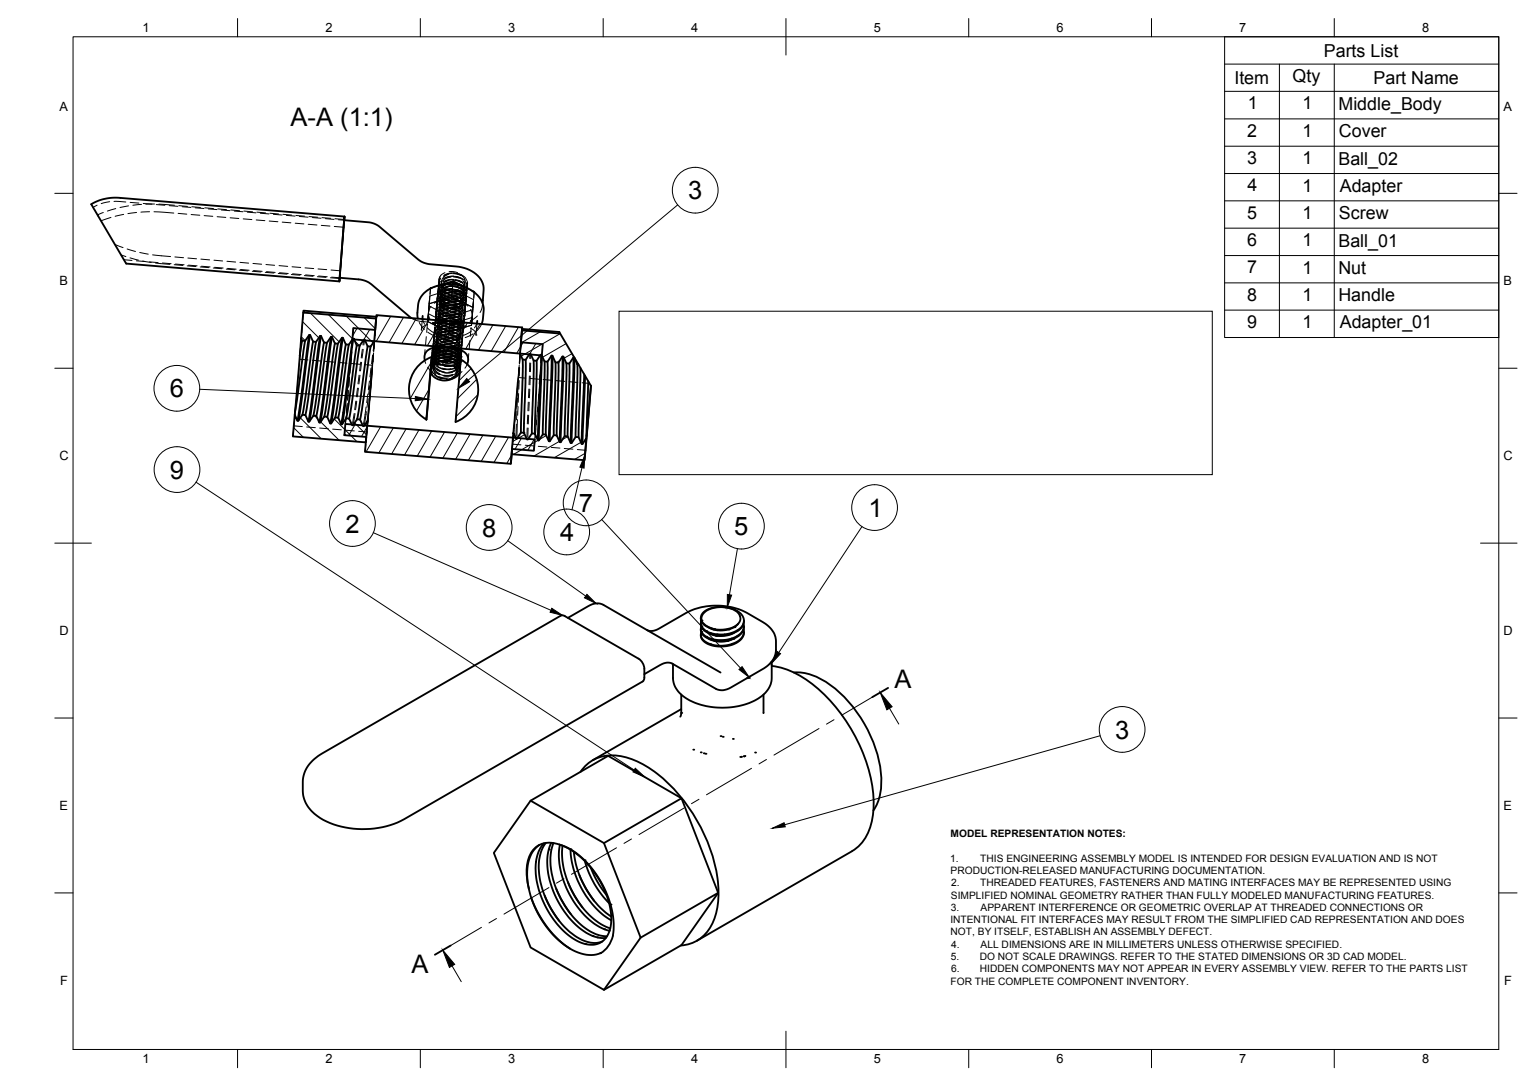
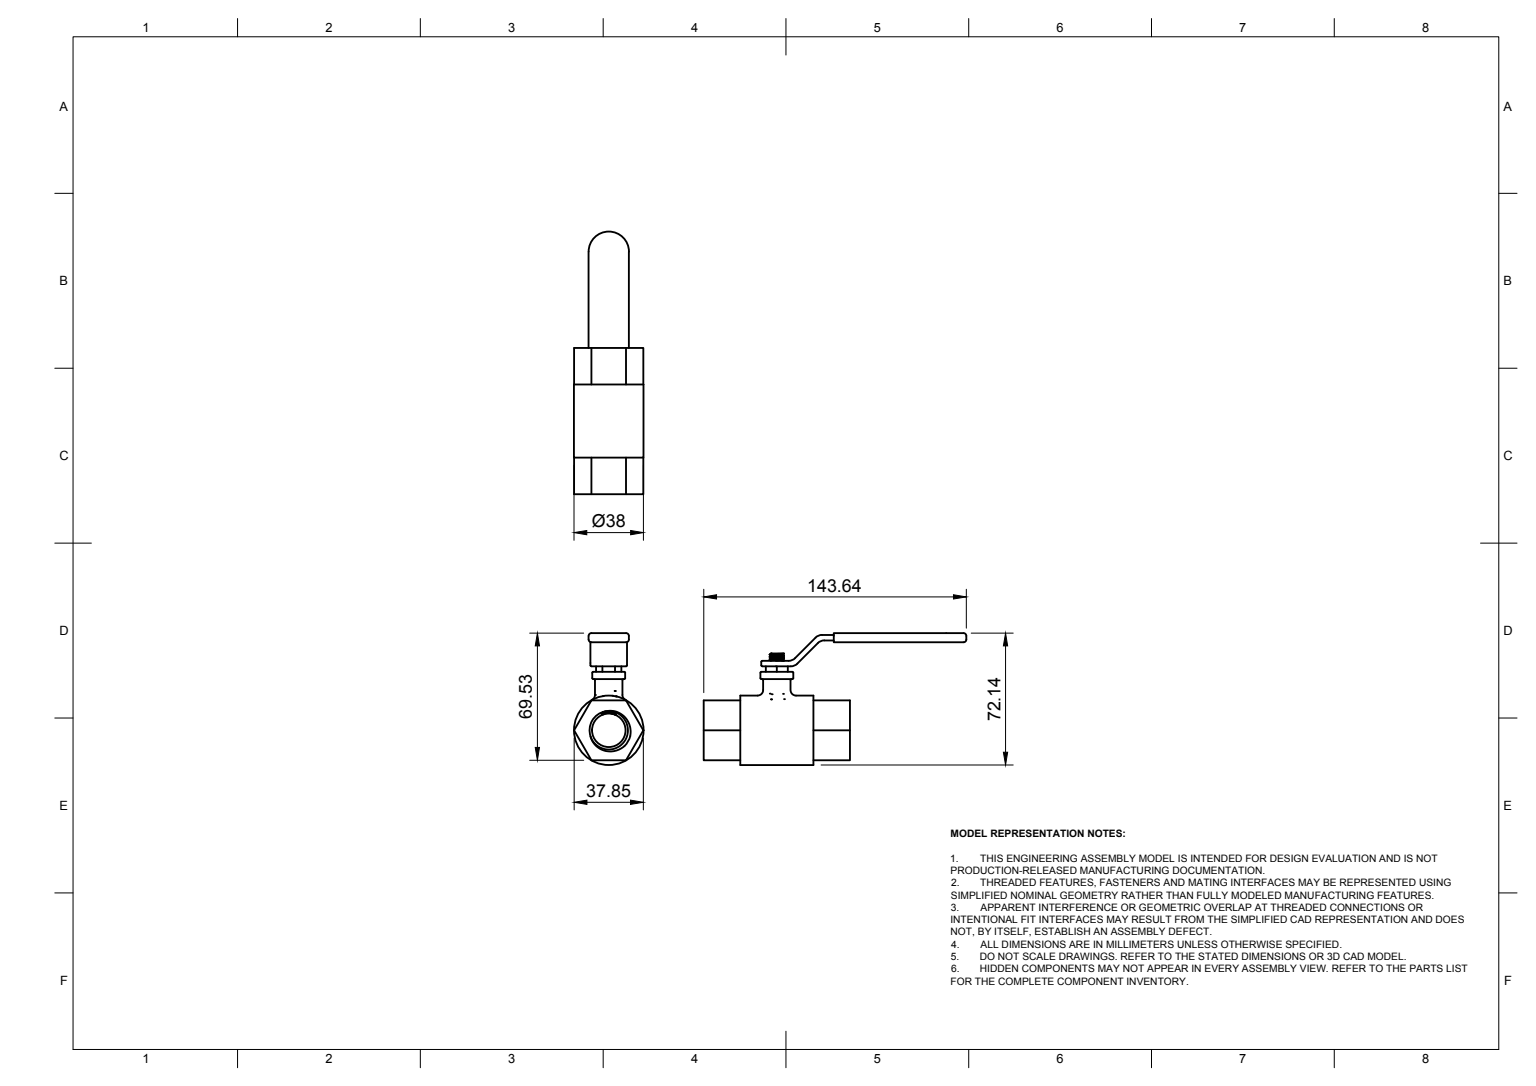
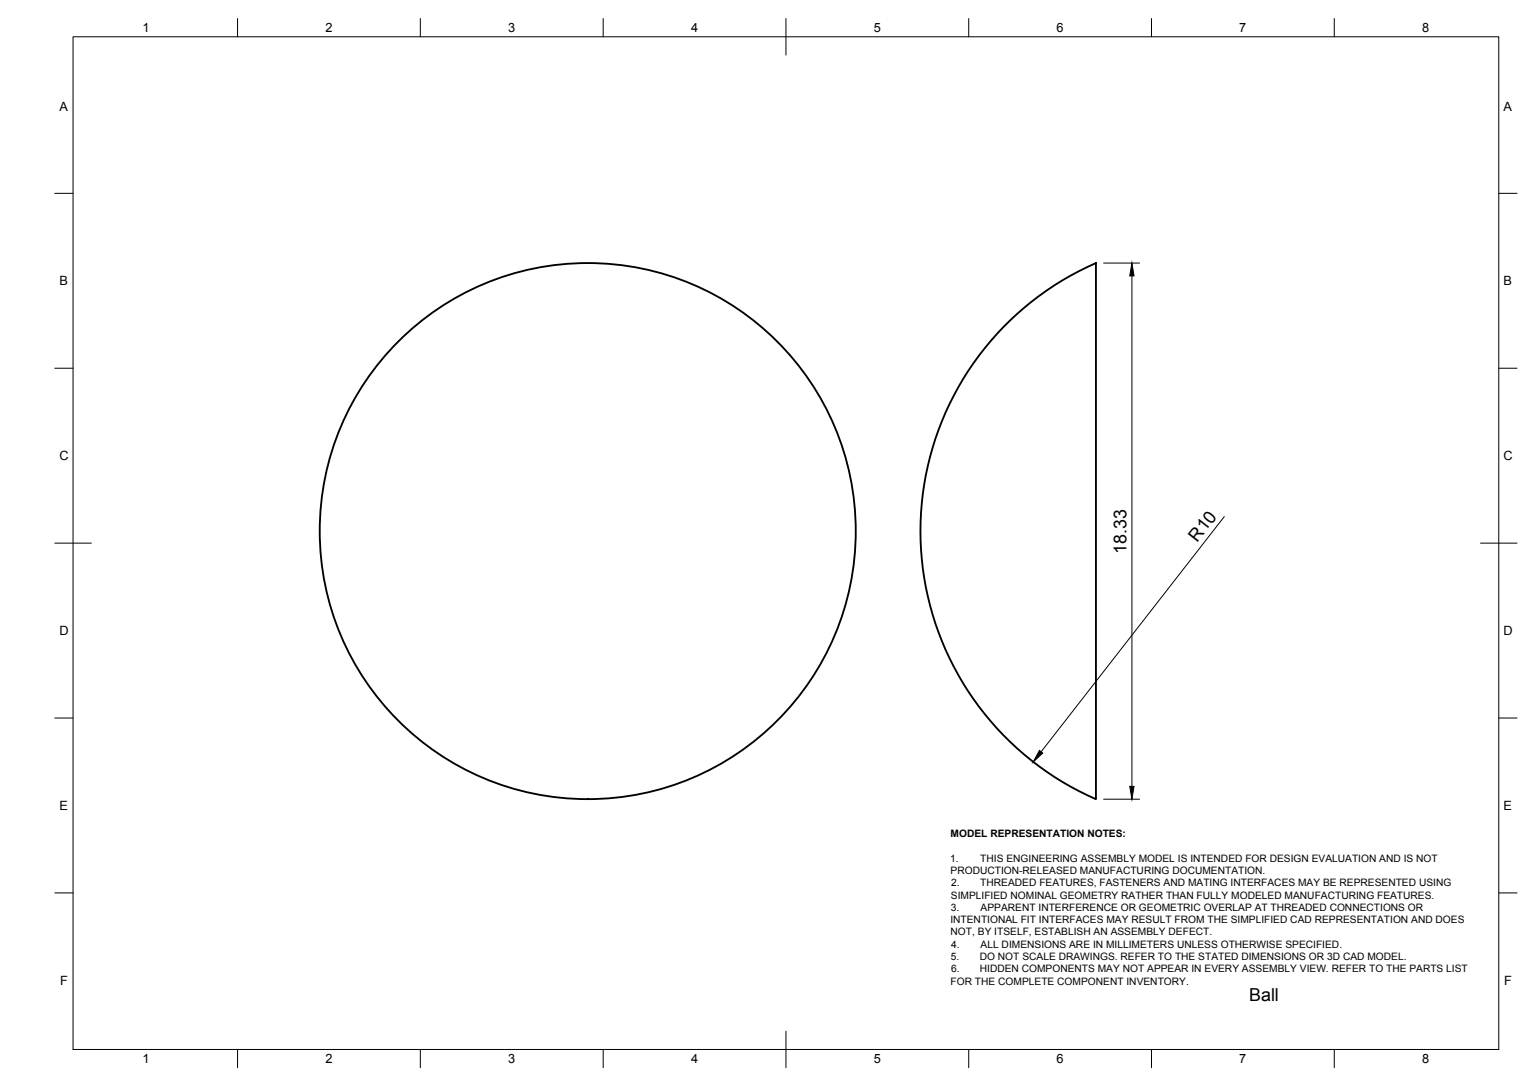
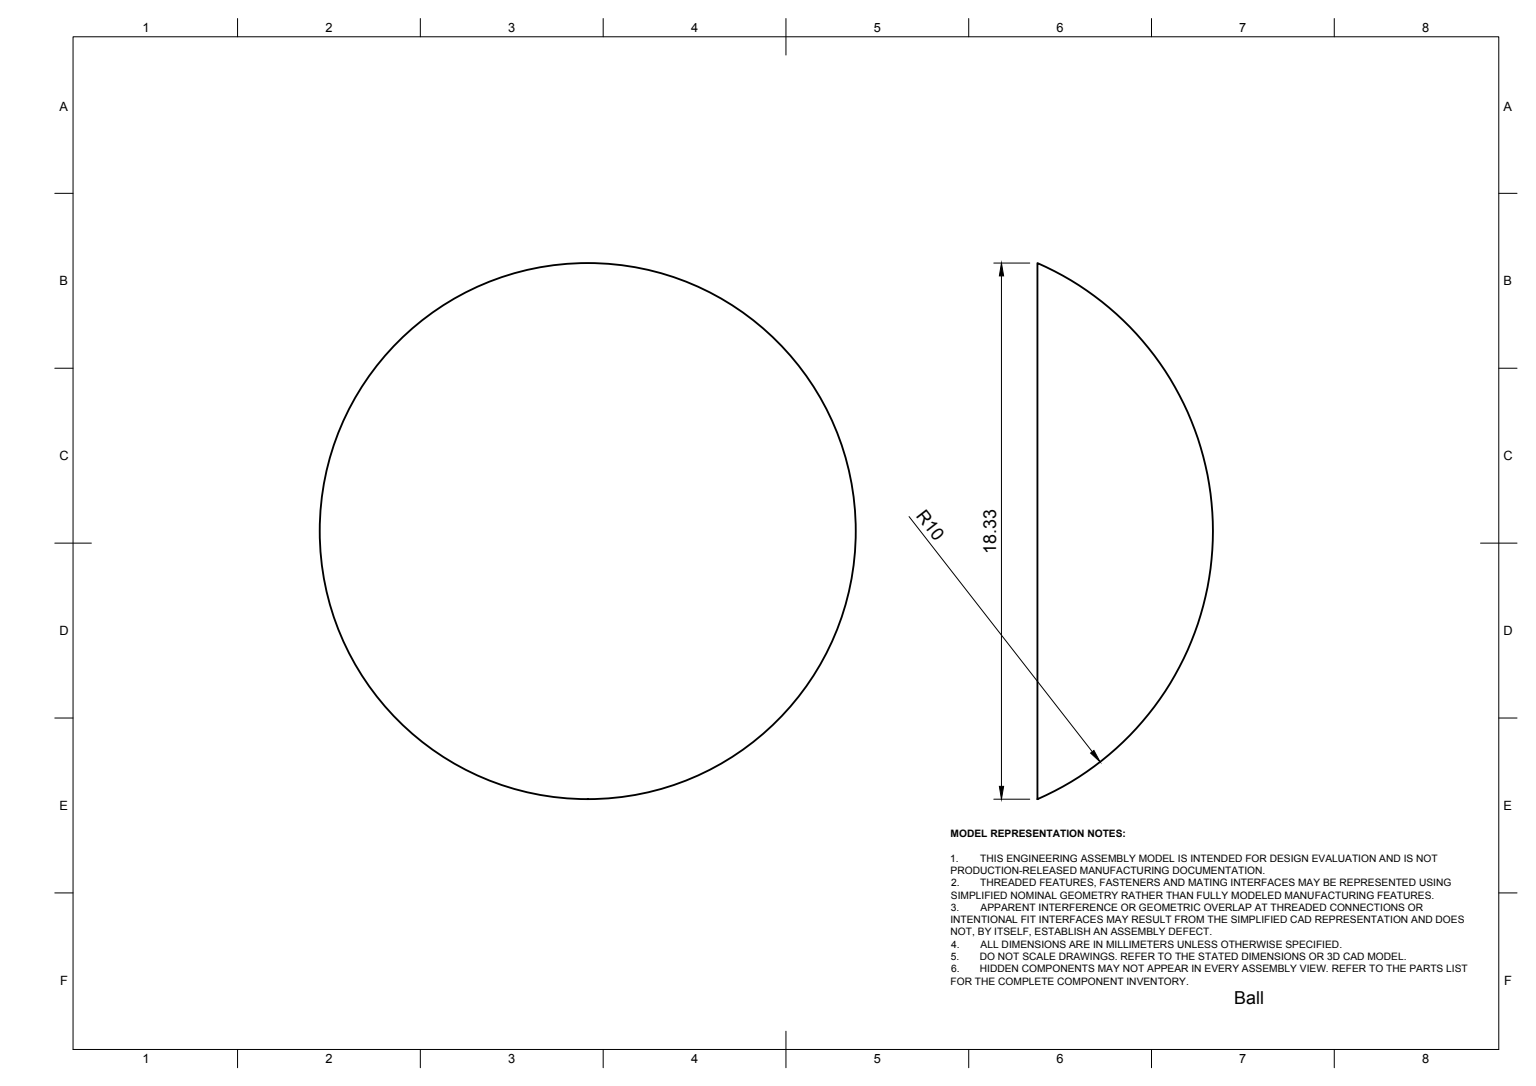
ISO-10303-21;
HEADER;
/* Generated by software containing ST-Developer
 * from STEP Tools, Inc. (www.steptools.com) 
 */

FILE_DESCRIPTION(
/* description */ (''),
/* implementation_level */ '2;1');

FILE_NAME(
/* name */ 'BR-301',
/* time_stamp */ '2026-10-06T12:47:13-07:00',
/* author */ (''),
/* organization */ (''),
/* preprocessor_version */ 'ST-DEVELOPER v20.2',
/* originating_system */ 'Autodesk Translation Framework v15.15.0.0',
/* authorisation */ '');

FILE_SCHEMA (('AUTOMOTIVE_DESIGN { 1 0 10303 214 3 1 1 }'));
ENDSEC;

DATA;
#10=MECHANICAL_DESIGN_GEOMETRIC_PRESENTATION_REPRESENTATION('',(#67,#68,
#69,#70,#71,#72,#73,#74,#75),#42667);
#11=ITEM_DEFINED_TRANSFORMATION($,$,#4142,#4459);
#12=ITEM_DEFINED_TRANSFORMATION($,$,#4196,#4460);
#13=ITEM_DEFINED_TRANSFORMATION($,$,#4231,#4461);
#14=ITEM_DEFINED_TRANSFORMATION($,$,#4235,#4462);
#15=ITEM_DEFINED_TRANSFORMATION($,$,#4264,#4463);
#16=ITEM_DEFINED_TRANSFORMATION($,$,#4301,#4464);
#17=ITEM_DEFINED_TRANSFORMATION($,$,#4305,#4465);
#18=ITEM_DEFINED_TRANSFORMATION($,$,#4317,#4466);
#19=ITEM_DEFINED_TRANSFORMATION($,$,#4430,#4467);
#20=(
REPRESENTATION_RELATIONSHIP($,$,#42702,#42701)
REPRESENTATION_RELATIONSHIP_WITH_TRANSFORMATION(#11)
SHAPE_REPRESENTATION_RELATIONSHIP()
);
#21=(
REPRESENTATION_RELATIONSHIP($,$,#42703,#42701)
REPRESENTATION_RELATIONSHIP_WITH_TRANSFORMATION(#12)
SHAPE_REPRESENTATION_RELATIONSHIP()
);
#22=(
REPRESENTATION_RELATIONSHIP($,$,#42704,#42701)
REPRESENTATION_RELATIONSHIP_WITH_TRANSFORMATION(#13)
SHAPE_REPRESENTATION_RELATIONSHIP()
);
#23=(
REPRESENTATION_RELATIONSHIP($,$,#42705,#42701)
REPRESENTATION_RELATIONSHIP_WITH_TRANSFORMATION(#14)
SHAPE_REPRESENTATION_RELATIONSHIP()
);
#24=(
REPRESENTATION_RELATIONSHIP($,$,#42706,#42701)
REPRESENTATION_RELATIONSHIP_WITH_TRANSFORMATION(#15)
SHAPE_REPRESENTATION_RELATIONSHIP()
);
#25=(
REPRESENTATION_RELATIONSHIP($,$,#42707,#42701)
REPRESENTATION_RELATIONSHIP_WITH_TRANSFORMATION(#16)
SHAPE_REPRESENTATION_RELATIONSHIP()
);
#26=(
REPRESENTATION_RELATIONSHIP($,$,#42708,#42701)
REPRESENTATION_RELATIONSHIP_WITH_TRANSFORMATION(#17)
SHAPE_REPRESENTATION_RELATIONSHIP()
);
#27=(
REPRESENTATION_RELATIONSHIP($,$,#42709,#42701)
REPRESENTATION_RELATIONSHIP_WITH_TRANSFORMATION(#18)
SHAPE_REPRESENTATION_RELATIONSHIP()
);
#28=(
REPRESENTATION_RELATIONSHIP($,$,#42710,#42701)
REPRESENTATION_RELATIONSHIP_WITH_TRANSFORMATION(#19)
SHAPE_REPRESENTATION_RELATIONSHIP()
);
#29=CONTEXT_DEPENDENT_SHAPE_REPRESENTATION(#20,#42692);
#30=CONTEXT_DEPENDENT_SHAPE_REPRESENTATION(#21,#42693);
#31=CONTEXT_DEPENDENT_SHAPE_REPRESENTATION(#22,#42694);
#32=CONTEXT_DEPENDENT_SHAPE_REPRESENTATION(#23,#42695);
#33=CONTEXT_DEPENDENT_SHAPE_REPRESENTATION(#24,#42696);
#34=CONTEXT_DEPENDENT_SHAPE_REPRESENTATION(#25,#42697);
#35=CONTEXT_DEPENDENT_SHAPE_REPRESENTATION(#26,#42698);
#36=CONTEXT_DEPENDENT_SHAPE_REPRESENTATION(#27,#42699);
#37=CONTEXT_DEPENDENT_SHAPE_REPRESENTATION(#28,#42700);
#38=NEXT_ASSEMBLY_USAGE_OCCURRENCE('Middle_Body:1','Middle_Body:1',
'Middle_Body:1',#42712,#42713,'Middle_Body:1');
#39=NEXT_ASSEMBLY_USAGE_OCCURRENCE('Cover:1','Cover:1','Cover:1',#42712,
#42714,'Cover:1');
#40=NEXT_ASSEMBLY_USAGE_OCCURRENCE('Ball_02:1','Ball_02:1','Ball_02:1',
#42712,#42715,'Ball_02:1');
#41=NEXT_ASSEMBLY_USAGE_OCCURRENCE('Adapter:1','Adapter:1','Adapter:1',
#42712,#42716,'Adapter:1');
#42=NEXT_ASSEMBLY_USAGE_OCCURRENCE('Screw:1','Screw:1','Screw:1',#42712,
#42717,'Screw:1');
#43=NEXT_ASSEMBLY_USAGE_OCCURRENCE('Ball_01:1','Ball_01:1','Ball_01:1',
#42712,#42718,'Ball_01:1');
#44=NEXT_ASSEMBLY_USAGE_OCCURRENCE('Nut:1','Nut:1','Nut:1',#42712,#42719,
'Nut:1');
#45=NEXT_ASSEMBLY_USAGE_OCCURRENCE('Handle:1','Handle:1','Handle:1',#42712,
#42720,'Handle:1');
#46=NEXT_ASSEMBLY_USAGE_OCCURRENCE('Adapter_01:1','Adapter_01:1',
'Adapter_01:1',#42712,#42721,'Adapter_01:1');
#47=SPHERICAL_SURFACE('',#4234,10.);
#48=SPHERICAL_SURFACE('',#4304,10.);
#49=SHAPE_REPRESENTATION_RELATIONSHIP('SRR','None',#42702,#58);
#50=SHAPE_REPRESENTATION_RELATIONSHIP('SRR','None',#42703,#59);
#51=SHAPE_REPRESENTATION_RELATIONSHIP('SRR','None',#42704,#60);
#52=SHAPE_REPRESENTATION_RELATIONSHIP('SRR','None',#42705,#61);
#53=SHAPE_REPRESENTATION_RELATIONSHIP('SRR','None',#42706,#62);
#54=SHAPE_REPRESENTATION_RELATIONSHIP('SRR','None',#42707,#63);
#55=SHAPE_REPRESENTATION_RELATIONSHIP('SRR','None',#42708,#64);
#56=SHAPE_REPRESENTATION_RELATIONSHIP('SRR','None',#42709,#65);
#57=SHAPE_REPRESENTATION_RELATIONSHIP('SRR','None',#42710,#66);
#58=ADVANCED_BREP_SHAPE_REPRESENTATION('',(#76),#42658);
#59=ADVANCED_BREP_SHAPE_REPRESENTATION('',(#77),#42659);
#60=ADVANCED_BREP_SHAPE_REPRESENTATION('',(#78),#42660);
#61=ADVANCED_BREP_SHAPE_REPRESENTATION('',(#79),#42661);
#62=ADVANCED_BREP_SHAPE_REPRESENTATION('',(#80),#42662);
#63=ADVANCED_BREP_SHAPE_REPRESENTATION('',(#81),#42663);
#64=ADVANCED_BREP_SHAPE_REPRESENTATION('',(#82),#42664);
#65=ADVANCED_BREP_SHAPE_REPRESENTATION('',(#83),#42665);
#66=ADVANCED_BREP_SHAPE_REPRESENTATION('',(#84),#42666);
#67=STYLED_ITEM('',(#42756),#76);
#68=STYLED_ITEM('',(#42756),#77);
#69=STYLED_ITEM('',(#42756),#78);
#70=STYLED_ITEM('',(#42756),#79);
#71=STYLED_ITEM('',(#42756),#80);
#72=STYLED_ITEM('',(#42756),#81);
#73=STYLED_ITEM('',(#42756),#82);
#74=STYLED_ITEM('',(#42756),#83);
#75=STYLED_ITEM('',(#42756),#84);
#76=MANIFOLD_SOLID_BREP('Body1',#4032);
#77=MANIFOLD_SOLID_BREP('Body1',#4033);
#78=MANIFOLD_SOLID_BREP('Body1',#4034);
#79=MANIFOLD_SOLID_BREP('Body1',#4035);
#80=MANIFOLD_SOLID_BREP('Body1',#4036);
#81=MANIFOLD_SOLID_BREP('Body1',#4037);
#82=MANIFOLD_SOLID_BREP('Body1',#4038);
#83=MANIFOLD_SOLID_BREP('Body1',#4039);
#84=MANIFOLD_SOLID_BREP('Body1',#4040);
#85=B_SPLINE_SURFACE_WITH_KNOTS('',3,3,((#5678,#5679,#5680,#5681,#5682,
#5683,#5684,#5685,#5686,#5687,#5688,#5689,#5690,#5691,#5692,#5693,#5694,
#5695),(#5696,#5697,#5698,#5699,#5700,#5701,#5702,#5703,#5704,#5705,#5706,
#5707,#5708,#5709,#5710,#5711,#5712,#5713),(#5714,#5715,#5716,#5717,#5718,
#5719,#5720,#5721,#5722,#5723,#5724,#5725,#5726,#5727,#5728,#5729,#5730,
#5731),(#5732,#5733,#5734,#5735,#5736,#5737,#5738,#5739,#5740,#5741,#5742,
#5743,#5744,#5745,#5746,#5747,#5748,#5749),(#5750,#5751,#5752,#5753,#5754,
#5755,#5756,#5757,#5758,#5759,#5760,#5761,#5762,#5763,#5764,#5765,#5766,
#5767)),.UNSPECIFIED.,.F.,.T.,.F.,(4,1,4),(4,1,1,1,1,1,1,1,1,1,1,1,1,1,
1,4),(0.,0.571428571428571,1.00004196138552),(0.,0.326770108848208,0.653540217696416,
0.980310326544624,1.30708043539283,1.52492717462497,1.96062065308925,2.17846739232139,
2.39631413155352,2.61416087078566,3.04985434924994,3.26770108848208,3.48554782771422,
3.92124130617849,4.2480114150267,4.57478152387491),.UNSPECIFIED.);
#86=B_SPLINE_SURFACE_WITH_KNOTS('',3,3,((#10429,#10430,#10431,#10432,#10433,
#10434,#10435,#10436,#10437,#10438,#10439,#10440,#10441,#10442,#10443,#10444,
#10445,#10446,#10447,#10448,#10449,#10450,#10451,#10452,#10453,#10454,#10455,
#10456,#10457,#10458,#10459,#10460,#10461,#10462,#10463,#10464,#10465,#10466,
#10467,#10468,#10469,#10470,#10471,#10472,#10473,#10474,#10475,#10476,#10477,
#10478,#10479,#10480,#10481,#10482,#10483,#10484,#10485,#10486,#10487,#10488,
#10489,#10490,#10491,#10492,#10493,#10494,#10495,#10496,#10497,#10498,#10499,
#10500,#10501,#10502,#10503,#10504,#10505,#10506,#10507,#10508,#10509,#10510,
#10511,#10512,#10513,#10514,#10515,#10516,#10517,#10518,#10519),(#10520,
#10521,#10522,#10523,#10524,#10525,#10526,#10527,#10528,#10529,#10530,#10531,
#10532,#10533,#10534,#10535,#10536,#10537,#10538,#10539,#10540,#10541,#10542,
#10543,#10544,#10545,#10546,#10547,#10548,#10549,#10550,#10551,#10552,#10553,
#10554,#10555,#10556,#10557,#10558,#10559,#10560,#10561,#10562,#10563,#10564,
#10565,#10566,#10567,#10568,#10569,#10570,#10571,#10572,#10573,#10574,#10575,
#10576,#10577,#10578,#10579,#10580,#10581,#10582,#10583,#10584,#10585,#10586,
#10587,#10588,#10589,#10590,#10591,#10592,#10593,#10594,#10595,#10596,#10597,
#10598,#10599,#10600,#10601,#10602,#10603,#10604,#10605,#10606,#10607,#10608,
#10609,#10610),(#10611,#10612,#10613,#10614,#10615,#10616,#10617,#10618,
#10619,#10620,#10621,#10622,#10623,#10624,#10625,#10626,#10627,#10628,#10629,
#10630,#10631,#10632,#10633,#10634,#10635,#10636,#10637,#10638,#10639,#10640,
#10641,#10642,#10643,#10644,#10645,#10646,#10647,#10648,#10649,#10650,#10651,
#10652,#10653,#10654,#10655,#10656,#10657,#10658,#10659,#10660,#10661,#10662,
#10663,#10664,#10665,#10666,#10667,#10668,#10669,#10670,#10671,#10672,#10673,
#10674,#10675,#10676,#10677,#10678,#10679,#10680,#10681,#10682,#10683,#10684,
#10685,#10686,#10687,#10688,#10689,#10690,#10691,#10692,#10693,#10694,#10695,
#10696,#10697,#10698,#10699,#10700,#10701),(#10702,#10703,#10704,#10705,
#10706,#10707,#10708,#10709,#10710,#10711,#10712,#10713,#10714,#10715,#10716,
#10717,#10718,#10719,#10720,#10721,#10722,#10723,#10724,#10725,#10726,#10727,
#10728,#10729,#10730,#10731,#10732,#10733,#10734,#10735,#10736,#10737,#10738,
#10739,#10740,#10741,#10742,#10743,#10744,#10745,#10746,#10747,#10748,#10749,
#10750,#10751,#10752,#10753,#10754,#10755,#10756,#10757,#10758,#10759,#10760,
#10761,#10762,#10763,#10764,#10765,#10766,#10767,#10768,#10769,#10770,#10771,
#10772,#10773,#10774,#10775,#10776,#10777,#10778,#10779,#10780,#10781,#10782,
#10783,#10784,#10785,#10786,#10787,#10788,#10789,#10790,#10791,#10792)),
 .UNSPECIFIED.,.F.,.F.,.F.,(4,4),(4,1,1,1,1,1,1,1,1,1,1,1,1,1,1,1,1,1,1,
1,1,1,1,1,1,1,1,1,1,1,1,1,1,1,1,1,1,1,1,1,1,1,1,1,1,1,1,1,1,1,1,1,1,1,1,
1,1,1,1,1,1,1,1,1,1,1,1,1,1,1,1,1,1,1,1,1,1,1,1,1,1,1,1,1,1,1,1,1,4),(-0.000129081019394602,
0.193330292353948),(11.8519068837255,12.3510302549558,12.8500245451668,
13.3490188353777,13.8480131255886,14.3470074157995,14.8460017060104,15.3449959962214,
15.8439902864323,16.3429845766432,16.8419788668541,17.3409731570651,17.839967447276,
18.3389617374869,18.8379560276978,19.3369503179088,19.8359446081197,20.3349388983306,
20.8339331885415,21.3329274787524,21.8319217689634,22.3309160591743,22.8299103493852,
23.3289046395961,23.8278989298071,24.326893220018,24.8258875102289,25.3248818004398,
25.8238760906508,26.3228703808617,26.8218646710726,27.3208589612835,27.8198532514944,
28.3188475417054,28.8178418319163,29.3168361221272,29.8158304123381,30.3148247025491,
30.81381899276,31.3128132829709,31.8118075731818,32.3108018633928,32.8097961536037,
33.3087904438146,33.8077847340255,34.3067790242364,34.8057733144474,35.3047676046583,
35.8037618948692,36.3027561850801,36.8017504752911,37.300744765502,37.7997390557129,
38.2987333459238,38.7977276361348,39.2967219263457,39.7957162165566,40.2947105067675,
40.7937047969784,41.2926990871894,41.7916933774003,42.2906876676112,42.7896819578221,
43.2886762480331,43.787670538244,44.2866648284549,44.7856591186658,45.2846534088767,
45.7836476990877,46.2826419892986,46.7816362795095,47.2806305697204,47.7796248599314,
48.2786191501423,48.7776134403532,49.2766077305641,49.7756020207751,50.274596310986,
50.7735906011969,51.2725848914078,51.7715791816187,52.2705734718297,52.7695677620406,
53.2685620522515,53.7675563424624,54.2665506326734,54.7655449228843,55.2645392130952,
55.7635335033061),.UNSPECIFIED.);
#87=B_SPLINE_SURFACE_WITH_KNOTS('',3,3,((#11034,#11035,#11036,#11037,#11038,
#11039,#11040,#11041,#11042,#11043,#11044,#11045,#11046,#11047,#11048,#11049,
#11050,#11051,#11052,#11053,#11054,#11055,#11056,#11057,#11058,#11059,#11060,
#11061,#11062,#11063,#11064,#11065,#11066,#11067,#11068,#11069,#11070,#11071,
#11072,#11073,#11074,#11075,#11076,#11077,#11078,#11079,#11080,#11081,#11082,
#11083,#11084,#11085,#11086,#11087,#11088,#11089,#11090,#11091,#11092,#11093,
#11094,#11095,#11096,#11097,#11098,#11099,#11100,#11101,#11102,#11103,#11104,
#11105,#11106,#11107,#11108,#11109,#11110,#11111,#11112,#11113,#11114,#11115,
#11116,#11117,#11118,#11119,#11120,#11121,#11122,#11123,#11124),(#11125,
#11126,#11127,#11128,#11129,#11130,#11131,#11132,#11133,#11134,#11135,#11136,
#11137,#11138,#11139,#11140,#11141,#11142,#11143,#11144,#11145,#11146,#11147,
#11148,#11149,#11150,#11151,#11152,#11153,#11154,#11155,#11156,#11157,#11158,
#11159,#11160,#11161,#11162,#11163,#11164,#11165,#11166,#11167,#11168,#11169,
#11170,#11171,#11172,#11173,#11174,#11175,#11176,#11177,#11178,#11179,#11180,
#11181,#11182,#11183,#11184,#11185,#11186,#11187,#11188,#11189,#11190,#11191,
#11192,#11193,#11194,#11195,#11196,#11197,#11198,#11199,#11200,#11201,#11202,
#11203,#11204,#11205,#11206,#11207,#11208,#11209,#11210,#11211,#11212,#11213,
#11214,#11215),(#11216,#11217,#11218,#11219,#11220,#11221,#11222,#11223,
#11224,#11225,#11226,#11227,#11228,#11229,#11230,#11231,#11232,#11233,#11234,
#11235,#11236,#11237,#11238,#11239,#11240,#11241,#11242,#11243,#11244,#11245,
#11246,#11247,#11248,#11249,#11250,#11251,#11252,#11253,#11254,#11255,#11256,
#11257,#11258,#11259,#11260,#11261,#11262,#11263,#11264,#11265,#11266,#11267,
#11268,#11269,#11270,#11271,#11272,#11273,#11274,#11275,#11276,#11277,#11278,
#11279,#11280,#11281,#11282,#11283,#11284,#11285,#11286,#11287,#11288,#11289,
#11290,#11291,#11292,#11293,#11294,#11295,#11296,#11297,#11298,#11299,#11300,
#11301,#11302,#11303,#11304,#11305,#11306),(#11307,#11308,#11309,#11310,
#11311,#11312,#11313,#11314,#11315,#11316,#11317,#11318,#11319,#11320,#11321,
#11322,#11323,#11324,#11325,#11326,#11327,#11328,#11329,#11330,#11331,#11332,
#11333,#11334,#11335,#11336,#11337,#11338,#11339,#11340,#11341,#11342,#11343,
#11344,#11345,#11346,#11347,#11348,#11349,#11350,#11351,#11352,#11353,#11354,
#11355,#11356,#11357,#11358,#11359,#11360,#11361,#11362,#11363,#11364,#11365,
#11366,#11367,#11368,#11369,#11370,#11371,#11372,#11373,#11374,#11375,#11376,
#11377,#11378,#11379,#11380,#11381,#11382,#11383,#11384,#11385,#11386,#11387,
#11388,#11389,#11390,#11391,#11392,#11393,#11394,#11395,#11396,#11397)),
 .UNSPECIFIED.,.F.,.F.,.F.,(4,4),(4,1,1,1,1,1,1,1,1,1,1,1,1,1,1,1,1,1,1,
1,1,1,1,1,1,1,1,1,1,1,1,1,1,1,1,1,1,1,1,1,1,1,1,1,1,1,1,1,1,1,1,1,1,1,1,
1,1,1,1,1,1,1,1,1,1,1,1,1,1,1,1,1,1,1,1,1,1,1,1,1,1,1,1,1,1,1,1,1,4),(-9.09719654654513E-5,
0.1933682374602),(14.3987024268659,14.8976967170768,15.3966910072877,15.8956852974986,
16.3946795877096,16.8936738779205,17.3926681681314,17.8916624583423,18.3906567485533,
18.8896510387642,19.3886453289751,19.887639619186,20.386633909397,20.8856281996079,
21.3846224898188,21.8836167800297,22.3826110702406,22.8816053604516,23.3805996506625,
23.8795939408734,24.3785882310843,24.8775825212953,25.3765768115062,25.8755711017171,
26.374565391928,26.8735596821389,27.3725539723499,27.8715482625608,28.3705425527717,
28.8695368429826,29.3685311331936,29.8675254234045,30.3665197136154,30.8655140038263,
31.3645082940373,31.8635025842482,32.3624968744591,32.86149116467,33.3604854548809,
33.8594797450919,34.3584740353028,34.8574683255137,35.3564626157246,35.8554569059356,
36.3544511961465,36.8534454863574,37.3524397765683,37.8514340667792,38.3504283569902,
38.8494226472011,39.348416937412,39.8474112276229,40.3464055178339,40.8453998080448,
41.3443940982557,41.8433883884666,42.3423826786776,42.8413769688885,43.3403712590994,
43.8393655493103,44.3383598395212,44.8373541297322,45.3363484199431,45.835342710154,
46.3343370003649,46.8333312905759,47.3323255807868,47.8313198709977,48.3303141612086,
48.8293084514195,49.3283027416305,49.8272970318414,50.3262913220523,50.8252856122632,
51.3242799024742,51.8232741926851,52.322268482896,52.8212627731069,53.3202570633179,
53.8192513535288,54.3182456437397,54.8172399339506,55.3162342241615,55.8152285143725,
56.3142228045834,56.8132170947943,57.3122113850052,57.8112056752162,58.3103290677895),
 .UNSPECIFIED.);
#88=B_SPLINE_SURFACE_WITH_KNOTS('',3,3,((#31748,#31749,#31750,#31751,#31752,
#31753,#31754,#31755,#31756,#31757,#31758,#31759,#31760,#31761,#31762,#31763,
#31764,#31765,#31766,#31767,#31768,#31769,#31770,#31771,#31772,#31773,#31774,
#31775,#31776,#31777,#31778,#31779,#31780,#31781,#31782,#31783,#31784,#31785,
#31786,#31787,#31788,#31789,#31790,#31791,#31792,#31793,#31794,#31795,#31796,
#31797,#31798,#31799,#31800,#31801,#31802,#31803,#31804,#31805,#31806,#31807,
#31808,#31809,#31810,#31811,#31812,#31813,#31814,#31815,#31816,#31817,#31818,
#31819,#31820,#31821,#31822,#31823,#31824,#31825,#31826,#31827,#31828,#31829,
#31830,#31831,#31832,#31833,#31834,#31835,#31836,#31837,#31838,#31839,#31840,
#31841,#31842,#31843,#31844,#31845,#31846,#31847,#31848,#31849,#31850,#31851,
#31852,#31853,#31854,#31855,#31856,#31857,#31858,#31859,#31860,#31861,#31862,
#31863,#31864,#31865,#31866,#31867,#31868,#31869,#31870,#31871,#31872,#31873,
#31874,#31875,#31876,#31877,#31878,#31879,#31880,#31881,#31882,#31883,#31884,
#31885,#31886,#31887,#31888,#31889,#31890,#31891,#31892,#31893,#31894,#31895,
#31896,#31897,#31898,#31899,#31900,#31901,#31902,#31903,#31904,#31905,#31906,
#31907,#31908,#31909,#31910,#31911,#31912,#31913,#31914,#31915,#31916,#31917,
#31918,#31919,#31920,#31921,#31922,#31923,#31924,#31925,#31926,#31927,#31928),
(#31929,#31930,#31931,#31932,#31933,#31934,#31935,#31936,#31937,#31938,
#31939,#31940,#31941,#31942,#31943,#31944,#31945,#31946,#31947,#31948,#31949,
#31950,#31951,#31952,#31953,#31954,#31955,#31956,#31957,#31958,#31959,#31960,
#31961,#31962,#31963,#31964,#31965,#31966,#31967,#31968,#31969,#31970,#31971,
#31972,#31973,#31974,#31975,#31976,#31977,#31978,#31979,#31980,#31981,#31982,
#31983,#31984,#31985,#31986,#31987,#31988,#31989,#31990,#31991,#31992,#31993,
#31994,#31995,#31996,#31997,#31998,#31999,#32000,#32001,#32002,#32003,#32004,
#32005,#32006,#32007,#32008,#32009,#32010,#32011,#32012,#32013,#32014,#32015,
#32016,#32017,#32018,#32019,#32020,#32021,#32022,#32023,#32024,#32025,#32026,
#32027,#32028,#32029,#32030,#32031,#32032,#32033,#32034,#32035,#32036,#32037,
#32038,#32039,#32040,#32041,#32042,#32043,#32044,#32045,#32046,#32047,#32048,
#32049,#32050,#32051,#32052,#32053,#32054,#32055,#32056,#32057,#32058,#32059,
#32060,#32061,#32062,#32063,#32064,#32065,#32066,#32067,#32068,#32069,#32070,
#32071,#32072,#32073,#32074,#32075,#32076,#32077,#32078,#32079,#32080,#32081,
#32082,#32083,#32084,#32085,#32086,#32087,#32088,#32089,#32090,#32091,#32092,
#32093,#32094,#32095,#32096,#32097,#32098,#32099,#32100,#32101,#32102,#32103,
#32104,#32105,#32106,#32107,#32108,#32109),(#32110,#32111,#32112,#32113,
#32114,#32115,#32116,#32117,#32118,#32119,#32120,#32121,#32122,#32123,#32124,
#32125,#32126,#32127,#32128,#32129,#32130,#32131,#32132,#32133,#32134,#32135,
#32136,#32137,#32138,#32139,#32140,#32141,#32142,#32143,#32144,#32145,#32146,
#32147,#32148,#32149,#32150,#32151,#32152,#32153,#32154,#32155,#32156,#32157,
#32158,#32159,#32160,#32161,#32162,#32163,#32164,#32165,#32166,#32167,#32168,
#32169,#32170,#32171,#32172,#32173,#32174,#32175,#32176,#32177,#32178,#32179,
#32180,#32181,#32182,#32183,#32184,#32185,#32186,#32187,#32188,#32189,#32190,
#32191,#32192,#32193,#32194,#32195,#32196,#32197,#32198,#32199,#32200,#32201,
#32202,#32203,#32204,#32205,#32206,#32207,#32208,#32209,#32210,#32211,#32212,
#32213,#32214,#32215,#32216,#32217,#32218,#32219,#32220,#32221,#32222,#32223,
#32224,#32225,#32226,#32227,#32228,#32229,#32230,#32231,#32232,#32233,#32234,
#32235,#32236,#32237,#32238,#32239,#32240,#32241,#32242,#32243,#32244,#32245,
#32246,#32247,#32248,#32249,#32250,#32251,#32252,#32253,#32254,#32255,#32256,
#32257,#32258,#32259,#32260,#32261,#32262,#32263,#32264,#32265,#32266,#32267,
#32268,#32269,#32270,#32271,#32272,#32273,#32274,#32275,#32276,#32277,#32278,
#32279,#32280,#32281,#32282,#32283,#32284,#32285,#32286,#32287,#32288,#32289,
#32290),(#32291,#32292,#32293,#32294,#32295,#32296,#32297,#32298,#32299,
#32300,#32301,#32302,#32303,#32304,#32305,#32306,#32307,#32308,#32309,#32310,
#32311,#32312,#32313,#32314,#32315,#32316,#32317,#32318,#32319,#32320,#32321,
#32322,#32323,#32324,#32325,#32326,#32327,#32328,#32329,#32330,#32331,#32332,
#32333,#32334,#32335,#32336,#32337,#32338,#32339,#32340,#32341,#32342,#32343,
#32344,#32345,#32346,#32347,#32348,#32349,#32350,#32351,#32352,#32353,#32354,
#32355,#32356,#32357,#32358,#32359,#32360,#32361,#32362,#32363,#32364,#32365,
#32366,#32367,#32368,#32369,#32370,#32371,#32372,#32373,#32374,#32375,#32376,
#32377,#32378,#32379,#32380,#32381,#32382,#32383,#32384,#32385,#32386,#32387,
#32388,#32389,#32390,#32391,#32392,#32393,#32394,#32395,#32396,#32397,#32398,
#32399,#32400,#32401,#32402,#32403,#32404,#32405,#32406,#32407,#32408,#32409,
#32410,#32411,#32412,#32413,#32414,#32415,#32416,#32417,#32418,#32419,#32420,
#32421,#32422,#32423,#32424,#32425,#32426,#32427,#32428,#32429,#32430,#32431,
#32432,#32433,#32434,#32435,#32436,#32437,#32438,#32439,#32440,#32441,#32442,
#32443,#32444,#32445,#32446,#32447,#32448,#32449,#32450,#32451,#32452,#32453,
#32454,#32455,#32456,#32457,#32458,#32459,#32460,#32461,#32462,#32463,#32464,
#32465,#32466,#32467,#32468,#32469,#32470,#32471)),.UNSPECIFIED.,.F.,.F.,
 .F.,(4,4),(4,1,1,1,1,1,1,1,1,1,1,1,1,1,1,1,1,1,1,1,1,1,1,1,1,1,1,1,1,1,
1,1,1,1,1,1,1,1,1,1,1,1,1,1,1,1,1,1,1,1,1,1,1,1,1,1,1,1,1,1,1,1,1,1,1,1,
1,1,1,1,1,1,1,1,1,1,1,1,1,1,1,1,1,1,1,1,1,1,1,1,1,1,1,1,1,1,1,1,1,1,1,1,
1,1,1,1,1,1,1,1,1,1,1,1,1,1,1,1,1,1,1,1,1,1,1,1,1,1,1,1,1,1,1,1,1,1,1,1,
1,1,1,1,1,1,1,1,1,1,1,1,1,1,1,1,1,1,1,1,1,1,1,1,1,1,1,1,1,1,1,1,1,1,1,1,
1,1,1,1,4),(-0.000650925100349628,0.0823958707828885),(8.31473274985812,
9.3146787622095,10.3146247745609,11.3145707869122,12.3145167992636,13.314462811615,
14.3144088239664,15.3143548363177,16.3143008486691,17.3142468610205,18.3141928733718,
19.3141388857232,20.3140848980746,21.314030910426,22.3139769227773,23.3139229351287,
24.3138689474801,25.3138149598315,26.3137609721828,27.3137069845342,28.3136529968856,
29.3135990092369,30.3135450215883,31.3134910339397,32.3134370462911,33.3133830586424,
34.3133290709938,35.3132750833452,36.3132210956965,37.3131671080479,38.3131131203993,
39.3130591327507,40.313005145102,41.3129511574534,42.3128971698048,43.3128431821562,
44.3127891945075,45.3127352068589,46.3126812192103,47.3126272315616,48.312573243913,
49.3125192562644,50.3124652686158,51.3124112809671,52.3123572933185,53.3123033056699,
54.3122493180213,55.3121953303726,56.312141342724,57.3120873550754,58.3120333674267,
59.3119793797781,60.3119253921295,61.3118714044809,62.3118174168322,63.3117634291836,
64.311709441535,65.3116554538863,66.3116014662377,67.3115474785891,68.3114934909405,
69.3114395032918,70.3113855156432,71.3113315279946,72.311277540346,73.3112235526973,
74.3111695650487,75.3111155774001,76.3110615897514,77.3110076021028,78.3109536144542,
79.3108996268056,80.3108456391569,81.3107916515083,82.3107376638597,83.3106836762111,
84.3106296885624,85.3105757009138,86.3105217132652,87.3104677256165,88.3104137379679,
89.3103597503193,90.3103057626707,91.310251775022,92.3101977873734,93.3101437997248,
94.3100898120761,95.3100358244275,96.3099818367789,97.3099278491303,98.3098738614816,
99.309819873833,100.309765886184,101.309711898536,102.309657910887,103.309603923238,
104.30954993559,105.309495947941,106.309441960293,107.309387972644,108.309333984995,
109.309279997347,110.309226009698,111.309172022049,112.309118034401,113.309064046752,
114.309010059104,115.308956071455,116.308902083806,117.308848096158,118.308794108509,
119.30874012086,120.308686133212,121.308632145563,122.308578157915,123.308524170266,
124.308470182617,125.308416194969,126.30836220732,127.308308219671,128.308254232023,
129.308200244374,130.308146256726,131.308092269077,132.308038281428,133.30798429378,
134.307930306131,135.307876318482,136.307822330834,137.307768343185,138.307714355537,
139.307660367888,140.307606380239,141.307552392591,142.307498404942,143.307444417293,
144.307390429645,145.307336441996,146.307282454348,147.307228466699,148.30717447905,
149.307120491402,150.307066503753,151.307012516104,152.306958528456,153.306904540807,
154.306850553158,155.30679656551,156.306742577861,157.306688590213,158.306634602564,
159.306580614915,160.306526627267,161.306472639618,162.306418651969,163.306364664321,
164.306310676672,165.306256689024,166.306202701375,167.306148713726,168.306094726078,
169.306040738429,170.30598675078,171.305932763132,172.305878775483,173.305824787835,
174.305770800186,175.305716812537,176.305662824889,177.30560883724,178.305554849591,
179.305500861943,180.305446874294,181.305392886646,182.305338898997,183.305284911348,
184.3052309237,185.305176936051,186.305773873502),.UNSPECIFIED.);
#89=B_SPLINE_SURFACE_WITH_KNOTS('',3,3,((#32657,#32658,#32659,#32660,#32661,
#32662,#32663,#32664,#32665,#32666,#32667,#32668,#32669,#32670,#32671,#32672,
#32673,#32674,#32675,#32676,#32677,#32678,#32679,#32680,#32681,#32682,#32683,
#32684,#32685,#32686,#32687,#32688,#32689,#32690,#32691,#32692,#32693,#32694,
#32695,#32696,#32697,#32698,#32699,#32700,#32701,#32702,#32703,#32704,#32705,
#32706,#32707,#32708,#32709,#32710,#32711,#32712,#32713,#32714,#32715,#32716,
#32717,#32718,#32719,#32720,#32721,#32722,#32723,#32724,#32725,#32726,#32727,
#32728,#32729,#32730,#32731,#32732,#32733,#32734,#32735,#32736,#32737,#32738,
#32739,#32740,#32741,#32742,#32743,#32744,#32745,#32746,#32747,#32748,#32749,
#32750,#32751,#32752,#32753,#32754,#32755,#32756,#32757,#32758,#32759,#32760,
#32761,#32762,#32763,#32764,#32765,#32766,#32767,#32768,#32769,#32770,#32771,
#32772,#32773,#32774,#32775,#32776,#32777,#32778,#32779,#32780,#32781,#32782,
#32783,#32784,#32785,#32786,#32787,#32788,#32789,#32790,#32791,#32792,#32793,
#32794,#32795,#32796,#32797,#32798,#32799,#32800,#32801,#32802,#32803,#32804,
#32805,#32806,#32807,#32808,#32809,#32810,#32811,#32812,#32813,#32814,#32815,
#32816,#32817,#32818,#32819,#32820,#32821,#32822,#32823,#32824,#32825,#32826,
#32827,#32828,#32829,#32830,#32831,#32832,#32833,#32834,#32835,#32836,#32837),
(#32838,#32839,#32840,#32841,#32842,#32843,#32844,#32845,#32846,#32847,
#32848,#32849,#32850,#32851,#32852,#32853,#32854,#32855,#32856,#32857,#32858,
#32859,#32860,#32861,#32862,#32863,#32864,#32865,#32866,#32867,#32868,#32869,
#32870,#32871,#32872,#32873,#32874,#32875,#32876,#32877,#32878,#32879,#32880,
#32881,#32882,#32883,#32884,#32885,#32886,#32887,#32888,#32889,#32890,#32891,
#32892,#32893,#32894,#32895,#32896,#32897,#32898,#32899,#32900,#32901,#32902,
#32903,#32904,#32905,#32906,#32907,#32908,#32909,#32910,#32911,#32912,#32913,
#32914,#32915,#32916,#32917,#32918,#32919,#32920,#32921,#32922,#32923,#32924,
#32925,#32926,#32927,#32928,#32929,#32930,#32931,#32932,#32933,#32934,#32935,
#32936,#32937,#32938,#32939,#32940,#32941,#32942,#32943,#32944,#32945,#32946,
#32947,#32948,#32949,#32950,#32951,#32952,#32953,#32954,#32955,#32956,#32957,
#32958,#32959,#32960,#32961,#32962,#32963,#32964,#32965,#32966,#32967,#32968,
#32969,#32970,#32971,#32972,#32973,#32974,#32975,#32976,#32977,#32978,#32979,
#32980,#32981,#32982,#32983,#32984,#32985,#32986,#32987,#32988,#32989,#32990,
#32991,#32992,#32993,#32994,#32995,#32996,#32997,#32998,#32999,#33000,#33001,
#33002,#33003,#33004,#33005,#33006,#33007,#33008,#33009,#33010,#33011,#33012,
#33013,#33014,#33015,#33016,#33017,#33018),(#33019,#33020,#33021,#33022,
#33023,#33024,#33025,#33026,#33027,#33028,#33029,#33030,#33031,#33032,#33033,
#33034,#33035,#33036,#33037,#33038,#33039,#33040,#33041,#33042,#33043,#33044,
#33045,#33046,#33047,#33048,#33049,#33050,#33051,#33052,#33053,#33054,#33055,
#33056,#33057,#33058,#33059,#33060,#33061,#33062,#33063,#33064,#33065,#33066,
#33067,#33068,#33069,#33070,#33071,#33072,#33073,#33074,#33075,#33076,#33077,
#33078,#33079,#33080,#33081,#33082,#33083,#33084,#33085,#33086,#33087,#33088,
#33089,#33090,#33091,#33092,#33093,#33094,#33095,#33096,#33097,#33098,#33099,
#33100,#33101,#33102,#33103,#33104,#33105,#33106,#33107,#33108,#33109,#33110,
#33111,#33112,#33113,#33114,#33115,#33116,#33117,#33118,#33119,#33120,#33121,
#33122,#33123,#33124,#33125,#33126,#33127,#33128,#33129,#33130,#33131,#33132,
#33133,#33134,#33135,#33136,#33137,#33138,#33139,#33140,#33141,#33142,#33143,
#33144,#33145,#33146,#33147,#33148,#33149,#33150,#33151,#33152,#33153,#33154,
#33155,#33156,#33157,#33158,#33159,#33160,#33161,#33162,#33163,#33164,#33165,
#33166,#33167,#33168,#33169,#33170,#33171,#33172,#33173,#33174,#33175,#33176,
#33177,#33178,#33179,#33180,#33181,#33182,#33183,#33184,#33185,#33186,#33187,
#33188,#33189,#33190,#33191,#33192,#33193,#33194,#33195,#33196,#33197,#33198,
#33199),(#33200,#33201,#33202,#33203,#33204,#33205,#33206,#33207,#33208,
#33209,#33210,#33211,#33212,#33213,#33214,#33215,#33216,#33217,#33218,#33219,
#33220,#33221,#33222,#33223,#33224,#33225,#33226,#33227,#33228,#33229,#33230,
#33231,#33232,#33233,#33234,#33235,#33236,#33237,#33238,#33239,#33240,#33241,
#33242,#33243,#33244,#33245,#33246,#33247,#33248,#33249,#33250,#33251,#33252,
#33253,#33254,#33255,#33256,#33257,#33258,#33259,#33260,#33261,#33262,#33263,
#33264,#33265,#33266,#33267,#33268,#33269,#33270,#33271,#33272,#33273,#33274,
#33275,#33276,#33277,#33278,#33279,#33280,#33281,#33282,#33283,#33284,#33285,
#33286,#33287,#33288,#33289,#33290,#33291,#33292,#33293,#33294,#33295,#33296,
#33297,#33298,#33299,#33300,#33301,#33302,#33303,#33304,#33305,#33306,#33307,
#33308,#33309,#33310,#33311,#33312,#33313,#33314,#33315,#33316,#33317,#33318,
#33319,#33320,#33321,#33322,#33323,#33324,#33325,#33326,#33327,#33328,#33329,
#33330,#33331,#33332,#33333,#33334,#33335,#33336,#33337,#33338,#33339,#33340,
#33341,#33342,#33343,#33344,#33345,#33346,#33347,#33348,#33349,#33350,#33351,
#33352,#33353,#33354,#33355,#33356,#33357,#33358,#33359,#33360,#33361,#33362,
#33363,#33364,#33365,#33366,#33367,#33368,#33369,#33370,#33371,#33372,#33373,
#33374,#33375,#33376,#33377,#33378,#33379,#33380)),.UNSPECIFIED.,.F.,.F.,
 .F.,(4,4),(4,1,1,1,1,1,1,1,1,1,1,1,1,1,1,1,1,1,1,1,1,1,1,1,1,1,1,1,1,1,
1,1,1,1,1,1,1,1,1,1,1,1,1,1,1,1,1,1,1,1,1,1,1,1,1,1,1,1,1,1,1,1,1,1,1,1,
1,1,1,1,1,1,1,1,1,1,1,1,1,1,1,1,1,1,1,1,1,1,1,1,1,1,1,1,1,1,1,1,1,1,1,1,
1,1,1,1,1,1,1,1,1,1,1,1,1,1,1,1,1,1,1,1,1,1,1,1,1,1,1,1,1,1,1,1,1,1,1,1,
1,1,1,1,1,1,1,1,1,1,1,1,1,1,1,1,1,1,1,1,1,1,1,1,1,1,1,1,1,1,1,1,1,1,1,1,
1,1,1,1,4),(-0.00033399260015787,0.082683618112034),(11.6145432153813,12.6151602401062,
13.6151062524576,14.615052264809,15.6149982771603,16.6149442895117,17.6148903018631,
18.6148363142145,19.6147823265658,20.6147283389172,21.6146743512686,22.61462036362,
23.6145663759713,24.6145123883227,25.6144584006741,26.6144044130254,27.6143504253768,
28.6142964377282,29.6142424500796,30.6141884624309,31.6141344747823,32.6140804871337,
33.614026499485,34.6139725118364,35.6139185241878,36.6138645365392,37.6138105488905,
38.6137565612419,39.6137025735933,40.6136485859447,41.613594598296,42.6135406106474,
43.6134866229988,44.6134326353501,45.6133786477015,46.6133246600529,47.6132706724043,
48.6132166847556,49.613162697107,50.6131087094584,51.6130547218097,52.6130007341611,
53.6129467465125,54.6128927588639,55.6128387712152,56.6127847835666,57.612730795918,
58.6126768082694,59.6126228206207,60.6125688329721,61.6125148453235,62.6124608576748,
63.6124068700262,64.6123528823776,65.612298894729,66.6122449070803,67.6121909194317,
68.6121369317831,69.6120829441344,70.6120289564858,71.6119749688372,72.6119209811886,
73.6118669935399,74.6118130058913,75.6117590182427,76.6117050305941,77.6116510429454,
78.6115970552968,79.6115430676482,80.6114890799995,81.6114350923509,82.6113811047023,
83.6113271170537,84.611273129405,85.6112191417564,86.6111651541078,87.6111111664591,
88.6110571788105,89.6110031911619,90.6109492035133,91.6108952158646,92.610841228216,
93.6107872405674,94.6107332529187,95.6106792652701,96.6106252776215,97.6105712899729,
98.6105173023242,99.6104633146756,100.610409327027,101.610355339378,102.61030135173,
103.610247364081,104.610193376432,105.610139388784,106.610085401135,107.610031413487,
108.609977425838,109.609923438189,110.609869450541,111.609815462892,112.609761475243,
113.609707487595,114.609653499946,115.609599512298,116.609545524649,117.609491537,
118.609437549352,119.609383561703,120.609329574054,121.609275586406,122.609221598757,
123.609167611109,124.60911362346,125.609059635811,126.609005648163,127.608951660514,
128.608897672865,129.608843685217,130.608789697568,131.60873570992,132.608681722271,
133.608627734622,134.608573746974,135.608519759325,136.608465771676,137.608411784028,
138.608357796379,139.60830380873,140.608249821082,141.608195833433,142.608141845785,
143.608087858136,144.608033870487,145.607979882839,146.60792589519,147.607871907541,
148.607817919893,149.607763932244,150.607709944596,151.607655956947,152.607601969298,
153.60754798165,154.607493994001,155.607440006352,156.607386018704,157.607332031055,
158.607278043407,159.607224055758,160.607170068109,161.607116080461,162.607062092812,
163.607008105163,164.606954117515,165.606900129866,166.606846142218,167.606792154569,
168.60673816692,169.606684179272,170.606630191623,171.606576203974,172.606522216326,
173.606468228677,174.606414241029,175.60636025338,176.606306265731,177.606252278083,
178.606198290434,179.606144302785,180.606090315137,181.606036327488,182.605982339839,
183.605928352191,184.605874364542,185.605820376894,186.605766389245,187.605712401596,
188.605658413948,189.605604426299),.UNSPECIFIED.);
#90=B_SPLINE_SURFACE_WITH_KNOTS('',3,3,((#34754,#34755,#34756,#34757,#34758,
#34759,#34760,#34761,#34762,#34763,#34764,#34765,#34766,#34767,#34768,#34769,
#34770,#34771,#34772,#34773,#34774,#34775,#34776,#34777,#34778,#34779,#34780,
#34781,#34782,#34783,#34784,#34785,#34786,#34787,#34788,#34789,#34790,#34791,
#34792,#34793,#34794,#34795,#34796,#34797,#34798,#34799,#34800,#34801,#34802,
#34803,#34804,#34805,#34806,#34807,#34808,#34809,#34810,#34811,#34812,#34813,
#34814,#34815,#34816,#34817,#34818,#34819,#34820,#34821,#34822,#34823,#34824,
#34825,#34826,#34827,#34828,#34829,#34830,#34831,#34832,#34833,#34834,#34835,
#34836,#34837,#34838,#34839,#34840,#34841,#34842,#34843,#34844,#34845,#34846,
#34847,#34848,#34849,#34850,#34851,#34852,#34853,#34854,#34855,#34856,#34857,
#34858,#34859,#34860,#34861,#34862,#34863,#34864,#34865,#34866,#34867,#34868,
#34869,#34870,#34871,#34872,#34873,#34874,#34875,#34876,#34877,#34878,#34879,
#34880,#34881,#34882,#34883,#34884,#34885,#34886,#34887,#34888,#34889,#34890,
#34891,#34892,#34893,#34894,#34895,#34896,#34897,#34898,#34899,#34900,#34901,
#34902,#34903,#34904,#34905,#34906,#34907,#34908,#34909,#34910,#34911,#34912,
#34913,#34914,#34915,#34916,#34917,#34918,#34919,#34920,#34921,#34922,#34923,
#34924,#34925,#34926,#34927,#34928,#34929,#34930,#34931,#34932,#34933,#34934),
(#34935,#34936,#34937,#34938,#34939,#34940,#34941,#34942,#34943,#34944,
#34945,#34946,#34947,#34948,#34949,#34950,#34951,#34952,#34953,#34954,#34955,
#34956,#34957,#34958,#34959,#34960,#34961,#34962,#34963,#34964,#34965,#34966,
#34967,#34968,#34969,#34970,#34971,#34972,#34973,#34974,#34975,#34976,#34977,
#34978,#34979,#34980,#34981,#34982,#34983,#34984,#34985,#34986,#34987,#34988,
#34989,#34990,#34991,#34992,#34993,#34994,#34995,#34996,#34997,#34998,#34999,
#35000,#35001,#35002,#35003,#35004,#35005,#35006,#35007,#35008,#35009,#35010,
#35011,#35012,#35013,#35014,#35015,#35016,#35017,#35018,#35019,#35020,#35021,
#35022,#35023,#35024,#35025,#35026,#35027,#35028,#35029,#35030,#35031,#35032,
#35033,#35034,#35035,#35036,#35037,#35038,#35039,#35040,#35041,#35042,#35043,
#35044,#35045,#35046,#35047,#35048,#35049,#35050,#35051,#35052,#35053,#35054,
#35055,#35056,#35057,#35058,#35059,#35060,#35061,#35062,#35063,#35064,#35065,
#35066,#35067,#35068,#35069,#35070,#35071,#35072,#35073,#35074,#35075,#35076,
#35077,#35078,#35079,#35080,#35081,#35082,#35083,#35084,#35085,#35086,#35087,
#35088,#35089,#35090,#35091,#35092,#35093,#35094,#35095,#35096,#35097,#35098,
#35099,#35100,#35101,#35102,#35103,#35104,#35105,#35106,#35107,#35108,#35109,
#35110,#35111,#35112,#35113,#35114,#35115),(#35116,#35117,#35118,#35119,
#35120,#35121,#35122,#35123,#35124,#35125,#35126,#35127,#35128,#35129,#35130,
#35131,#35132,#35133,#35134,#35135,#35136,#35137,#35138,#35139,#35140,#35141,
#35142,#35143,#35144,#35145,#35146,#35147,#35148,#35149,#35150,#35151,#35152,
#35153,#35154,#35155,#35156,#35157,#35158,#35159,#35160,#35161,#35162,#35163,
#35164,#35165,#35166,#35167,#35168,#35169,#35170,#35171,#35172,#35173,#35174,
#35175,#35176,#35177,#35178,#35179,#35180,#35181,#35182,#35183,#35184,#35185,
#35186,#35187,#35188,#35189,#35190,#35191,#35192,#35193,#35194,#35195,#35196,
#35197,#35198,#35199,#35200,#35201,#35202,#35203,#35204,#35205,#35206,#35207,
#35208,#35209,#35210,#35211,#35212,#35213,#35214,#35215,#35216,#35217,#35218,
#35219,#35220,#35221,#35222,#35223,#35224,#35225,#35226,#35227,#35228,#35229,
#35230,#35231,#35232,#35233,#35234,#35235,#35236,#35237,#35238,#35239,#35240,
#35241,#35242,#35243,#35244,#35245,#35246,#35247,#35248,#35249,#35250,#35251,
#35252,#35253,#35254,#35255,#35256,#35257,#35258,#35259,#35260,#35261,#35262,
#35263,#35264,#35265,#35266,#35267,#35268,#35269,#35270,#35271,#35272,#35273,
#35274,#35275,#35276,#35277,#35278,#35279,#35280,#35281,#35282,#35283,#35284,
#35285,#35286,#35287,#35288,#35289,#35290,#35291,#35292,#35293,#35294,#35295,
#35296),(#35297,#35298,#35299,#35300,#35301,#35302,#35303,#35304,#35305,
#35306,#35307,#35308,#35309,#35310,#35311,#35312,#35313,#35314,#35315,#35316,
#35317,#35318,#35319,#35320,#35321,#35322,#35323,#35324,#35325,#35326,#35327,
#35328,#35329,#35330,#35331,#35332,#35333,#35334,#35335,#35336,#35337,#35338,
#35339,#35340,#35341,#35342,#35343,#35344,#35345,#35346,#35347,#35348,#35349,
#35350,#35351,#35352,#35353,#35354,#35355,#35356,#35357,#35358,#35359,#35360,
#35361,#35362,#35363,#35364,#35365,#35366,#35367,#35368,#35369,#35370,#35371,
#35372,#35373,#35374,#35375,#35376,#35377,#35378,#35379,#35380,#35381,#35382,
#35383,#35384,#35385,#35386,#35387,#35388,#35389,#35390,#35391,#35392,#35393,
#35394,#35395,#35396,#35397,#35398,#35399,#35400,#35401,#35402,#35403,#35404,
#35405,#35406,#35407,#35408,#35409,#35410,#35411,#35412,#35413,#35414,#35415,
#35416,#35417,#35418,#35419,#35420,#35421,#35422,#35423,#35424,#35425,#35426,
#35427,#35428,#35429,#35430,#35431,#35432,#35433,#35434,#35435,#35436,#35437,
#35438,#35439,#35440,#35441,#35442,#35443,#35444,#35445,#35446,#35447,#35448,
#35449,#35450,#35451,#35452,#35453,#35454,#35455,#35456,#35457,#35458,#35459,
#35460,#35461,#35462,#35463,#35464,#35465,#35466,#35467,#35468,#35469,#35470,
#35471,#35472,#35473,#35474,#35475,#35476,#35477)),.UNSPECIFIED.,.F.,.F.,
 .F.,(4,4),(4,1,1,1,1,1,1,1,1,1,1,1,1,1,1,1,1,1,1,1,1,1,1,1,1,1,1,1,1,1,
1,1,1,1,1,1,1,1,1,1,1,1,1,1,1,1,1,1,1,1,1,1,1,1,1,1,1,1,1,1,1,1,1,1,1,1,
1,1,1,1,1,1,1,1,1,1,1,1,1,1,1,1,1,1,1,1,1,1,1,1,1,1,1,1,1,1,1,1,1,1,1,1,
1,1,1,1,1,1,1,1,1,1,1,1,1,1,1,1,1,1,1,1,1,1,1,1,1,1,1,1,1,1,1,1,1,1,1,1,
1,1,1,1,1,1,1,1,1,1,1,1,1,1,1,1,1,1,1,1,1,1,1,1,1,1,1,1,1,1,1,1,1,1,1,1,
1,1,1,1,4),(-0.000650925100349628,0.0823958707828885),(8.31473274985812,
9.3146787622095,10.3146247745609,11.3145707869122,12.3145167992636,13.314462811615,
14.3144088239664,15.3143548363177,16.3143008486691,17.3142468610205,18.3141928733718,
19.3141388857232,20.3140848980746,21.314030910426,22.3139769227773,23.3139229351287,
24.3138689474801,25.3138149598315,26.3137609721828,27.3137069845342,28.3136529968856,
29.3135990092369,30.3135450215883,31.3134910339397,32.3134370462911,33.3133830586424,
34.3133290709938,35.3132750833452,36.3132210956965,37.3131671080479,38.3131131203993,
39.3130591327507,40.313005145102,41.3129511574534,42.3128971698048,43.3128431821562,
44.3127891945075,45.3127352068589,46.3126812192103,47.3126272315616,48.312573243913,
49.3125192562644,50.3124652686158,51.3124112809671,52.3123572933185,53.3123033056699,
54.3122493180213,55.3121953303726,56.312141342724,57.3120873550754,58.3120333674267,
59.3119793797781,60.3119253921295,61.3118714044809,62.3118174168322,63.3117634291836,
64.311709441535,65.3116554538863,66.3116014662377,67.3115474785891,68.3114934909405,
69.3114395032918,70.3113855156432,71.3113315279946,72.311277540346,73.3112235526973,
74.3111695650487,75.3111155774001,76.3110615897514,77.3110076021028,78.3109536144542,
79.3108996268056,80.3108456391569,81.3107916515083,82.3107376638597,83.3106836762111,
84.3106296885624,85.3105757009138,86.3105217132652,87.3104677256165,88.3104137379679,
89.3103597503193,90.3103057626707,91.310251775022,92.3101977873734,93.3101437997248,
94.3100898120761,95.3100358244275,96.3099818367789,97.3099278491303,98.3098738614816,
99.309819873833,100.309765886184,101.309711898536,102.309657910887,103.309603923238,
104.30954993559,105.309495947941,106.309441960293,107.309387972644,108.309333984995,
109.309279997347,110.309226009698,111.309172022049,112.309118034401,113.309064046752,
114.309010059104,115.308956071455,116.308902083806,117.308848096158,118.308794108509,
119.30874012086,120.308686133212,121.308632145563,122.308578157915,123.308524170266,
124.308470182617,125.308416194969,126.30836220732,127.308308219671,128.308254232023,
129.308200244374,130.308146256726,131.308092269077,132.308038281428,133.30798429378,
134.307930306131,135.307876318482,136.307822330834,137.307768343185,138.307714355537,
139.307660367888,140.307606380239,141.307552392591,142.307498404942,143.307444417293,
144.307390429645,145.307336441996,146.307282454348,147.307228466699,148.30717447905,
149.307120491402,150.307066503753,151.307012516104,152.306958528456,153.306904540807,
154.306850553158,155.30679656551,156.306742577861,157.306688590213,158.306634602564,
159.306580614915,160.306526627267,161.306472639618,162.306418651969,163.306364664321,
164.306310676672,165.306256689024,166.306202701375,167.306148713726,168.306094726078,
169.306040738429,170.30598675078,171.305932763132,172.305878775483,173.305824787835,
174.305770800186,175.305716812537,176.305662824889,177.30560883724,178.305554849591,
179.305500861943,180.305446874294,181.305392886646,182.305338898997,183.305284911348,
184.3052309237,185.305176936051,186.305773873502),.UNSPECIFIED.);
#91=B_SPLINE_SURFACE_WITH_KNOTS('',3,3,((#35967,#35968,#35969,#35970,#35971,
#35972,#35973,#35974,#35975,#35976,#35977,#35978,#35979,#35980,#35981,#35982,
#35983,#35984,#35985,#35986,#35987,#35988,#35989,#35990,#35991,#35992,#35993,
#35994,#35995,#35996,#35997,#35998,#35999,#36000,#36001,#36002,#36003,#36004,
#36005,#36006,#36007,#36008,#36009,#36010,#36011,#36012,#36013,#36014,#36015,
#36016,#36017,#36018,#36019,#36020,#36021,#36022,#36023,#36024,#36025,#36026,
#36027,#36028,#36029,#36030,#36031,#36032,#36033,#36034,#36035,#36036,#36037,
#36038,#36039,#36040,#36041,#36042,#36043,#36044,#36045,#36046,#36047,#36048,
#36049,#36050,#36051,#36052,#36053,#36054,#36055,#36056,#36057,#36058,#36059,
#36060,#36061,#36062,#36063,#36064,#36065,#36066,#36067,#36068,#36069,#36070,
#36071,#36072,#36073,#36074,#36075,#36076,#36077,#36078,#36079,#36080,#36081,
#36082,#36083,#36084,#36085,#36086,#36087,#36088,#36089,#36090,#36091,#36092,
#36093,#36094,#36095,#36096,#36097,#36098,#36099,#36100,#36101,#36102,#36103,
#36104,#36105,#36106,#36107,#36108,#36109,#36110,#36111,#36112,#36113,#36114,
#36115,#36116,#36117,#36118,#36119,#36120,#36121,#36122,#36123,#36124,#36125,
#36126,#36127,#36128,#36129,#36130,#36131,#36132,#36133,#36134,#36135,#36136,
#36137,#36138,#36139,#36140,#36141,#36142,#36143,#36144,#36145,#36146,#36147),
(#36148,#36149,#36150,#36151,#36152,#36153,#36154,#36155,#36156,#36157,
#36158,#36159,#36160,#36161,#36162,#36163,#36164,#36165,#36166,#36167,#36168,
#36169,#36170,#36171,#36172,#36173,#36174,#36175,#36176,#36177,#36178,#36179,
#36180,#36181,#36182,#36183,#36184,#36185,#36186,#36187,#36188,#36189,#36190,
#36191,#36192,#36193,#36194,#36195,#36196,#36197,#36198,#36199,#36200,#36201,
#36202,#36203,#36204,#36205,#36206,#36207,#36208,#36209,#36210,#36211,#36212,
#36213,#36214,#36215,#36216,#36217,#36218,#36219,#36220,#36221,#36222,#36223,
#36224,#36225,#36226,#36227,#36228,#36229,#36230,#36231,#36232,#36233,#36234,
#36235,#36236,#36237,#36238,#36239,#36240,#36241,#36242,#36243,#36244,#36245,
#36246,#36247,#36248,#36249,#36250,#36251,#36252,#36253,#36254,#36255,#36256,
#36257,#36258,#36259,#36260,#36261,#36262,#36263,#36264,#36265,#36266,#36267,
#36268,#36269,#36270,#36271,#36272,#36273,#36274,#36275,#36276,#36277,#36278,
#36279,#36280,#36281,#36282,#36283,#36284,#36285,#36286,#36287,#36288,#36289,
#36290,#36291,#36292,#36293,#36294,#36295,#36296,#36297,#36298,#36299,#36300,
#36301,#36302,#36303,#36304,#36305,#36306,#36307,#36308,#36309,#36310,#36311,
#36312,#36313,#36314,#36315,#36316,#36317,#36318,#36319,#36320,#36321,#36322,
#36323,#36324,#36325,#36326,#36327,#36328),(#36329,#36330,#36331,#36332,
#36333,#36334,#36335,#36336,#36337,#36338,#36339,#36340,#36341,#36342,#36343,
#36344,#36345,#36346,#36347,#36348,#36349,#36350,#36351,#36352,#36353,#36354,
#36355,#36356,#36357,#36358,#36359,#36360,#36361,#36362,#36363,#36364,#36365,
#36366,#36367,#36368,#36369,#36370,#36371,#36372,#36373,#36374,#36375,#36376,
#36377,#36378,#36379,#36380,#36381,#36382,#36383,#36384,#36385,#36386,#36387,
#36388,#36389,#36390,#36391,#36392,#36393,#36394,#36395,#36396,#36397,#36398,
#36399,#36400,#36401,#36402,#36403,#36404,#36405,#36406,#36407,#36408,#36409,
#36410,#36411,#36412,#36413,#36414,#36415,#36416,#36417,#36418,#36419,#36420,
#36421,#36422,#36423,#36424,#36425,#36426,#36427,#36428,#36429,#36430,#36431,
#36432,#36433,#36434,#36435,#36436,#36437,#36438,#36439,#36440,#36441,#36442,
#36443,#36444,#36445,#36446,#36447,#36448,#36449,#36450,#36451,#36452,#36453,
#36454,#36455,#36456,#36457,#36458,#36459,#36460,#36461,#36462,#36463,#36464,
#36465,#36466,#36467,#36468,#36469,#36470,#36471,#36472,#36473,#36474,#36475,
#36476,#36477,#36478,#36479,#36480,#36481,#36482,#36483,#36484,#36485,#36486,
#36487,#36488,#36489,#36490,#36491,#36492,#36493,#36494,#36495,#36496,#36497,
#36498,#36499,#36500,#36501,#36502,#36503,#36504,#36505,#36506,#36507,#36508,
#36509),(#36510,#36511,#36512,#36513,#36514,#36515,#36516,#36517,#36518,
#36519,#36520,#36521,#36522,#36523,#36524,#36525,#36526,#36527,#36528,#36529,
#36530,#36531,#36532,#36533,#36534,#36535,#36536,#36537,#36538,#36539,#36540,
#36541,#36542,#36543,#36544,#36545,#36546,#36547,#36548,#36549,#36550,#36551,
#36552,#36553,#36554,#36555,#36556,#36557,#36558,#36559,#36560,#36561,#36562,
#36563,#36564,#36565,#36566,#36567,#36568,#36569,#36570,#36571,#36572,#36573,
#36574,#36575,#36576,#36577,#36578,#36579,#36580,#36581,#36582,#36583,#36584,
#36585,#36586,#36587,#36588,#36589,#36590,#36591,#36592,#36593,#36594,#36595,
#36596,#36597,#36598,#36599,#36600,#36601,#36602,#36603,#36604,#36605,#36606,
#36607,#36608,#36609,#36610,#36611,#36612,#36613,#36614,#36615,#36616,#36617,
#36618,#36619,#36620,#36621,#36622,#36623,#36624,#36625,#36626,#36627,#36628,
#36629,#36630,#36631,#36632,#36633,#36634,#36635,#36636,#36637,#36638,#36639,
#36640,#36641,#36642,#36643,#36644,#36645,#36646,#36647,#36648,#36649,#36650,
#36651,#36652,#36653,#36654,#36655,#36656,#36657,#36658,#36659,#36660,#36661,
#36662,#36663,#36664,#36665,#36666,#36667,#36668,#36669,#36670,#36671,#36672,
#36673,#36674,#36675,#36676,#36677,#36678,#36679,#36680,#36681,#36682,#36683,
#36684,#36685,#36686,#36687,#36688,#36689,#36690)),.UNSPECIFIED.,.F.,.F.,
 .F.,(4,4),(4,1,1,1,1,1,1,1,1,1,1,1,1,1,1,1,1,1,1,1,1,1,1,1,1,1,1,1,1,1,
1,1,1,1,1,1,1,1,1,1,1,1,1,1,1,1,1,1,1,1,1,1,1,1,1,1,1,1,1,1,1,1,1,1,1,1,
1,1,1,1,1,1,1,1,1,1,1,1,1,1,1,1,1,1,1,1,1,1,1,1,1,1,1,1,1,1,1,1,1,1,1,1,
1,1,1,1,1,1,1,1,1,1,1,1,1,1,1,1,1,1,1,1,1,1,1,1,1,1,1,1,1,1,1,1,1,1,1,1,
1,1,1,1,1,1,1,1,1,1,1,1,1,1,1,1,1,1,1,1,1,1,1,1,1,1,1,1,1,1,1,1,1,1,1,1,
1,1,1,1,4),(-0.00033399260015787,0.082683618112034),(11.6145432153813,12.6151602401062,
13.6151062524576,14.615052264809,15.6149982771603,16.6149442895117,17.6148903018631,
18.6148363142145,19.6147823265658,20.6147283389172,21.6146743512686,22.61462036362,
23.6145663759713,24.6145123883227,25.6144584006741,26.6144044130254,27.6143504253768,
28.6142964377282,29.6142424500796,30.6141884624309,31.6141344747823,32.6140804871337,
33.614026499485,34.6139725118364,35.6139185241878,36.6138645365392,37.6138105488905,
38.6137565612419,39.6137025735933,40.6136485859447,41.613594598296,42.6135406106474,
43.6134866229988,44.6134326353501,45.6133786477015,46.6133246600529,47.6132706724043,
48.6132166847556,49.613162697107,50.6131087094584,51.6130547218097,52.6130007341611,
53.6129467465125,54.6128927588639,55.6128387712152,56.6127847835666,57.612730795918,
58.6126768082694,59.6126228206207,60.6125688329721,61.6125148453235,62.6124608576748,
63.6124068700262,64.6123528823776,65.612298894729,66.6122449070803,67.6121909194317,
68.6121369317831,69.6120829441344,70.6120289564858,71.6119749688372,72.6119209811886,
73.6118669935399,74.6118130058913,75.6117590182427,76.6117050305941,77.6116510429454,
78.6115970552968,79.6115430676482,80.6114890799995,81.6114350923509,82.6113811047023,
83.6113271170537,84.611273129405,85.6112191417564,86.6111651541078,87.6111111664591,
88.6110571788105,89.6110031911619,90.6109492035133,91.6108952158646,92.610841228216,
93.6107872405674,94.6107332529187,95.6106792652701,96.6106252776215,97.6105712899729,
98.6105173023242,99.6104633146756,100.610409327027,101.610355339378,102.61030135173,
103.610247364081,104.610193376432,105.610139388784,106.610085401135,107.610031413487,
108.609977425838,109.609923438189,110.609869450541,111.609815462892,112.609761475243,
113.609707487595,114.609653499946,115.609599512298,116.609545524649,117.609491537,
118.609437549352,119.609383561703,120.609329574054,121.609275586406,122.609221598757,
123.609167611109,124.60911362346,125.609059635811,126.609005648163,127.608951660514,
128.608897672865,129.608843685217,130.608789697568,131.60873570992,132.608681722271,
133.608627734622,134.608573746974,135.608519759325,136.608465771676,137.608411784028,
138.608357796379,139.60830380873,140.608249821082,141.608195833433,142.608141845785,
143.608087858136,144.608033870487,145.607979882839,146.60792589519,147.607871907541,
148.607817919893,149.607763932244,150.607709944596,151.607655956947,152.607601969298,
153.60754798165,154.607493994001,155.607440006352,156.607386018704,157.607332031055,
158.607278043407,159.607224055758,160.607170068109,161.607116080461,162.607062092812,
163.607008105163,164.606954117515,165.606900129866,166.606846142218,167.606792154569,
168.60673816692,169.606684179272,170.606630191623,171.606576203974,172.606522216326,
173.606468228677,174.606414241029,175.60636025338,176.606306265731,177.606252278083,
178.606198290434,179.606144302785,180.606090315137,181.606036327488,182.605982339839,
183.605928352191,184.605874364542,185.605820376894,186.605766389245,187.605712401596,
188.605658413948,189.605604426299),.UNSPECIFIED.);
#92=B_SPLINE_SURFACE_WITH_KNOTS('',3,3,((#41391,#41392,#41393,#41394,#41395,
#41396,#41397,#41398,#41399,#41400,#41401,#41402,#41403,#41404,#41405,#41406,
#41407,#41408,#41409,#41410,#41411,#41412,#41413,#41414,#41415,#41416,#41417,
#41418,#41419,#41420,#41421,#41422,#41423,#41424,#41425,#41426,#41427,#41428,
#41429,#41430,#41431,#41432,#41433,#41434,#41435,#41436,#41437,#41438,#41439,
#41440,#41441,#41442,#41443,#41444,#41445,#41446,#41447,#41448,#41449,#41450,
#41451,#41452,#41453,#41454,#41455,#41456,#41457,#41458,#41459,#41460,#41461,
#41462,#41463,#41464,#41465,#41466,#41467,#41468,#41469,#41470,#41471,#41472,
#41473,#41474,#41475,#41476,#41477,#41478,#41479,#41480,#41481),(#41482,
#41483,#41484,#41485,#41486,#41487,#41488,#41489,#41490,#41491,#41492,#41493,
#41494,#41495,#41496,#41497,#41498,#41499,#41500,#41501,#41502,#41503,#41504,
#41505,#41506,#41507,#41508,#41509,#41510,#41511,#41512,#41513,#41514,#41515,
#41516,#41517,#41518,#41519,#41520,#41521,#41522,#41523,#41524,#41525,#41526,
#41527,#41528,#41529,#41530,#41531,#41532,#41533,#41534,#41535,#41536,#41537,
#41538,#41539,#41540,#41541,#41542,#41543,#41544,#41545,#41546,#41547,#41548,
#41549,#41550,#41551,#41552,#41553,#41554,#41555,#41556,#41557,#41558,#41559,
#41560,#41561,#41562,#41563,#41564,#41565,#41566,#41567,#41568,#41569,#41570,
#41571,#41572),(#41573,#41574,#41575,#41576,#41577,#41578,#41579,#41580,
#41581,#41582,#41583,#41584,#41585,#41586,#41587,#41588,#41589,#41590,#41591,
#41592,#41593,#41594,#41595,#41596,#41597,#41598,#41599,#41600,#41601,#41602,
#41603,#41604,#41605,#41606,#41607,#41608,#41609,#41610,#41611,#41612,#41613,
#41614,#41615,#41616,#41617,#41618,#41619,#41620,#41621,#41622,#41623,#41624,
#41625,#41626,#41627,#41628,#41629,#41630,#41631,#41632,#41633,#41634,#41635,
#41636,#41637,#41638,#41639,#41640,#41641,#41642,#41643,#41644,#41645,#41646,
#41647,#41648,#41649,#41650,#41651,#41652,#41653,#41654,#41655,#41656,#41657,
#41658,#41659,#41660,#41661,#41662,#41663),(#41664,#41665,#41666,#41667,
#41668,#41669,#41670,#41671,#41672,#41673,#41674,#41675,#41676,#41677,#41678,
#41679,#41680,#41681,#41682,#41683,#41684,#41685,#41686,#41687,#41688,#41689,
#41690,#41691,#41692,#41693,#41694,#41695,#41696,#41697,#41698,#41699,#41700,
#41701,#41702,#41703,#41704,#41705,#41706,#41707,#41708,#41709,#41710,#41711,
#41712,#41713,#41714,#41715,#41716,#41717,#41718,#41719,#41720,#41721,#41722,
#41723,#41724,#41725,#41726,#41727,#41728,#41729,#41730,#41731,#41732,#41733,
#41734,#41735,#41736,#41737,#41738,#41739,#41740,#41741,#41742,#41743,#41744,
#41745,#41746,#41747,#41748,#41749,#41750,#41751,#41752,#41753,#41754)),
 .UNSPECIFIED.,.F.,.F.,.F.,(4,4),(4,1,1,1,1,1,1,1,1,1,1,1,1,1,1,1,1,1,1,
1,1,1,1,1,1,1,1,1,1,1,1,1,1,1,1,1,1,1,1,1,1,1,1,1,1,1,1,1,1,1,1,1,1,1,1,
1,1,1,1,1,1,1,1,1,1,1,1,1,1,1,1,1,1,1,1,1,1,1,1,1,1,1,1,1,1,1,1,1,4),(-0.000129081019394558,
0.193330292353948),(11.8519068837255,12.3510302549558,12.8500245451668,
13.3490188353777,13.8480131255886,14.3470074157995,14.8460017060104,15.3449959962214,
15.8439902864323,16.3429845766432,16.8419788668541,17.3409731570651,17.839967447276,
18.3389617374869,18.8379560276978,19.3369503179088,19.8359446081197,20.3349388983306,
20.8339331885415,21.3329274787524,21.8319217689634,22.3309160591743,22.8299103493852,
23.3289046395961,23.8278989298071,24.326893220018,24.8258875102289,25.3248818004398,
25.8238760906508,26.3228703808617,26.8218646710726,27.3208589612835,27.8198532514944,
28.3188475417054,28.8178418319163,29.3168361221272,29.8158304123381,30.3148247025491,
30.81381899276,31.3128132829709,31.8118075731818,32.3108018633928,32.8097961536037,
33.3087904438146,33.8077847340255,34.3067790242364,34.8057733144474,35.3047676046583,
35.8037618948692,36.3027561850801,36.8017504752911,37.300744765502,37.7997390557129,
38.2987333459238,38.7977276361348,39.2967219263457,39.7957162165566,40.2947105067675,
40.7937047969784,41.2926990871894,41.7916933774003,42.2906876676112,42.7896819578221,
43.2886762480331,43.787670538244,44.2866648284549,44.7856591186658,45.2846534088767,
45.7836476990877,46.2826419892986,46.7816362795095,47.2806305697204,47.7796248599314,
48.2786191501423,48.7776134403532,49.2766077305641,49.7756020207751,50.274596310986,
50.7735906011969,51.2725848914078,51.7715791816187,52.2705734718297,52.7695677620406,
53.2685620522515,53.7675563424624,54.2665506326734,54.7655449228843,55.2645392130952,
55.7635335033061),.UNSPECIFIED.);
#93=B_SPLINE_SURFACE_WITH_KNOTS('',3,3,((#41996,#41997,#41998,#41999,#42000,
#42001,#42002,#42003,#42004,#42005,#42006,#42007,#42008,#42009,#42010,#42011,
#42012,#42013,#42014,#42015,#42016,#42017,#42018,#42019,#42020,#42021,#42022,
#42023,#42024,#42025,#42026,#42027,#42028,#42029,#42030,#42031,#42032,#42033,
#42034,#42035,#42036,#42037,#42038,#42039,#42040,#42041,#42042,#42043,#42044,
#42045,#42046,#42047,#42048,#42049,#42050,#42051,#42052,#42053,#42054,#42055,
#42056,#42057,#42058,#42059,#42060,#42061,#42062,#42063,#42064,#42065,#42066,
#42067,#42068,#42069,#42070,#42071,#42072,#42073,#42074,#42075,#42076,#42077,
#42078,#42079,#42080,#42081,#42082,#42083,#42084,#42085,#42086),(#42087,
#42088,#42089,#42090,#42091,#42092,#42093,#42094,#42095,#42096,#42097,#42098,
#42099,#42100,#42101,#42102,#42103,#42104,#42105,#42106,#42107,#42108,#42109,
#42110,#42111,#42112,#42113,#42114,#42115,#42116,#42117,#42118,#42119,#42120,
#42121,#42122,#42123,#42124,#42125,#42126,#42127,#42128,#42129,#42130,#42131,
#42132,#42133,#42134,#42135,#42136,#42137,#42138,#42139,#42140,#42141,#42142,
#42143,#42144,#42145,#42146,#42147,#42148,#42149,#42150,#42151,#42152,#42153,
#42154,#42155,#42156,#42157,#42158,#42159,#42160,#42161,#42162,#42163,#42164,
#42165,#42166,#42167,#42168,#42169,#42170,#42171,#42172,#42173,#42174,#42175,
#42176,#42177),(#42178,#42179,#42180,#42181,#42182,#42183,#42184,#42185,
#42186,#42187,#42188,#42189,#42190,#42191,#42192,#42193,#42194,#42195,#42196,
#42197,#42198,#42199,#42200,#42201,#42202,#42203,#42204,#42205,#42206,#42207,
#42208,#42209,#42210,#42211,#42212,#42213,#42214,#42215,#42216,#42217,#42218,
#42219,#42220,#42221,#42222,#42223,#42224,#42225,#42226,#42227,#42228,#42229,
#42230,#42231,#42232,#42233,#42234,#42235,#42236,#42237,#42238,#42239,#42240,
#42241,#42242,#42243,#42244,#42245,#42246,#42247,#42248,#42249,#42250,#42251,
#42252,#42253,#42254,#42255,#42256,#42257,#42258,#42259,#42260,#42261,#42262,
#42263,#42264,#42265,#42266,#42267,#42268),(#42269,#42270,#42271,#42272,
#42273,#42274,#42275,#42276,#42277,#42278,#42279,#42280,#42281,#42282,#42283,
#42284,#42285,#42286,#42287,#42288,#42289,#42290,#42291,#42292,#42293,#42294,
#42295,#42296,#42297,#42298,#42299,#42300,#42301,#42302,#42303,#42304,#42305,
#42306,#42307,#42308,#42309,#42310,#42311,#42312,#42313,#42314,#42315,#42316,
#42317,#42318,#42319,#42320,#42321,#42322,#42323,#42324,#42325,#42326,#42327,
#42328,#42329,#42330,#42331,#42332,#42333,#42334,#42335,#42336,#42337,#42338,
#42339,#42340,#42341,#42342,#42343,#42344,#42345,#42346,#42347,#42348,#42349,
#42350,#42351,#42352,#42353,#42354,#42355,#42356,#42357,#42358,#42359)),
 .UNSPECIFIED.,.F.,.F.,.F.,(4,4),(4,1,1,1,1,1,1,1,1,1,1,1,1,1,1,1,1,1,1,
1,1,1,1,1,1,1,1,1,1,1,1,1,1,1,1,1,1,1,1,1,1,1,1,1,1,1,1,1,1,1,1,1,1,1,1,
1,1,1,1,1,1,1,1,1,1,1,1,1,1,1,1,1,1,1,1,1,1,1,1,1,1,1,1,1,1,1,1,1,4),(-9.09719654654217E-5,
0.1933682374602),(14.3987024268659,14.8976967170768,15.3966910072877,15.8956852974986,
16.3946795877096,16.8936738779205,17.3926681681314,17.8916624583423,18.3906567485533,
18.8896510387642,19.3886453289751,19.887639619186,20.386633909397,20.8856281996079,
21.3846224898188,21.8836167800297,22.3826110702406,22.8816053604516,23.3805996506625,
23.8795939408734,24.3785882310843,24.8775825212953,25.3765768115062,25.8755711017171,
26.374565391928,26.8735596821389,27.3725539723499,27.8715482625608,28.3705425527717,
28.8695368429826,29.3685311331936,29.8675254234045,30.3665197136154,30.8655140038263,
31.3645082940373,31.8635025842482,32.3624968744591,32.86149116467,33.3604854548809,
33.8594797450919,34.3584740353028,34.8574683255137,35.3564626157246,35.8554569059356,
36.3544511961465,36.8534454863574,37.3524397765683,37.8514340667792,38.3504283569902,
38.8494226472011,39.348416937412,39.8474112276229,40.3464055178339,40.8453998080448,
41.3443940982557,41.8433883884666,42.3423826786776,42.8413769688885,43.3403712590994,
43.8393655493103,44.3383598395212,44.8373541297322,45.3363484199431,45.835342710154,
46.3343370003649,46.8333312905759,47.3323255807868,47.8313198709977,48.3303141612086,
48.8293084514195,49.3283027416305,49.8272970318414,50.3262913220523,50.8252856122632,
51.3242799024742,51.8232741926851,52.322268482896,52.8212627731069,53.3202570633179,
53.8192513535288,54.3182456437397,54.8172399339506,55.3162342241615,55.8152285143725,
56.3142228045834,56.8132170947943,57.3122113850052,57.8112056752162,58.3103290677895),
 .UNSPECIFIED.);
#94=B_SPLINE_CURVE_WITH_KNOTS('',3,(#5427,#5428,#5429,#5430,#5431,#5432,
#5433,#5434,#5435,#5436,#5437,#5438,#5439,#5440,#5441,#5442,#5443,#5444,
#5445,#5446,#5447,#5448,#5449,#5450,#5451,#5452,#5453,#5454,#5455,#5456,
#5457,#5458,#5459,#5460,#5461,#5462,#5463,#5464,#5465,#5466,#5467,#5468,
#5469,#5470,#5471,#5472,#5473,#5474,#5475,#5476,#5477,#5478,#5479,#5480,
#5481,#5482,#5483,#5484,#5485,#5486,#5487,#5488,#5489,#5490,#5491,#5492,
#5493,#5494,#5495,#5496,#5497,#5498,#5499,#5500,#5501,#5502,#5503,#5504,
#5505,#5506,#5507,#5508,#5509,#5510,#5511,#5512,#5513,#5514,#5515,#5516,
#5517,#5518,#5519,#5520,#5521,#5522,#5523,#5524,#5525,#5526,#5527,#5528,
#5529,#5530,#5531,#5532,#5533,#5534,#5535,#5536,#5537,#5538,#5539,#5540,
#5541,#5542,#5543,#5544,#5545,#5546,#5547,#5548,#5549,#5550),
 .UNSPECIFIED.,.F.,.F.,(4,3,3,3,3,3,3,3,3,3,3,3,3,3,3,3,3,3,3,3,3,3,3,3,
3,3,3,3,3,3,3,3,3,3,3,3,3,3,3,3,3,4),(0.,0.0515890274929282,0.103204292695659,
0.154856373216778,0.206591856648151,0.25837614825577,0.310254566416546,
0.326770108848208,0.398899776939704,0.480730369472977,0.567135293584696,
0.646990791668246,0.653540217696416,0.713270639311335,0.772778129234328,
0.831949962874738,0.890922354735589,0.949595703830974,0.980310326544624,
1.02811421917601,1.07588590458137,1.1236371825647,1.17139353825776,1.21915060551796,
1.26694469505578,1.30708043539283,1.36339088247901,1.4198291936612,1.47649599617247,
1.52492717462497,1.60478198943241,1.69630632876662,1.79926962978145,1.88030337649094,
1.96062065308925,2.01516322116673,2.0696000908893,2.12403374160535,2.17846739232139,
2.22502234109762,2.27155796869371,2.28737840760206),.UNSPECIFIED.);
#95=B_SPLINE_CURVE_WITH_KNOTS('',3,(#5551,#5552,#5553,#5554,#5555,#5556,
#5557,#5558,#5559,#5560,#5561,#5562,#5563,#5564,#5565,#5566,#5567,#5568,
#5569,#5570,#5571,#5572,#5573,#5574,#5575,#5576,#5577,#5578,#5579,#5580,
#5581,#5582,#5583,#5584,#5585,#5586,#5587,#5588,#5589,#5590,#5591,#5592,
#5593,#5594,#5595,#5596,#5597,#5598,#5599,#5600,#5601,#5602,#5603,#5604,
#5605,#5606,#5607,#5608,#5609,#5610,#5611,#5612,#5613,#5614,#5615,#5616,
#5617,#5618,#5619,#5620,#5621,#5622,#5623,#5624,#5625,#5626,#5627,#5628,
#5629,#5630,#5631,#5632,#5633,#5634,#5635,#5636,#5637,#5638,#5639,#5640,
#5641,#5642,#5643,#5644,#5645,#5646,#5647,#5648,#5649,#5650,#5651,#5652,
#5653,#5654,#5655,#5656,#5657,#5658,#5659,#5660,#5661,#5662,#5663,#5664,
#5665,#5666,#5667,#5668,#5669,#5670,#5671,#5672,#5673,#5674,#5675,#5676,
#5677),.UNSPECIFIED.,.F.,.F.,(4,3,3,3,3,3,3,3,3,3,3,3,3,3,3,3,3,3,3,3,3,
3,3,3,3,3,3,3,3,3,3,3,3,3,3,3,3,3,3,3,3,3,4),(2.28737840766402,2.33375007519743,
2.3801437049756,2.39631413155352,2.45117314344955,2.50612653591306,2.56126498980737,
2.61416087078566,2.69133411582037,2.77539876579215,2.86930017643718,2.95957726284356,
3.0384899988861,3.04985434924994,3.11071114418125,3.17119439820841,3.23109353713712,
3.26770108848208,3.31260298810012,3.35748093451019,3.40234653816875,3.44723256342706,
3.48554782771422,3.54204675587125,3.59866131344456,3.65539681169898,3.712258631246,
3.76933145073308,3.82652040574213,3.8839071682845,3.92124130617849,4.00407786973751,
4.08802290404028,4.16801715953349,4.23929616483205,4.2480114150267,4.30052474757075,
4.35295604051741,4.40531606758536,4.45759990073163,4.50983970731316,4.56203893311869,
4.57478152387491),.UNSPECIFIED.);
#96=B_SPLINE_CURVE_WITH_KNOTS('',3,(#5769,#5770,#5771,#5772,#5773),
 .UNSPECIFIED.,.F.,.F.,(4,1,4),(0.,0.571428571428571,1.00000000000031),
 .UNSPECIFIED.);
#97=B_SPLINE_CURVE_WITH_KNOTS('',3,(#5774,#5775,#5776,#5777,#5778,#5779,
#5780,#5781,#5782,#5783,#5784,#5785,#5786,#5787,#5788,#5789,#5790,#5791),
 .UNSPECIFIED.,.T.,.F.,(4,1,1,1,1,1,1,1,1,1,1,1,1,1,1,4),(-4.57478152387491,
-4.2480114150267,-3.92124130617849,-3.48554782771422,-3.26770108848208,
-3.04985434924994,-2.61416087078566,-2.39631413155352,-2.17846739232139,
-1.96062065308925,-1.52492717462497,-1.30708043539283,-0.980310326544624,
-0.653540217696416,-0.326770108848208,0.),.UNSPECIFIED.);
#98=B_SPLINE_CURVE_WITH_KNOTS('',3,(#5801,#5802,#5803,#5804,#5805,#5806,
#5807,#5808,#5809,#5810,#5811,#5812,#5813,#5814,#5815,#5816,#5817,#5818),
 .UNSPECIFIED.,.F.,.F.,(4,2,2,2,2,2,2,2,4),(-3.69014930019619,-3.45920017966731,
-3.22825105913842,-2.99793151714278,-2.76761197514714,-2.5372924331515,
-2.30697289115586,-2.07602377062698,-1.8450746500981),.UNSPECIFIED.);
#99=B_SPLINE_CURVE_WITH_KNOTS('',3,(#5819,#5820,#5821,#5822,#5823,#5824,
#5825,#5826,#5827,#5828,#5829,#5830,#5831,#5832,#5833,#5834,#5835,#5836),
 .UNSPECIFIED.,.F.,.F.,(4,2,2,2,2,2,2,2,4),(-1.8450746500981,-1.61412552956921,
-1.38317640904033,-1.15285686704469,-0.922537325049048,-0.692217783053408,
-0.461898241057768,-0.230949120528884,0.),.UNSPECIFIED.);
#100=B_SPLINE_CURVE_WITH_KNOTS('',3,(#5957,#5958,#5959,#5960,#5961,#5962,
#5963),.UNSPECIFIED.,.F.,.F.,(4,3,4),(13.8756314554422,13.9455249758043,
14.0061469241355),.UNSPECIFIED.);
#101=B_SPLINE_CURVE_WITH_KNOTS('',3,(#5970,#5971,#5972,#5973,#5974,#5975,
#5976,#5977,#5978,#5979,#5980,#5981,#5982,#5983,#5984,#5985,#5986,#5987,
#5988,#5989,#5990,#5991,#5992,#5993,#5994,#5995,#5996,#5997,#5998,#5999,
#6000,#6001,#6002,#6003,#6004,#6005,#6006,#6007,#6008,#6009,#6010,#6011,
#6012,#6013,#6014,#6015,#6016,#6017,#6018,#6019,#6020,#6021,#6022,#6023,
#6024,#6025,#6026,#6027,#6028,#6029,#6030,#6031,#6032,#6033,#6034,#6035,
#6036,#6037,#6038,#6039,#6040,#6041,#6042,#6043,#6044,#6045,#6046,#6047,
#6048,#6049,#6050,#6051,#6052,#6053,#6054,#6055,#6056,#6057,#6058,#6059,
#6060,#6061,#6062,#6063,#6064,#6065,#6066,#6067,#6068,#6069,#6070,#6071,
#6072,#6073,#6074,#6075,#6076,#6077,#6078,#6079,#6080,#6081,#6082,#6083,
#6084,#6085,#6086,#6087,#6088,#6089,#6090,#6091,#6092,#6093,#6094,#6095,
#6096,#6097,#6098,#6099,#6100,#6101,#6102,#6103,#6104,#6105,#6106,#6107,
#6108,#6109,#6110,#6111,#6112,#6113,#6114,#6115,#6116,#6117,#6118,#6119,
#6120,#6121,#6122,#6123,#6124,#6125,#6126,#6127,#6128,#6129,#6130,#6131,
#6132,#6133,#6134,#6135,#6136,#6137,#6138,#6139,#6140,#6141,#6142,#6143,
#6144,#6145,#6146,#6147,#6148,#6149,#6150,#6151,#6152,#6153,#6154,#6155,
#6156,#6157,#6158,#6159,#6160,#6161,#6162,#6163,#6164,#6165),
 .UNSPECIFIED.,.F.,.F.,(4,3,3,3,3,3,3,3,3,3,3,3,3,3,3,3,3,3,3,3,3,3,3,3,
3,3,3,3,3,3,3,3,3,3,3,3,3,3,3,3,3,3,3,3,3,3,3,3,3,3,3,3,3,3,3,3,3,3,3,3,
3,3,3,3,3,4),(15.7079632680278,15.781258546969,15.8439902864323,15.9140293859905,
15.9840565719878,16.0540759705774,16.1263031220939,16.1963262492752,16.2696554129592,
16.3429845766432,16.4130258394328,16.4830552130784,16.5530768178735,16.6253023301186,
16.6953276818739,16.768653274364,16.8419788668541,16.9120192399517,16.9820477145933,
17.0520684134795,17.1242945993759,17.1943190394544,17.2676460982597,17.3409731570651,
17.4110137716016,17.4810424897669,17.5510634336108,17.6232894370271,17.6933141225493,
17.7666407849127,17.839967447276,17.9100080714022,17.9800367996442,18.0500577540238,
18.1222837498896,18.192308446954,18.2656350922205,18.3389617374869,18.4090022932936,
18.4790309522726,18.5490518366316,18.6212778843981,18.6913025104407,18.7646292690693,
18.8379560276978,18.9079966408986,18.9780253579764,19.048046300983,19.1202723052145,
19.1902969905308,19.2636236542198,19.3369503179088,19.406990897852,19.47701958129,
19.5470404903645,19.6192665198033,19.6892911708882,19.762617889504,19.8359446081197,
19.9059847976786,19.9760129588395,20.0460332138481,20.1160559860082,20.1860772609487,
20.2561091917616,20.289300242169),.UNSPECIFIED.);
#102=B_SPLINE_CURVE_WITH_KNOTS('',3,(#6166,#6167,#6168,#6169,#6170,#6171,
#6172,#6173,#6174,#6175,#6176,#6177,#6178,#6179,#6180,#6181,#6182,#6183,
#6184,#6185,#6186,#6187,#6188,#6189,#6190,#6191,#6192,#6193,#6194,#6195,
#6196,#6197,#6198,#6199,#6200,#6201,#6202,#6203,#6204,#6205,#6206,#6207,
#6208,#6209,#6210,#6211,#6212,#6213,#6214,#6215,#6216,#6217,#6218,#6219,
#6220,#6221,#6222,#6223,#6224,#6225,#6226,#6227,#6228,#6229,#6230,#6231,
#6232,#6233,#6234,#6235,#6236,#6237,#6238,#6239,#6240,#6241),
 .UNSPECIFIED.,.F.,.F.,(4,3,3,3,3,3,3,3,3,3,3,3,3,3,3,3,3,3,3,3,3,3,3,3,
3,4),(14.0061469241355,14.076021357976,14.1459007978716,14.2157791918409,
14.2856739697488,14.3470074157995,14.4170482343003,14.4870771759581,14.5570983621866,
14.6293241981425,14.6993491698427,14.7726754379265,14.8460017060104,14.9160393182244,
14.9860649926552,15.0560828595175,15.1283111436935,15.198332708346,15.2716643522837,
15.3449959962214,15.4148686130277,15.488142276758,15.5579967616873,15.6278466788921,
15.697700868083,15.7079632679489),.UNSPECIFIED.);
#103=B_SPLINE_CURVE_WITH_KNOTS('',3,(#6245,#6246,#6247,#6248,#6249,#6250),
 .UNSPECIFIED.,.F.,.F.,(4,1,1,4),(14.3987024268659,14.8976967170768,15.3966910072877,
15.7079632679489),.UNSPECIFIED.);
#104=B_SPLINE_CURVE_WITH_KNOTS('',3,(#6251,#6252,#6253,#6254,#6255,#6256,
#6257,#6258,#6259,#6260,#6261,#6262,#6263),.UNSPECIFIED.,.F.,.F.,(4,1,1,
1,1,1,1,1,1,1,4),(15.7079632679489,15.8956852974986,16.3946795877096,16.8936738779205,
17.3926681681314,17.8916624583423,18.3906567485533,18.8896510387642,19.3886453289751,
19.887639619186,20.2892872762916),.UNSPECIFIED.);
#105=B_SPLINE_CURVE_WITH_KNOTS('',3,(#6269,#6270,#6271,#6272,#6273,#6274,
#6275,#6276,#6277,#6278,#6279,#6280,#6281,#6282,#6283,#6284,#6285,#6286,
#6287,#6288,#6289,#6290,#6291,#6292,#6293,#6294,#6295,#6296,#6297,#6298,
#6299,#6300,#6301,#6302,#6303,#6304,#6305,#6306,#6307,#6308,#6309,#6310,
#6311,#6312,#6313,#6314,#6315,#6316,#6317,#6318,#6319,#6320,#6321,#6322,
#6323,#6324,#6325,#6326,#6327,#6328,#6329,#6330,#6331,#6332,#6333,#6334,
#6335,#6336,#6337,#6338,#6339,#6340,#6341,#6342,#6343,#6344,#6345,#6346,
#6347,#6348,#6349,#6350,#6351,#6352,#6353,#6354,#6355,#6356,#6357,#6358,
#6359,#6360,#6361,#6362,#6363,#6364,#6365,#6366,#6367,#6368,#6369,#6370,
#6371,#6372,#6373,#6374,#6375,#6376,#6377,#6378,#6379,#6380,#6381,#6382,
#6383,#6384,#6385,#6386,#6387,#6388,#6389,#6390,#6391,#6392,#6393,#6394,
#6395,#6396,#6397,#6398,#6399,#6400,#6401,#6402,#6403,#6404,#6405,#6406,
#6407,#6408,#6409,#6410,#6411,#6412,#6413,#6414,#6415,#6416,#6417,#6418,
#6419,#6420,#6421,#6422,#6423,#6424,#6425,#6426,#6427,#6428,#6429,#6430,
#6431,#6432,#6433,#6434,#6435,#6436,#6437,#6438,#6439,#6440,#6441,#6442,
#6443,#6444,#6445,#6446,#6447,#6448,#6449,#6450,#6451,#6452,#6453,#6454,
#6455,#6456,#6457,#6458,#6459,#6460,#6461,#6462,#6463,#6464),
 .UNSPECIFIED.,.F.,.F.,(4,3,3,3,3,3,3,3,3,3,3,3,3,3,3,3,3,3,3,3,3,3,3,3,
3,3,3,3,3,3,3,3,3,3,3,3,3,3,3,3,3,3,3,3,3,3,3,3,3,3,3,3,3,3,3,3,3,3,3,3,
3,3,3,3,3,4),(21.9911485751285,22.0611187640108,22.1310953555668,22.2010715824223,
22.2710644969389,22.3309160591743,22.4009566501728,22.4709853447878,22.541006265131,
22.6132322861946,22.683256948635,22.7565836490101,22.8299103493852,22.8999509401425,
22.9699796345137,23.0400005546109,23.1122265758572,23.18225123805,23.2555779388231,
23.3289046395961,23.3989452304404,23.4689739248995,23.5389948450855,23.6112208662659,
23.6812455285474,23.7545722291773,23.8278989298071,23.8979395206352,23.9679682150779,
24.037989135248,24.1102151564405,24.1802398187058,24.2535665193619,24.326893220018,
24.3969338108387,24.4669625052738,24.5369834254368,24.6092094466348,24.6792341088923,
24.7525608095606,24.8258875102289,24.8959281010602,24.9659567955063,25.0359777156793,
25.1082037368695,25.1782283991379,25.2515550997889,25.3248818004398,25.3949223912636,
25.4649510857019,25.5349720058675,25.6071980270633,25.6772226893242,25.7505493899875,
25.8238760906508,25.8939166814786,25.9639453759211,26.0339662960901,26.106192317283,
26.1762169795476,26.2495436802046,26.3228703808617,26.392910974502,26.4629389186468,
26.5329614212261,26.5724975465912),.UNSPECIFIED.);
#106=B_SPLINE_CURVE_WITH_KNOTS('',3,(#6465,#6466,#6467,#6468,#6469,#6470,
#6471,#6472,#6473,#6474,#6475,#6476,#6477,#6478,#6479,#6480,#6481,#6482,
#6483,#6484,#6485,#6486,#6487,#6488,#6489,#6490,#6491,#6492,#6493,#6494,
#6495,#6496,#6497,#6498,#6499,#6500,#6501,#6502,#6503,#6504,#6505,#6506,
#6507,#6508,#6509,#6510,#6511,#6512,#6513,#6514,#6515,#6516,#6517,#6518,
#6519,#6520,#6521,#6522,#6523,#6524,#6525,#6526,#6527,#6528,#6529,#6530,
#6531,#6532,#6533,#6534,#6535,#6536,#6537,#6538,#6539,#6540),
 .UNSPECIFIED.,.F.,.F.,(4,3,3,3,3,3,3,3,3,3,3,3,3,3,3,3,3,3,3,3,3,3,3,3,
3,4),(20.289300242169,20.3349388983306,20.4049794883864,20.4750081820518,
20.5450291014412,20.6172551232163,20.6872797847037,20.7606064866226,20.8339331885415,
20.9039737790573,20.9740024731822,21.0440233930295,21.1162494144602,21.1862740763956,
21.259600777574,21.3329274787524,21.4029680700421,21.4729967649525,21.5430176855947,
21.6152437064369,21.6852683691804,21.7585950690719,21.8319217689634,21.9045986695098,
21.9772545252523,21.9911485750577),.UNSPECIFIED.);
#107=B_SPLINE_CURVE_WITH_KNOTS('',3,(#6542,#6543,#6544,#6545,#6546,#6547,
#6548,#6549),.UNSPECIFIED.,.F.,.F.,(4,1,1,1,1,4),(20.2892872762916,20.386633909397,
20.8856281996079,21.3846224898188,21.8836167800297,21.9911485751285),
 .UNSPECIFIED.);
#108=B_SPLINE_CURVE_WITH_KNOTS('',3,(#6550,#6551,#6552,#6553,#6554,#6555,
#6556,#6557,#6558,#6559,#6560,#6561,#6562,#6563,#6564,#6565,#6566,#6567,
#6568,#6569,#6570,#6571,#6572,#6573,#6574,#6575,#6576,#6577,#6578,#6579,
#6580,#6581,#6582,#6583,#6584,#6585,#6586,#6587,#6588,#6589,#6590,#6591,
#6592,#6593,#6594,#6595,#6596,#6597,#6598,#6599,#6600,#6601,#6602,#6603,
#6604,#6605,#6606,#6607,#6608,#6609,#6610,#6611,#6612,#6613,#6614,#6615,
#6616,#6617,#6618,#6619,#6620,#6621,#6622,#6623,#6624,#6625,#6626,#6627,
#6628,#6629,#6630,#6631,#6632,#6633,#6634,#6635,#6636,#6637,#6638,#6639,
#6640,#6641,#6642,#6643,#6644,#6645,#6646,#6647,#6648,#6649,#6650,#6651,
#6652,#6653,#6654,#6655,#6656,#6657,#6658,#6659,#6660,#6661,#6662,#6663,
#6664,#6665,#6666,#6667,#6668,#6669,#6670,#6671,#6672,#6673,#6674,#6675,
#6676,#6677,#6678,#6679,#6680,#6681,#6682,#6683,#6684,#6685,#6686,#6687,
#6688,#6689,#6690,#6691,#6692,#6693,#6694,#6695,#6696,#6697,#6698,#6699,
#6700,#6701,#6702,#6703,#6704,#6705,#6706,#6707,#6708,#6709,#6710,#6711,
#6712,#6713,#6714,#6715,#6716,#6717,#6718,#6719,#6720,#6721,#6722,#6723,
#6724,#6725,#6726,#6727,#6728,#6729,#6730,#6731,#6732,#6733,#6734,#6735,
#6736,#6737,#6738,#6739,#6740,#6741,#6742,#6743,#6744,#6745),
 .UNSPECIFIED.,.F.,.F.,(4,3,3,3,3,3,3,3,3,3,3,3,3,3,3,3,3,3,3,3,3,3,3,3,
3,3,3,3,3,3,3,3,3,3,3,3,3,3,3,3,3,3,3,3,3,3,3,3,3,3,3,3,3,3,3,3,3,3,3,3,
3,3,3,3,3,4),(21.9911485751285,22.0609174698852,22.1306788205048,22.2004452722809,
22.2702117236623,22.339993679049,22.3826110702406,22.4526516650052,22.522680363424,
22.5927012875987,22.6649273058119,22.7349519721031,22.8082786662773,22.8816053604516,
22.9516459505158,23.0216746441895,23.0916955635876,23.1639215853563,23.2339462468523,
23.3072729487574,23.3805996506625,23.4506402411789,23.5206689353043,23.5906898551522,
23.6629158765825,23.7329405385188,23.8062672396961,23.8795939408734,23.9496345321602,
24.0196632270677,24.0896841477066,24.1619101685511,24.2319348312914,24.3052615311878,
24.3785882310843,24.4486288215852,24.5186575156965,24.5886784355325,24.6609044569732,
24.7309291189009,24.8042558200981,24.8775825212953,24.9476231122925,25.0176518069063,
25.0876727272481,25.1598987483126,25.2299234107518,25.303250111129,25.3765768115062,
25.4466174022641,25.5166460966359,25.5866670167347,25.6588930379803,25.7289177001737,
25.8022444009454,25.8755711017171,25.9456116925611,26.0156403870198,26.0856613072057,
26.1578873283863,26.2279119906681,26.301238691298,26.374565391928,26.4446053180435,
26.5146354344288,26.5725063250621),.UNSPECIFIED.);
#109=B_SPLINE_CURVE_WITH_KNOTS('',3,(#6751,#6752,#6753,#6754,#6755,#6756,
#6757,#6758,#6759,#6760,#6761,#6762,#6763,#6764,#6765,#6766,#6767,#6768,
#6769,#6770,#6771,#6772,#6773,#6774,#6775,#6776,#6777,#6778,#6779,#6780,
#6781,#6782,#6783,#6784,#6785,#6786,#6787,#6788,#6789,#6790,#6791,#6792,
#6793,#6794,#6795,#6796,#6797,#6798,#6799,#6800,#6801,#6802,#6803,#6804,
#6805,#6806,#6807,#6808,#6809,#6810,#6811,#6812,#6813,#6814,#6815,#6816,
#6817,#6818,#6819,#6820,#6821,#6822,#6823,#6824,#6825,#6826,#6827,#6828,
#6829,#6830,#6831,#6832,#6833,#6834,#6835,#6836,#6837,#6838,#6839,#6840,
#6841,#6842,#6843,#6844,#6845,#6846,#6847,#6848,#6849,#6850,#6851,#6852,
#6853,#6854,#6855,#6856,#6857,#6858,#6859,#6860,#6861,#6862,#6863,#6864,
#6865,#6866,#6867,#6868,#6869,#6870,#6871,#6872,#6873,#6874,#6875,#6876,
#6877,#6878,#6879,#6880,#6881,#6882,#6883,#6884,#6885,#6886,#6887,#6888,
#6889,#6890,#6891,#6892,#6893,#6894,#6895,#6896,#6897,#6898,#6899,#6900,
#6901,#6902,#6903,#6904,#6905,#6906,#6907,#6908,#6909,#6910,#6911,#6912,
#6913,#6914,#6915,#6916,#6917,#6918,#6919,#6920,#6921,#6922,#6923,#6924,
#6925,#6926,#6927,#6928,#6929,#6930,#6931,#6932,#6933,#6934,#6935,#6936,
#6937,#6938,#6939,#6940,#6941,#6942,#6943,#6944,#6945,#6946),
 .UNSPECIFIED.,.F.,.F.,(4,3,3,3,3,3,3,3,3,3,3,3,3,3,3,3,3,3,3,3,3,3,3,3,
3,3,3,3,3,3,3,3,3,3,3,3,3,3,3,3,3,3,3,3,3,3,3,3,3,3,3,3,3,3,3,3,3,3,3,3,
3,3,3,3,3,4),(28.2743338823081,28.3188475417054,28.3888881325318,28.4589168269729,
28.5289377471412,28.601163768335,28.6711884305987,28.7445151312575,28.8178418319163,
28.8878824227428,28.9579111171838,29.0279320373515,29.1001580585454,29.170182720809,
29.2435094214681,29.3168361221272,29.3868767129537,29.4569054073949,29.526926327563,
29.5991523487568,29.6691770110205,29.7425037116793,29.8158304123381,29.8858710031646,
29.9558996976058,30.025920617774,30.0981466389678,30.1681713012315,30.2414980018903,
30.3148247025491,30.3848652933756,30.4548939878167,30.5249149079848,30.5971409291786,
30.6671655914423,30.7404922921012,30.81381899276,30.8838595835864,30.9538882780275,
31.0239091981955,31.0961352193893,31.166159881653,31.2394865823119,31.3128132829709,
31.3828538737974,31.4528825682385,31.5229034884066,31.5951295096004,31.6651541718641,
31.7384808725229,31.8118075731818,31.8818481640083,31.9518768584493,32.0218977786175,
32.0941237998113,32.164148462075,32.2374751627339,32.3108018633928,32.3808424542193,
32.4508711486604,32.5208920688285,32.5931180900223,32.6631427522859,32.7364694529448,
32.8097961536037,32.8556949433396),.UNSPECIFIED.);
#110=B_SPLINE_CURVE_WITH_KNOTS('',3,(#6947,#6948,#6949,#6950,#6951,#6952,
#6953,#6954,#6955,#6956,#6957,#6958,#6959,#6960,#6961,#6962,#6963,#6964,
#6965,#6966,#6967,#6968,#6969,#6970,#6971,#6972,#6973,#6974,#6975,#6976,
#6977,#6978,#6979,#6980,#6981,#6982,#6983,#6984,#6985,#6986,#6987,#6988,
#6989,#6990,#6991,#6992,#6993,#6994,#6995,#6996,#6997,#6998,#6999,#7000,
#7001,#7002,#7003,#7004,#7005,#7006,#7007,#7008,#7009,#7010,#7011,#7012,
#7013,#7014,#7015,#7016,#7017,#7018,#7019,#7020,#7021,#7022),
 .UNSPECIFIED.,.F.,.F.,(4,3,3,3,3,3,3,3,3,3,3,3,3,3,3,3,3,3,3,3,3,3,3,3,
3,4),(26.5724975465912,26.6425224627946,26.7125479358874,26.7825880206627,
26.8218646710726,26.8919052618991,26.9619339563403,27.0319548765084,27.1041808977022,
27.1742055599662,27.2475322606249,27.3208589612835,27.3908995521103,27.4609282465518,
27.5309491667197,27.6031751879134,27.6731998501771,27.7465265508357,27.8198532514944,
27.8896727070108,27.9594796023928,28.0292786272708,28.0990816217299,28.1688842155913,
28.238700456284,28.2743338822293),.UNSPECIFIED.);
#111=B_SPLINE_CURVE_WITH_KNOTS('',3,(#7024,#7025,#7026,#7027,#7028,#7029,
#7030,#7031,#7032,#7033,#7034,#7035,#7036,#7037,#7038,#7039,#7040,#7041,
#7042,#7043,#7044,#7045,#7046,#7047,#7048,#7049,#7050,#7051,#7052,#7053,
#7054,#7055,#7056,#7057,#7058,#7059,#7060,#7061,#7062,#7063,#7064,#7065,
#7066,#7067,#7068,#7069,#7070,#7071,#7072,#7073,#7074,#7075,#7076,#7077,
#7078,#7079,#7080,#7081,#7082,#7083,#7084,#7085,#7086,#7087,#7088,#7089,
#7090,#7091,#7092,#7093,#7094,#7095,#7096,#7097,#7098,#7099),
 .UNSPECIFIED.,.F.,.F.,(4,3,3,3,3,3,3,3,3,3,3,3,3,3,3,3,3,3,3,3,3,3,3,3,
3,4),(26.5725063250621,26.6425239289077,26.7125485918865,26.7825748927809,
26.8526147955675,26.8735596821389,26.9436002729595,27.0136289673943,27.0836498875562,
27.1558759087546,27.2259005710118,27.2992272716809,27.3725539723499,27.4425945631809,
27.5126232576271,27.5826441778001,27.6548701989903,27.7248948612584,27.7982215619096,
27.8715482625608,27.9413131725913,28.0110652143382,28.0808150034561,28.1505602216933,
28.2203156472821,28.2743338822406),.UNSPECIFIED.);
#112=B_SPLINE_CURVE_WITH_KNOTS('',3,(#7100,#7101,#7102,#7103,#7104,#7105,
#7106,#7107,#7108,#7109,#7110,#7111,#7112,#7113,#7114,#7115,#7116,#7117,
#7118,#7119,#7120,#7121,#7122,#7123,#7124,#7125,#7126,#7127,#7128,#7129,
#7130,#7131,#7132,#7133,#7134,#7135,#7136,#7137,#7138,#7139,#7140,#7141,
#7142,#7143,#7144,#7145,#7146,#7147,#7148,#7149,#7150,#7151,#7152,#7153,
#7154,#7155,#7156,#7157,#7158,#7159,#7160,#7161,#7162,#7163,#7164,#7165,
#7166,#7167,#7168,#7169,#7170,#7171,#7172,#7173,#7174,#7175,#7176,#7177,
#7178,#7179,#7180,#7181,#7182,#7183,#7184,#7185,#7186,#7187,#7188,#7189,
#7190,#7191,#7192,#7193,#7194,#7195,#7196,#7197,#7198,#7199,#7200,#7201,
#7202,#7203,#7204,#7205,#7206,#7207,#7208,#7209,#7210,#7211,#7212,#7213,
#7214,#7215,#7216,#7217,#7218,#7219,#7220,#7221,#7222,#7223,#7224,#7225,
#7226,#7227,#7228,#7229,#7230,#7231,#7232,#7233,#7234,#7235,#7236,#7237,
#7238,#7239,#7240,#7241,#7242,#7243,#7244,#7245,#7246,#7247,#7248,#7249,
#7250,#7251,#7252,#7253,#7254,#7255,#7256,#7257,#7258,#7259,#7260,#7261,
#7262,#7263,#7264,#7265,#7266,#7267,#7268,#7269,#7270,#7271,#7272,#7273,
#7274,#7275,#7276,#7277,#7278,#7279,#7280,#7281,#7282,#7283,#7284,#7285,
#7286,#7287,#7288,#7289,#7290,#7291,#7292,#7293,#7294,#7295),
 .UNSPECIFIED.,.F.,.F.,(4,3,3,3,3,3,3,3,3,3,3,3,3,3,3,3,3,3,3,3,3,3,3,3,
3,3,3,3,3,3,3,3,3,3,3,3,3,3,3,3,3,3,3,3,3,3,3,3,3,3,3,3,3,3,3,3,3,3,3,3,
3,3,3,3,3,4),(28.2743338823081,28.3488858316158,28.3705425527717,28.4405831435994,
28.5106118380417,28.5806327582111,28.652858779404,28.7228834416689,28.7962101423258,
28.8695368429826,28.9395774338088,29.0096061282494,29.0796270484171,29.1518530696112,
29.2218777318745,29.295204432534,29.3685311331936,29.4385717240202,29.5086004184613,
29.5786213386295,29.6508473598232,29.7208720220869,29.7941987227457,29.8675254234045,
29.937566014231,30.0075947086721,30.0776156288402,30.149841650034,30.2198663122976,
30.2931930129565,30.3665197136154,30.4365603044418,30.5065889988829,30.576609919051,
30.6488359402448,30.7188606025084,30.7921873031673,30.8655140038263,30.9355545946528,
31.005583289094,31.0756042092621,31.1478302304559,31.2178548927196,31.2911815933785,
31.3645082940373,31.4345488848638,31.5045775793049,31.574598499473,31.6468245206668,
31.7168491829305,31.7901758835893,31.8635025842482,31.9335431750747,32.0035718695158,
32.0735927896838,32.1458188108776,32.2158434731413,32.2891701738002,32.3624968744591,
32.4325374038997,32.5025660201463,32.5725868453283,32.643360355704,32.7133845410207,
32.7845327139258,32.8556808868309),.UNSPECIFIED.);
#113=B_SPLINE_CURVE_WITH_KNOTS('',3,(#7301,#7302,#7303,#7304,#7305,#7306,
#7307,#7308,#7309,#7310,#7311,#7312,#7313),.UNSPECIFIED.,.F.,.F.,(4,1,1,
1,1,1,1,1,1,1,4),(34.5575191894877,34.8057733144474,35.3047676046583,35.8037618948692,
36.3027561850801,36.8017504752911,37.300744765502,37.7997390557129,38.2987333459238,
38.7977276361348,39.138844988577),.UNSPECIFIED.);
#114=B_SPLINE_CURVE_WITH_KNOTS('',3,(#7314,#7315,#7316,#7317,#7318,#7319,
#7320,#7321,#7322,#7323,#7324,#7325,#7326,#7327,#7328,#7329,#7330,#7331,
#7332,#7333,#7334,#7335,#7336,#7337,#7338,#7339,#7340,#7341,#7342,#7343,
#7344,#7345,#7346,#7347,#7348,#7349,#7350,#7351,#7352,#7353,#7354,#7355,
#7356,#7357,#7358,#7359,#7360,#7361,#7362,#7363,#7364,#7365,#7366,#7367,
#7368,#7369,#7370,#7371,#7372,#7373,#7374,#7375,#7376,#7377,#7378,#7379,
#7380,#7381,#7382,#7383,#7384,#7385,#7386,#7387,#7388,#7389),
 .UNSPECIFIED.,.F.,.F.,(4,3,3,3,3,3,3,3,3,3,3,3,3,3,3,3,3,3,3,3,3,3,3,3,
3,4),(32.8556949433396,32.9257272727589,32.9957504074315,33.0657684672156,
33.1357932637452,33.205818991343,33.2758589616207,33.3087904438146,33.378831034641,
33.4488597290822,33.5188806492501,33.591106670444,33.6611313327076,33.7344580333666,
33.8077847340255,33.877825324852,33.9478540192931,34.0178749394612,34.090100960655,
34.1601256229187,34.2334523235775,34.3067790242364,34.3776775785114,34.4485623759747,
34.5194352520091,34.5575191894138),.UNSPECIFIED.);
#115=B_SPLINE_CURVE_WITH_KNOTS('',3,(#7391,#7392,#7393,#7394,#7395,#7396,
#7397,#7398,#7399,#7400,#7401,#7402,#7403,#7404,#7405,#7406,#7407,#7408,
#7409,#7410,#7411,#7412,#7413,#7414,#7415,#7416,#7417,#7418,#7419,#7420,
#7421,#7422,#7423,#7424,#7425,#7426,#7427,#7428,#7429,#7430,#7431,#7432,
#7433,#7434,#7435,#7436,#7437,#7438,#7439,#7440,#7441,#7442,#7443,#7444,
#7445,#7446,#7447,#7448,#7449,#7450,#7451,#7452,#7453,#7454,#7455,#7456,
#7457,#7458,#7459,#7460,#7461,#7462,#7463,#7464,#7465,#7466),
 .UNSPECIFIED.,.F.,.F.,(4,3,3,3,3,3,3,3,3,3,3,3,3,3,3,3,3,3,3,3,3,3,3,3,
3,4),(32.8556808868309,32.86149116467,32.9315317554965,33.0015604499375,
33.0715813701057,33.1438073912995,33.2138320535632,33.2871587542221,33.3604854548809,
33.4305260457074,33.5005547401485,33.5705756603166,33.6428016815104,33.712826343774,
33.786153044433,33.8594797450919,33.9295203359184,33.9995490303595,34.0695699505274,
34.1417959717213,34.211820633985,34.2851473346439,34.3584740353028,34.4302564390369,
34.5020210945599,34.557519189415),.UNSPECIFIED.);
#116=B_SPLINE_CURVE_WITH_KNOTS('',3,(#7467,#7468,#7469,#7470,#7471,#7472,
#7473,#7474,#7475,#7476,#7477,#7478,#7479,#7480,#7481,#7482,#7483,#7484,
#7485,#7486,#7487,#7488,#7489,#7490,#7491,#7492,#7493,#7494,#7495,#7496,
#7497,#7498,#7499,#7500,#7501,#7502,#7503,#7504,#7505,#7506,#7507,#7508,
#7509,#7510,#7511,#7512,#7513,#7514,#7515,#7516,#7517,#7518,#7519,#7520,
#7521,#7522,#7523,#7524,#7525,#7526,#7527,#7528,#7529,#7530,#7531,#7532,
#7533,#7534,#7535,#7536,#7537,#7538,#7539,#7540,#7541,#7542,#7543,#7544,
#7545,#7546,#7547,#7548,#7549,#7550,#7551,#7552,#7553,#7554,#7555,#7556,
#7557,#7558,#7559,#7560,#7561,#7562,#7563,#7564,#7565,#7566,#7567,#7568,
#7569,#7570,#7571,#7572,#7573,#7574,#7575,#7576,#7577,#7578,#7579,#7580,
#7581,#7582,#7583,#7584,#7585,#7586,#7587,#7588,#7589,#7590,#7591,#7592,
#7593,#7594,#7595,#7596,#7597,#7598,#7599,#7600,#7601,#7602,#7603,#7604,
#7605,#7606,#7607,#7608,#7609,#7610,#7611,#7612,#7613,#7614,#7615,#7616,
#7617,#7618,#7619,#7620,#7621,#7622,#7623,#7624,#7625,#7626,#7627,#7628,
#7629,#7630,#7631,#7632,#7633,#7634,#7635,#7636,#7637,#7638,#7639,#7640,
#7641,#7642,#7643,#7644,#7645,#7646,#7647,#7648,#7649,#7650,#7651,#7652,
#7653,#7654,#7655,#7656,#7657,#7658,#7659,#7660,#7661,#7662),
 .UNSPECIFIED.,.F.,.F.,(4,3,3,3,3,3,3,3,3,3,3,3,3,3,3,3,3,3,3,3,3,3,3,3,
3,3,3,3,3,3,3,3,3,3,3,3,3,3,3,3,3,3,3,3,3,3,3,3,3,3,3,3,3,3,3,3,3,3,3,3,
3,3,3,3,3,4),(34.5575191894877,34.6277996055737,34.6980904637057,34.7683845128919,
34.8386929125139,34.8574683255137,34.9275089163402,34.9975376107813,35.0675585309494,
35.1397845521432,35.2098092144068,35.2831359150657,35.3564626157246,35.4265032065511,
35.4965319009923,35.5665528211606,35.6387788423543,35.7088035046181,35.7821302052769,
35.8554569059356,35.9254974967621,35.9955261912033,36.0655471113711,36.137773132565,
36.2077977948286,36.2811244954875,36.3544511961465,36.424491786973,36.4945204814141,
36.5645414015817,36.6367674227756,36.7067920850394,36.7801187856984,36.8534454863574,
36.9234860771838,36.9935147716249,37.0635356917926,37.1357617129865,37.2057863752504,
37.2791130759094,37.3524397765683,37.4224803673948,37.4925090618357,37.5625299820039,
37.6347560031977,37.7047806654614,37.7781073661203,37.8514340667792,37.9214746576057,
37.9915033520468,38.0615242722151,38.1337502934089,38.2037749556726,38.2771016563314,
38.3504283569902,38.4204689478168,38.4904976422578,38.5605185624258,38.6327445836196,
38.702769245883,38.776095946542,38.8494226472011,38.9217823054225,38.9918107826881,
39.0653360313874,39.1388612800867),.UNSPECIFIED.);
#117=B_SPLINE_CURVE_WITH_KNOTS('',3,(#7668,#7669,#7670,#7671,#7672,#7673,
#7674,#7675,#7676,#7677,#7678,#7679,#7680,#7681,#7682,#7683,#7684,#7685,
#7686,#7687,#7688,#7689,#7690,#7691,#7692,#7693,#7694,#7695,#7696,#7697,
#7698,#7699,#7700,#7701,#7702,#7703,#7704,#7705,#7706,#7707,#7708,#7709,
#7710,#7711,#7712,#7713,#7714,#7715,#7716,#7717,#7718,#7719,#7720,#7721,
#7722,#7723,#7724,#7725,#7726,#7727,#7728,#7729,#7730,#7731,#7732,#7733,
#7734,#7735,#7736,#7737,#7738,#7739,#7740,#7741,#7742,#7743,#7744,#7745,
#7746,#7747,#7748,#7749,#7750,#7751,#7752,#7753,#7754,#7755,#7756,#7757,
#7758,#7759,#7760,#7761,#7762,#7763,#7764,#7765,#7766,#7767,#7768,#7769,
#7770,#7771,#7772,#7773,#7774,#7775,#7776,#7777,#7778,#7779,#7780,#7781,
#7782,#7783,#7784,#7785,#7786,#7787,#7788,#7789,#7790,#7791,#7792,#7793,
#7794,#7795,#7796,#7797,#7798,#7799,#7800,#7801,#7802,#7803,#7804,#7805,
#7806,#7807,#7808,#7809,#7810,#7811,#7812,#7813,#7814,#7815,#7816,#7817,
#7818,#7819,#7820,#7821,#7822,#7823,#7824,#7825,#7826,#7827,#7828,#7829,
#7830,#7831,#7832,#7833,#7834,#7835,#7836,#7837,#7838,#7839,#7840,#7841,
#7842,#7843,#7844,#7845,#7846,#7847,#7848,#7849,#7850,#7851,#7852,#7853,
#7854,#7855,#7856,#7857,#7858,#7859,#7860,#7861,#7862,#7863),
 .UNSPECIFIED.,.F.,.F.,(4,3,3,3,3,3,3,3,3,3,3,3,3,3,3,3,3,3,3,3,3,3,3,3,
3,3,3,3,3,3,3,3,3,3,3,3,3,3,3,3,3,3,3,3,3,3,3,3,3,3,3,3,3,3,3,3,3,3,3,3,
3,3,3,3,3,4),(40.8407044966673,40.910513107026,40.9803103162599,41.050100831576,
41.1198969722149,41.1896937756429,41.2595054868552,41.2926990871894,41.3627396780171,
41.4327683724595,41.5027892926283,41.5750153138213,41.645039976086,41.7183666767432,
41.7916933774003,41.861733968224,41.9317626626622,42.0017835828273,42.0740096040233,
42.1440342662842,42.2173609669477,42.2906876676112,42.3607282584425,42.4307569528887,
42.5007778730621,42.5730038942521,42.6430285565208,42.7163552571714,42.7896819578221,
42.8597225486426,42.9297512430777,42.9997721632399,43.0719981844382,43.1420228466959,
43.2153495473645,43.2886762480331,43.3587168388615,43.4287455333043,43.4987664534742,
43.5709924746666,43.641017136932,43.714343837588,43.787670538244,43.8577111290883,
43.9277398235473,43.9977607437335,44.0699867649139,44.1400114271953,44.2133381278251,
44.2866648284549,44.356705419211,44.426734113581,44.4967550336782,44.5689810549251,
44.6390057171185,44.7123324178922,44.7856591186658,44.8556997096685,44.9257284042865,
44.9957493246311,45.0679753456925,45.1380000081308,45.2113267085037,45.2846534088767,
45.3546946558375,45.4220693616144),.UNSPECIFIED.);
#118=B_SPLINE_CURVE_WITH_KNOTS('',3,(#7864,#7865,#7866,#7867,#7868,#7869,
#7870,#7871),.UNSPECIFIED.,.F.,.F.,(4,1,1,1,1,4),(39.138844988577,39.2967219263457,
39.7957162165566,40.2947105067675,40.7937047969784,40.8407044966673),
 .UNSPECIFIED.);
#119=B_SPLINE_CURVE_WITH_KNOTS('',3,(#7873,#7874,#7875,#7876,#7877,#7878,
#7879,#7880,#7881,#7882,#7883,#7884,#7885,#7886,#7887,#7888,#7889,#7890,
#7891,#7892,#7893,#7894,#7895,#7896,#7897,#7898,#7899,#7900,#7901,#7902,
#7903,#7904,#7905,#7906,#7907,#7908,#7909,#7910,#7911,#7912,#7913,#7914,
#7915,#7916,#7917,#7918,#7919,#7920,#7921,#7922,#7923,#7924,#7925,#7926,
#7927,#7928,#7929,#7930,#7931,#7932,#7933,#7934,#7935,#7936,#7937,#7938,
#7939,#7940,#7941,#7942,#7943,#7944,#7945),.UNSPECIFIED.,.F.,.F.,(4,3,3,
3,3,3,3,3,3,3,3,3,3,3,3,3,3,3,3,3,3,3,3,3,4),(39.1388612800867,39.2088860064159,
39.2789273844965,39.348416937412,39.4184575282385,39.4884862226791,39.5585071428482,
39.6307331640419,39.7007578263056,39.7740845269643,39.8474112276229,39.9174518184494,
39.9874805128906,40.0575014330589,40.1297274542526,40.1997521165164,40.2730788171751,
40.3464055178339,40.4164150422325,40.4864125754172,40.5564023218123,40.6274778655123,
40.6974714282655,40.7690879624389,40.8407044966123),.UNSPECIFIED.);
#120=B_SPLINE_CURVE_WITH_KNOTS('',3,(#7946,#7947,#7948,#7949,#7950,#7951,
#7952,#7953,#7954,#7955,#7956,#7957,#7958,#7959,#7960,#7961,#7962,#7963,
#7964,#7965,#7966,#7967,#7968,#7969,#7970,#7971,#7972,#7973,#7974,#7975,
#7976,#7977,#7978,#7979,#7980,#7981,#7982,#7983,#7984,#7985,#7986,#7987,
#7988,#7989,#7990,#7991,#7992,#7993,#7994,#7995,#7996,#7997,#7998,#7999,
#8000,#8001,#8002,#8003,#8004,#8005,#8006,#8007,#8008,#8009,#8010,#8011,
#8012,#8013,#8014,#8015,#8016,#8017,#8018,#8019,#8020,#8021,#8022,#8023,
#8024,#8025,#8026,#8027,#8028,#8029,#8030,#8031,#8032,#8033,#8034,#8035,
#8036,#8037,#8038,#8039,#8040,#8041,#8042,#8043,#8044,#8045,#8046,#8047,
#8048,#8049,#8050,#8051,#8052,#8053,#8054,#8055,#8056,#8057,#8058,#8059,
#8060,#8061,#8062,#8063,#8064,#8065,#8066,#8067,#8068,#8069,#8070,#8071,
#8072,#8073,#8074,#8075,#8076,#8077,#8078,#8079,#8080,#8081,#8082,#8083,
#8084,#8085,#8086,#8087,#8088,#8089,#8090,#8091,#8092,#8093,#8094,#8095,
#8096,#8097,#8098,#8099,#8100,#8101,#8102,#8103,#8104,#8105,#8106,#8107,
#8108,#8109,#8110,#8111,#8112,#8113,#8114,#8115,#8116,#8117,#8118,#8119,
#8120,#8121,#8122,#8123,#8124,#8125,#8126,#8127,#8128,#8129,#8130,#8131,
#8132,#8133,#8134,#8135,#8136,#8137,#8138,#8139,#8140,#8141,#8142,#8143,
#8144),.UNSPECIFIED.,.F.,.F.,(4,3,3,3,3,3,3,3,3,3,3,3,3,3,3,3,3,3,3,3,3,
3,3,3,3,3,3,3,3,3,3,3,3,3,3,3,3,3,3,3,3,3,3,3,3,3,3,3,3,3,3,3,3,3,3,3,3,
3,3,3,3,3,3,3,3,3,4),(40.8407044966673,40.8453998080448,40.9154403988712,
40.9854690933122,41.0554900134805,41.1277160346743,41.1977406969378,41.2710673975968,
41.3443940982557,41.4144346890823,41.4844633835235,41.5544843036917,41.6267103248854,
41.6967349871492,41.7700616878079,41.8433883884666,41.913428979293,41.9834576737341,
42.0534785939022,42.1257046150961,42.1957292773597,42.2690559780186,42.3423826786776,
42.4124232695042,42.4824519639455,42.5524728841137,42.6246989053074,42.6947235675711,
42.7680502682298,42.8413769688885,42.911417559715,42.9814462541562,43.0514671743242,
43.123693195518,43.1937178577816,43.2670445584405,43.3403712590994,43.4104118499255,
43.4804405443662,43.550461464534,43.6226874857281,43.6927121479913,43.7660388486508,
43.8393655493103,43.909406140138,43.9794348345803,44.0494557547496,44.1216817759425,
44.1917064382073,44.2650331388643,44.3383598395212,44.408400430345,44.4784291247834,
44.5484500449487,44.6206760661446,44.6907007284056,44.7640274290689,44.8373541297322,
44.9073947205635,44.9774234150094,45.0474443351823,45.1196703563725,45.189695018641,
45.263021719292,45.3363484199431,45.4063883545637,45.4220700257397),
 .UNSPECIFIED.);
#121=B_SPLINE_CURVE_WITH_KNOTS('',3,(#8150,#8151,#8152,#8153,#8154,#8155,
#8156,#8157,#8158,#8159,#8160,#8161,#8162,#8163,#8164,#8165,#8166,#8167,
#8168,#8169,#8170,#8171,#8172,#8173,#8174,#8175,#8176,#8177,#8178,#8179,
#8180,#8181,#8182,#8183,#8184,#8185,#8186,#8187,#8188,#8189,#8190,#8191,
#8192,#8193,#8194,#8195,#8196,#8197,#8198,#8199,#8200,#8201,#8202,#8203,
#8204,#8205,#8206,#8207,#8208,#8209,#8210,#8211,#8212,#8213,#8214,#8215,
#8216,#8217,#8218,#8219,#8220,#8221,#8222,#8223,#8224,#8225,#8226,#8227,
#8228,#8229,#8230,#8231,#8232,#8233,#8234,#8235,#8236,#8237,#8238,#8239,
#8240,#8241,#8242,#8243,#8244,#8245,#8246,#8247,#8248,#8249,#8250,#8251,
#8252,#8253,#8254,#8255,#8256,#8257,#8258,#8259,#8260,#8261,#8262,#8263,
#8264,#8265,#8266,#8267,#8268,#8269,#8270,#8271,#8272,#8273,#8274,#8275,
#8276,#8277,#8278,#8279,#8280,#8281,#8282,#8283,#8284,#8285,#8286,#8287,
#8288,#8289,#8290,#8291,#8292,#8293,#8294,#8295,#8296,#8297,#8298,#8299,
#8300,#8301,#8302,#8303,#8304,#8305,#8306,#8307,#8308,#8309,#8310,#8311,
#8312,#8313,#8314,#8315,#8316,#8317,#8318,#8319,#8320,#8321,#8322,#8323,
#8324,#8325,#8326,#8327,#8328,#8329,#8330,#8331,#8332,#8333,#8334,#8335,
#8336,#8337,#8338,#8339,#8340,#8341,#8342,#8343,#8344,#8345,#8346,#8347,
#8348),.UNSPECIFIED.,.F.,.F.,(4,3,3,3,3,3,3,3,3,3,3,3,3,3,3,3,3,3,3,3,3,
3,3,3,3,3,3,3,3,3,3,3,3,3,3,3,3,3,3,3,3,3,3,3,3,3,3,3,3,3,3,3,3,3,3,3,3,
3,3,3,3,3,3,3,3,3,4),(47.1238898039153,47.1966069931218,47.269346291875,
47.2806305697204,47.3506711645816,47.4206998630754,47.4907207873035,47.5629468054605,
47.6329714717519,47.7062981658417,47.7796248599314,47.8496654396268,47.919694122898,
47.9897150318869,48.0619410614508,48.1319657126511,48.2052924313967,48.2786191501423,
48.3486597639494,48.4186884814349,48.4887094246505,48.5609354285762,48.6309601136108,
48.704286776982,48.7776134403532,48.8476539950211,48.9176826532346,48.987703537201,
49.0599295855418,49.1299542121136,49.2032809713389,49.2766077305641,49.3466483562613,
49.4166770855596,49.486698040481,49.5589240355545,49.6289487318888,49.702275376332,
49.7756020207751,49.8456426343618,49.9156713518887,49.9856922954051,50.0579182993003,
50.1279429852639,50.201269648125,50.274596310986,50.3446366811021,50.4146651537395,
50.4846858515977,50.5569120389975,50.6269364804616,50.7002635408293,50.7735906011969,
50.8436318783237,50.9136612616073,50.9836828713458,51.0559083763613,51.1259337214531,
51.1992593064304,51.2725848914078,51.3426234218437,51.4126498588465,51.4857933163341,
51.5558129797052,51.6258314628023,51.695858176314,51.705223688797),
 .UNSPECIFIED.);
#122=B_SPLINE_CURVE_WITH_KNOTS('',3,(#8349,#8350,#8351,#8352,#8353,#8354,
#8355,#8356,#8357,#8358,#8359,#8360,#8361,#8362,#8363,#8364,#8365,#8366,
#8367,#8368,#8369,#8370,#8371,#8372,#8373,#8374,#8375,#8376,#8377,#8378,
#8379,#8380,#8381,#8382,#8383,#8384,#8385,#8386,#8387,#8388,#8389,#8390,
#8391,#8392,#8393,#8394,#8395,#8396,#8397,#8398,#8399,#8400,#8401,#8402,
#8403,#8404,#8405,#8406,#8407,#8408,#8409,#8410,#8411,#8412,#8413,#8414,
#8415,#8416,#8417,#8418,#8419,#8420,#8421,#8422,#8423,#8424),
 .UNSPECIFIED.,.F.,.F.,(4,3,3,3,3,3,3,3,3,3,3,3,3,3,3,3,3,3,3,3,3,3,3,3,
3,4),(45.4220693616144,45.4920905009292,45.5649798004688,45.6350044521349,
45.7050314710928,45.7750715078873,45.7836476990877,45.8536882903937,45.9237169853146,
45.9937379059628,46.0659639267968,46.1359885895327,46.2093152894156,46.2826419892986,
46.3526825797948,46.4227112739064,46.4927321937468,46.5649582151875,46.6349828771319,
46.7083095783207,46.7816362795095,46.8516132827516,46.9215804164053,46.9915381364908,
47.0614983061719,47.1238898038469),.UNSPECIFIED.);
#123=B_SPLINE_CURVE_WITH_KNOTS('',3,(#8426,#8427,#8428,#8429,#8430,#8431,
#8432,#8433,#8434,#8435,#8436,#8437,#8438,#8439,#8440,#8441,#8442,#8443,
#8444,#8445,#8446,#8447,#8448,#8449,#8450,#8451,#8452,#8453,#8454,#8455,
#8456,#8457,#8458,#8459,#8460,#8461,#8462,#8463,#8464,#8465,#8466,#8467,
#8468,#8469,#8470,#8471,#8472,#8473,#8474,#8475,#8476,#8477,#8478,#8479,
#8480,#8481,#8482,#8483,#8484,#8485,#8486,#8487,#8488,#8489,#8490,#8491,
#8492,#8493,#8494,#8495,#8496,#8497,#8498),.UNSPECIFIED.,.F.,.F.,(4,3,3,
3,3,3,3,3,3,3,3,3,3,3,3,3,3,3,3,3,3,3,3,3,4),(45.4220700257397,45.492096621416,
45.562116365311,45.6321420349469,45.7021668544972,45.7722078578491,45.835342710154,
45.9053833009824,45.9754119954253,46.045432915595,46.1176589367875,46.1876835990528,
46.2610102997088,46.3343370003649,46.4043775912091,46.4744062856679,46.544427205854,
46.6166532270345,46.6866778893158,46.7600045899459,46.8333312905759,46.9059709188937,
46.9763616597276,47.0501257317873,47.1238898038469),.UNSPECIFIED.);
#124=B_SPLINE_CURVE_WITH_KNOTS('',3,(#8499,#8500,#8501,#8502,#8503,#8504,
#8505,#8506,#8507,#8508,#8509,#8510,#8511,#8512,#8513,#8514,#8515,#8516,
#8517,#8518,#8519,#8520,#8521,#8522,#8523,#8524,#8525,#8526,#8527,#8528,
#8529,#8530,#8531,#8532,#8533,#8534,#8535,#8536,#8537,#8538,#8539,#8540,
#8541,#8542,#8543,#8544,#8545,#8546,#8547,#8548,#8549,#8550,#8551,#8552,
#8553,#8554,#8555,#8556,#8557,#8558,#8559,#8560,#8561,#8562,#8563,#8564,
#8565,#8566,#8567,#8568,#8569,#8570,#8571,#8572,#8573,#8574,#8575,#8576,
#8577,#8578,#8579,#8580,#8581,#8582,#8583,#8584,#8585,#8586,#8587,#8588,
#8589,#8590,#8591,#8592,#8593,#8594,#8595,#8596,#8597,#8598,#8599,#8600,
#8601,#8602,#8603,#8604,#8605,#8606,#8607,#8608,#8609,#8610,#8611,#8612,
#8613,#8614,#8615,#8616,#8617,#8618,#8619,#8620,#8621,#8622,#8623,#8624,
#8625,#8626,#8627,#8628,#8629,#8630,#8631,#8632,#8633,#8634,#8635,#8636,
#8637,#8638,#8639,#8640,#8641,#8642,#8643,#8644,#8645,#8646,#8647,#8648,
#8649,#8650,#8651,#8652,#8653,#8654,#8655,#8656,#8657,#8658,#8659,#8660,
#8661,#8662,#8663,#8664,#8665,#8666,#8667,#8668,#8669,#8670,#8671,#8672,
#8673,#8674,#8675,#8676,#8677,#8678,#8679,#8680,#8681,#8682,#8683,#8684,
#8685,#8686,#8687,#8688,#8689,#8690,#8691,#8692,#8693,#8694),
 .UNSPECIFIED.,.F.,.F.,(4,3,3,3,3,3,3,3,3,3,3,3,3,3,3,3,3,3,3,3,3,3,3,3,
3,3,3,3,3,3,3,3,3,3,3,3,3,3,3,3,3,3,3,3,3,3,3,3,3,3,3,3,3,3,3,3,3,3,3,3,
3,3,3,3,3,4),(47.1238898039108,47.1954657532806,47.2670653523193,47.3323255807868,
47.4023661717881,47.4723948664045,47.5424157867478,47.6146418078103,47.6846664702475,
47.7579931706226,47.8313198709977,47.9013604614893,47.9713891555945,48.0414100754268,
48.1136360968722,48.1836607588042,48.2569874600064,48.3303141612086,48.4003547525115,
48.4703834474297,48.5404043680745,48.6126303889108,48.6826550516439,48.7559817515317,
48.8293084514195,48.8993490419166,48.9693777360291,49.0393986558705,49.1116246773105,
49.1816493392556,49.2549760404431,49.3283027416305,49.3983433316981,49.4683720253742,
49.5383929447734,49.6106189665404,49.6806436280347,49.753970329938,49.8272970318414,
49.8973376266718,49.9673663251347,50.0373872493318,50.1096132675119,50.1796379337725,
50.2529646279124,50.3262913220523,50.3963319018199,50.4663605851638,50.5363814942255,
50.6086075237349,50.678632175007,50.7519588936351,50.8252856122632,50.8953262259418,
50.9653549432983,51.0353758863851,51.1076018904074,51.1776265753145,51.2509532388944,
51.3242799024742,51.3943197709416,51.4643474012373,51.5343709622389,51.6043893378668,
51.6744125951888,51.7052219494017),.UNSPECIFIED.);
#125=B_SPLINE_CURVE_WITH_KNOTS('',3,(#8700,#8701,#8702,#8703),
 .UNSPECIFIED.,.F.,.F.,(4,4),(7.59244615558812,7.94961020078307),
 .UNSPECIFIED.);
#126=B_SPLINE_CURVE_WITH_KNOTS('',3,(#8705,#8706,#8707,#8708,#8709,#8710,
#8711,#8712,#8713,#8714,#8715,#8716,#8717,#8718,#8719,#8720,#8721,#8722,
#8723,#8724,#8725,#8726,#8727,#8728,#8729,#8730,#8731,#8732,#8733,#8734,
#8735,#8736,#8737,#8738,#8739,#8740,#8741,#8742,#8743,#8744,#8745,#8746,
#8747,#8748,#8749,#8750,#8751,#8752,#8753,#8754,#8755,#8756,#8757,#8758,
#8759,#8760,#8761,#8762,#8763,#8764,#8765,#8766,#8767,#8768,#8769,#8770,
#8771,#8772,#8773,#8774,#8775,#8776,#8777,#8778,#8779,#8780,#8781,#8782,
#8783,#8784,#8785,#8786,#8787,#8788,#8789,#8790,#8791,#8792,#8793,#8794,
#8795,#8796,#8797,#8798,#8799,#8800,#8801,#8802,#8803,#8804,#8805,#8806,
#8807,#8808,#8809,#8810,#8811,#8812,#8813,#8814,#8815,#8816,#8817,#8818,
#8819,#8820,#8821,#8822,#8823,#8824,#8825,#8826,#8827,#8828,#8829,#8830,
#8831,#8832,#8833,#8834,#8835,#8836,#8837,#8838,#8839,#8840,#8841,#8842,
#8843,#8844,#8845,#8846,#8847,#8848,#8849,#8850,#8851,#8852,#8853,#8854,
#8855,#8856,#8857,#8858,#8859,#8860,#8861,#8862,#8863,#8864,#8865,#8866,
#8867,#8868,#8869,#8870,#8871,#8872,#8873,#8874,#8875,#8876,#8877,#8878,
#8879,#8880,#8881,#8882,#8883,#8884,#8885,#8886,#8887,#8888,#8889,#8890,
#8891,#8892,#8893,#8894,#8895,#8896,#8897,#8898,#8899,#8900,#8901,#8902,
#8903,#8904,#8905,#8906,#8907,#8908,#8909,#8910,#8911,#8912,#8913,#8914,
#8915,#8916,#8917,#8918,#8919,#8920,#8921,#8922,#8923,#8924,#8925,#8926,
#8927,#8928,#8929,#8930,#8931,#8932,#8933,#8934,#8935,#8936,#8937,#8938,
#8939,#8940,#8941,#8942),.UNSPECIFIED.,.F.,.F.,(4,3,3,3,3,3,3,3,3,3,3,3,
3,3,3,3,3,3,3,3,3,3,3,3,3,3,3,3,3,3,3,3,3,3,3,3,3,3,3,3,3,3,3,3,3,3,3,3,
3,3,3,3,3,3,3,3,3,3,3,3,3,3,3,3,3,3,3,3,3,3,3,3,3,3,3,3,3,3,3,4),(2.02359556728784,
2.09612063785746,2.16863302303831,2.24113775293914,2.31364811582229,2.38615861296181,
2.45868474905377,2.49497145105461,2.56765002727523,2.64031589890252,2.71297367059207,
2.78563719645063,2.85829941345175,2.93097867400525,2.99396574126554,3.06664098081929,
3.13930345029594,3.21195776421116,3.28461777093719,3.35727644001194,3.42995213051997,
3.49296003147646,3.56564099670242,3.63830926977429,3.71096944845288,3.78363537238572,
3.85629997895852,3.92898159803042,3.99195432168738,4.06463110674485,4.13729514772769,
4.20995105460737,4.28261267608536,4.35527296959601,4.42795028890615,4.49094861189831,
4.56362763260635,4.63629393530697,4.70895212345169,4.78161603998939,4.85427863280186,
4.92695824199939,4.98994290210923,5.06262100423254,5.1352863784211,5.20794363080207,
5.28060660711106,5.35326825861507,5.42594693144099,5.48893719232016,5.56161554328838,
5.63428116853687,5.70693867347046,5.77960190281452,5.85226380724567,5.92494273101668,
5.98793148253108,6.06060984370026,6.13327547967456,6.20593299582697,6.27859623707525,
6.35125815377287,6.42393709031945,6.486925772742,6.55960406326347,6.63226962758147,
6.70492707127597,6.77759023934746,6.85025208257815,6.92293094570417,6.98592006295293,
7.05859841273454,7.13126403706467,7.20392154135016,7.27658477047137,7.3492466749157,
7.42192559908852,7.48491435316385,7.56187309461106,7.59244614826265),
 .UNSPECIFIED.);
#127=B_SPLINE_CURVE_WITH_KNOTS('',3,(#8945,#8946,#8947,#8948,#8949,#8950,
#8951,#8952,#8953,#8954,#8955,#8956,#8957,#8958,#8959,#8960,#8961,#8962,
#8963,#8964,#8965,#8966,#8967,#8968,#8969,#8970,#8971,#8972,#8973,#8974,
#8975,#8976,#8977,#8978,#8979,#8980,#8981,#8982,#8983,#8984,#8985,#8986,
#8987,#8988,#8989,#8990,#8991,#8992,#8993,#8994,#8995,#8996,#8997,#8998,
#8999,#9000,#9001,#9002,#9003,#9004,#9005,#9006,#9007,#9008,#9009,#9010,
#9011,#9012,#9013,#9014),.UNSPECIFIED.,.F.,.F.,(4,2,2,2,2,2,2,2,2,2,2,2,
2,2,2,2,2,2,2,2,2,2,2,2,2,2,2,2,2,2,2,2,2,2,4),(0.000135688236192026,0.182534690442223,
0.329186859064794,0.430874046907693,0.509112081933848,0.621923710755093,
0.759294802457872,0.927030288955933,1.02288050568415,1.13549080719406,1.27678418460036,
1.46799932847935,1.55466406176925,1.66507905500832,1.80304759971923,1.99678085625352,
2.0809754199086,2.18736690979933,2.32733794325047,2.51744206634343,2.60414998945933,
2.71106797400003,2.85081076527383,3.0461407368146,3.13059907723473,3.24204658312837,
3.38004050519128,3.55146567007771,3.64685346840213,3.75941222161808,3.89978325985654,
4.0956229489707,4.18023039862239,4.29380952169095,4.43103355894701),
 .UNSPECIFIED.);
#128=B_SPLINE_CURVE_WITH_KNOTS('',3,(#9020,#9021,#9022,#9023,#9024,#9025,
#9026,#9027,#9028,#9029),.UNSPECIFIED.,.F.,.F.,(4,2,2,2,4),(12.8422919822627,
12.887154762158,13.0258167989269,13.1186138717486,13.2178341603313),
 .UNSPECIFIED.);
#129=B_SPLINE_CURVE_WITH_KNOTS('',3,(#9030,#9031,#9032,#9033,#9034,#9035,
#9036,#9037,#9038,#9039,#9040,#9041,#9042,#9043,#9044,#9045),
 .UNSPECIFIED.,.F.,.F.,(4,1,1,1,1,1,1,1,1,1,1,1,1,4),(7.94961020078307,
7.98390864337477,8.48290293358569,8.98189722379661,9.48089151400754,9.97988580421846,
10.4788800944294,10.9778743846403,11.4768686748512,11.9758629650621,12.4748572552731,
12.973851545484,13.4728458356949,13.8756314554422),.UNSPECIFIED.);
#130=B_SPLINE_CURVE_WITH_KNOTS('',3,(#9046,#9047,#9048,#9049,#9050,#9051,
#9052,#9053,#9054,#9055,#9056,#9057,#9058,#9059,#9060,#9061,#9062,#9063,
#9064,#9065,#9066,#9067,#9068,#9069,#9070,#9071,#9072,#9073,#9074,#9075,
#9076,#9077,#9078,#9079,#9080,#9081,#9082,#9083,#9084,#9085,#9086,#9087,
#9088,#9089,#9090,#9091,#9092,#9093,#9094,#9095,#9096,#9097,#9098,#9099,
#9100,#9101,#9102,#9103,#9104,#9105,#9106,#9107,#9108,#9109,#9110,#9111,
#9112,#9113,#9114,#9115,#9116,#9117,#9118,#9119,#9120,#9121,#9122,#9123,
#9124,#9125,#9126,#9127,#9128,#9129,#9130,#9131,#9132,#9133,#9134,#9135,
#9136,#9137,#9138,#9139,#9140,#9141,#9142,#9143,#9144,#9145),
 .UNSPECIFIED.,.F.,.F.,(4,2,2,2,2,2,2,2,2,2,2,2,2,2,2,2,2,2,2,2,2,2,2,2,
2,2,2,2,2,2,2,2,2,2,2,2,2,2,2,2,2,2,2,2,2,2,2,2,2,4),(4.43103355894701,
4.43112108136264,4.5974129920961,4.6949760496939,4.80225796218608,4.94513629188488,
5.14304951890869,5.22888262205294,5.33530324797899,5.47522895906651,5.67102573081961,
5.75521840543593,5.85791461303463,5.99864276279524,6.19466351084876,6.27953142305181,
6.39127651196381,6.52922847922396,6.70026604013396,6.79590080792733,6.97576906914361,
7.1369089391772,7.32967716260638,7.44353181543372,7.58080169596608,7.74761716210148,
7.84478550698122,7.95299010726183,8.09543431525411,8.29292072871432,8.37862309065676,
8.48559834856376,8.6253332273617,8.80539149015593,8.8980055317184,9.07507730815184,
9.23653588492767,9.42891091322493,9.53717879929051,9.67641954779035,9.85634273166462,
9.94846876501138,10.124371807052,10.2862506150661,10.4786886768751,10.585108936019,
10.7250936259518,10.9209686902655,11.0051861291791,11.0413371089366),
 .UNSPECIFIED.);
#131=B_SPLINE_CURVE_WITH_KNOTS('',3,(#9150,#9151,#9152,#9153,#9154,#9155,
#9156,#9157,#9158,#9159,#9160,#9161,#9162,#9163,#9164,#9165,#9166,#9167,
#9168,#9169,#9170,#9171,#9172,#9173,#9174,#9175,#9176,#9177,#9178,#9179,
#9180,#9181,#9182,#9183,#9184,#9185,#9186,#9187,#9188,#9189,#9190,#9191,
#9192,#9193,#9194,#9195,#9196,#9197,#9198,#9199,#9200,#9201,#9202,#9203,
#9204,#9205,#9206,#9207,#9208,#9209,#9210,#9211,#9212,#9213,#9214,#9215,
#9216,#9217,#9218,#9219,#9220,#9221,#9222,#9223,#9224,#9225,#9226,#9227,
#9228,#9229,#9230,#9231,#9232,#9233,#9234,#9235,#9236,#9237,#9238,#9239,
#9240,#9241,#9242,#9243,#9244,#9245,#9246,#9247,#9248,#9249,#9250,#9251),
 .UNSPECIFIED.,.F.,.F.,(4,2,2,2,2,2,2,2,2,2,2,2,2,2,2,2,2,2,2,2,2,2,2,2,
2,2,2,2,2,2,2,2,2,2,2,2,2,2,2,2,2,2,2,2,2,2,2,2,2,2,4),(6.23335612761586,
6.2680726661503,6.44942264436023,6.60915211923207,6.76136559666284,6.84923300983916,
6.95045580235986,7.11269571489834,7.25090846445631,7.36192407750934,7.44688581082496,
7.64297223261621,7.78383654572914,7.88624389570455,7.97052662126554,8.16631202122395,
8.30633596179256,8.41253308698677,8.4983811778714,8.69627543731715,8.83915310298785,
8.94644447739489,9.04402311820006,9.21031149618558,9.34765752913951,9.46120630502673,
9.54583931617467,9.74166539339258,9.8820615547246,9.9945325293888,10.0897943123272,
10.2615588379134,10.399560401475,10.5111028004756,10.5959745858038,10.7919542465067,
10.9326770564329,11.0353378666286,11.2280111432196,11.3887279582758,11.5692870436916,
11.6648159305064,11.8359091402827,11.9738179216995,12.0855833718003,12.1704159141617,
12.3663497119896,12.5070126022303,12.6105784668576,12.695645656318,12.8422919822627),
 .UNSPECIFIED.);
#132=B_SPLINE_CURVE_WITH_KNOTS('',3,(#9252,#9253,#9254,#9255,#9256,#9257,
#9258,#9259,#9260,#9261,#9262,#9263,#9264,#9265,#9266,#9267,#9268,#9269,
#9270,#9271,#9272,#9273,#9274,#9275,#9276,#9277,#9278,#9279,#9280,#9281,
#9282,#9283,#9284,#9285,#9286,#9287,#9288,#9289,#9290,#9291,#9292,#9293,
#9294,#9295,#9296,#9297,#9298,#9299,#9300,#9301,#9302,#9303,#9304,#9305,
#9306,#9307,#9308,#9309,#9310,#9311,#9312,#9313,#9314,#9315,#9316,#9317,
#9318,#9319,#9320,#9321,#9322,#9323,#9324,#9325,#9326,#9327,#9328,#9329,
#9330,#9331,#9332,#9333,#9334,#9335,#9336,#9337,#9338,#9339,#9340,#9341,
#9342,#9343,#9344,#9345,#9346,#9347),.UNSPECIFIED.,.F.,.F.,(4,2,2,2,2,2,
2,2,2,2,2,2,2,2,2,2,2,2,2,2,2,2,2,2,2,2,2,2,2,2,2,2,2,2,2,2,2,2,2,2,2,2,
2,2,2,2,2,4),(11.0413371089366,11.1079687724179,11.2487172487334,11.4447819529984,
11.5296659966344,11.6414732350562,11.7794588126016,11.9506203229406,12.0462296440394,
12.226700548978,12.3876027102809,12.5801555071267,12.6942822091242,12.8315199327858,
12.9987910833866,13.0956430068284,13.2046843234955,13.3467852356924,13.5439569316993,
13.6295371093675,13.7372405177515,13.8767441274198,14.0567961574491,14.1491616376219,
14.3256279190537,14.4873651427831,14.6798877932856,14.787419457666,14.9270028333426,
15.1070873787722,15.1995282230915,15.3761715394229,15.5378626266959,15.7303489097924,
15.8379211901484,15.9775009910812,16.1575942573031,16.2500284409572,16.4266528536513,
16.5883656734284,16.7808760392524,16.8884584809964,17.0280466873063,17.2081519258478,
17.3005913133539,17.4772251458276,17.6389498989778,17.6543409950681),
 .UNSPECIFIED.);
#133=B_SPLINE_CURVE_WITH_KNOTS('',3,(#9353,#9354,#9355,#9356,#9357,#9358),
 .UNSPECIFIED.,.F.,.F.,(4,2,4),(12.8423781512227,12.9895144519815,13.2181607322366),
 .UNSPECIFIED.);
#134=B_SPLINE_CURVE_WITH_KNOTS('',3,(#9359,#9360,#9361,#9362,#9363,#9364,
#9365,#9366,#9367,#9368,#9369,#9370,#9371,#9372,#9373,#9374,#9375,#9376,
#9377,#9378,#9379,#9380,#9381,#9382,#9383,#9384,#9385,#9386,#9387,#9388,
#9389,#9390,#9391,#9392,#9393,#9394,#9395,#9396,#9397,#9398,#9399,#9400,
#9401,#9402,#9403,#9404,#9405,#9406,#9407,#9408,#9409,#9410,#9411,#9412,
#9413,#9414,#9415,#9416,#9417,#9418,#9419,#9420,#9421,#9422,#9423,#9424,
#9425,#9426,#9427,#9428,#9429,#9430,#9431,#9432,#9433,#9434,#9435,#9436,
#9437,#9438,#9439,#9440,#9441,#9442,#9443,#9444,#9445,#9446,#9447,#9448),
 .UNSPECIFIED.,.F.,.F.,(4,2,2,2,2,2,2,2,2,2,2,2,2,2,2,2,2,2,2,2,2,2,2,2,
2,2,2,2,2,2,2,2,2,2,2,2,2,2,2,2,2,2,2,2,4),(0.000192812523341109,0.227830918649042,
0.402695824517761,0.495345820468585,0.605011255121174,0.745682846989847,
0.941635256368896,1.02647350321401,1.13818028830822,1.27609592000783,1.44708043233579,
1.54269318764458,1.72249229572632,1.88359776728222,2.07669827020567,2.17942746011534,
2.32010735870701,2.51607560838843,2.60091849941476,2.71266275449528,2.8505826010169,
3.02164223123286,3.11721781087632,3.29748494778651,3.45836804138001,3.65087443006171,
3.76478362635717,3.90200434301853,4.06891694069374,4.16595768138673,4.27438799083112,
4.416686309398,4.61401881184024,4.69966105666755,4.80681895602313,4.94644760489433,
5.12645933890658,5.21897313800511,5.39581519676004,5.55731223059382,5.74983419995918,
5.85878400080293,5.99773397831681,6.17448435879023,6.23335612761586),
 .UNSPECIFIED.);
#135=B_SPLINE_CURVE_WITH_KNOTS('',3,(#9449,#9450,#9451,#9452,#9453,#9454,
#9455,#9456,#9457,#9458,#9459,#9460,#9461,#9462,#9463,#9464,#9465,#9466,
#9467,#9468,#9469,#9470,#9471,#9472,#9473,#9474,#9475,#9476,#9477,#9478,
#9479,#9480,#9481,#9482,#9483,#9484,#9485,#9486,#9487,#9488,#9489,#9490,
#9491,#9492,#9493,#9494,#9495,#9496,#9497,#9498,#9499,#9500,#9501,#9502,
#9503,#9504,#9505,#9506,#9507,#9508,#9509,#9510,#9511,#9512,#9513,#9514,
#9515,#9516,#9517,#9518,#9519,#9520,#9521,#9522,#9523,#9524,#9525,#9526,
#9527,#9528,#9529,#9530,#9531,#9532,#9533,#9534,#9535,#9536,#9537,#9538,
#9539,#9540,#9541,#9542,#9543,#9544),.UNSPECIFIED.,.F.,.F.,(4,2,2,2,2,2,
2,2,2,2,2,2,2,2,2,2,2,2,2,2,2,2,2,2,2,2,2,2,2,2,2,2,2,2,2,2,2,2,2,2,2,2,
2,2,2,2,2,4),(17.6543409950681,17.831448232565,17.9388970388975,18.078550307813,
18.2580275286684,18.3509018576439,18.5285655816919,18.6899522360199,18.883317496408,
18.9859410358361,19.1268498083911,19.3230657959226,19.4080515417586,19.5194700182778,
19.6576752470134,19.8301085240745,19.925273452302,20.0382668814786,20.1785995356747,
20.3745754313835,20.4591193113276,20.560959448406,20.7022315358752,20.8987111478103,
20.9839122498395,21.0939464152428,21.2326549062009,21.4123366353141,21.5039831339058,
21.6859652182246,21.8449450631771,22.0389207324904,22.1618875308622,22.352077762761,
22.492416404637,22.6054578212541,22.7006149626931,22.8731170251549,23.0113543915084,
23.1227549816257,23.2077525682346,23.4039738361564,23.5449009423806,23.6475443397645,
23.8402633557091,24.0010308597138,24.1820036907275,24.2697619665442),
 .UNSPECIFIED.);
#136=B_SPLINE_CURVE_WITH_KNOTS('',3,(#9549,#9550,#9551,#9552,#9553,#9554,
#9555,#9556,#9557,#9558,#9559,#9560,#9561,#9562,#9563,#9564,#9565,#9566,
#9567,#9568,#9569,#9570,#9571,#9572,#9573,#9574,#9575,#9576,#9577,#9578,
#9579,#9580,#9581,#9582,#9583,#9584,#9585,#9586,#9587,#9588,#9589,#9590,
#9591,#9592,#9593,#9594,#9595,#9596,#9597,#9598,#9599,#9600,#9601,#9602,
#9603,#9604,#9605,#9606,#9607,#9608,#9609,#9610,#9611,#9612,#9613,#9614,
#9615,#9616,#9617,#9618,#9619,#9620,#9621,#9622,#9623,#9624,#9625,#9626,
#9627,#9628,#9629,#9630,#9631,#9632,#9633,#9634,#9635,#9636,#9637,#9638,
#9639,#9640,#9641,#9642,#9643,#9644,#9645,#9646,#9647,#9648,#9649,#9650),
 .UNSPECIFIED.,.F.,.F.,(4,2,2,2,2,2,2,2,2,2,2,2,2,2,2,2,2,2,2,2,2,2,2,2,
2,2,2,2,2,2,2,2,2,2,2,2,2,2,2,2,2,2,2,2,2,2,2,2,2,2,4),(6.23337760445098,
6.26077836375648,6.36024771798476,6.46448343304622,6.60906386766685,6.78456179187364,
6.93662045763576,7.1323810286063,7.30321529556475,7.45656361674879,7.53958466179243,
7.73647663198394,7.87584064015966,7.98371163899557,8.06920767247095,8.2661630472445,
8.40808467559384,8.51733631274462,8.61403729468532,8.78135200164673,8.91851068914279,
9.03266254477226,9.11723416458245,9.3130398364756,9.45336262315145,9.56600363361281,
9.66119059252339,9.83316651194362,9.97120439935581,10.0826538815603,10.1675408239304,
10.3635373773577,10.5042835130592,10.6069015054932,10.7997225471817,10.9605892203953,
11.1408781760215,11.2364444175853,11.4074977978003,11.545416911005,11.6571650160255,
11.742002359112,11.9379433516568,12.0786137180603,12.1827271699913,12.2684323702091,
12.4659165898637,12.6083986443827,12.7163747934482,12.813552790721,12.8423781512227),
 .UNSPECIFIED.);
#137=B_SPLINE_CURVE_WITH_KNOTS('',3,(#9651,#9652,#9653,#9654,#9655,#9656,
#9657,#9658,#9659,#9660,#9661,#9662,#9663,#9664,#9665,#9666,#9667,#9668,
#9669,#9670,#9671,#9672,#9673,#9674,#9675,#9676,#9677,#9678,#9679,#9680,
#9681,#9682,#9683,#9684,#9685,#9686,#9687,#9688,#9689,#9690,#9691,#9692,
#9693,#9694,#9695,#9696,#9697,#9698,#9699,#9700,#9701,#9702,#9703,#9704,
#9705,#9706,#9707,#9708,#9709,#9710,#9711,#9712,#9713,#9714,#9715,#9716,
#9717,#9718,#9719,#9720,#9721,#9722,#9723,#9724,#9725,#9726,#9727,#9728,
#9729,#9730,#9731,#9732,#9733,#9734,#9735,#9736,#9737,#9738,#9739,#9740,
#9741,#9742,#9743,#9744,#9745,#9746,#9747,#9748,#9749,#9750),
 .UNSPECIFIED.,.F.,.F.,(4,2,2,2,2,2,2,2,2,2,2,2,2,2,2,2,2,2,2,2,2,2,2,2,
2,2,2,2,2,2,2,2,2,2,2,2,2,2,2,2,2,2,2,2,2,2,2,2,2,4),(24.2697619665442,
24.2775981868636,24.4489178802201,24.5869659818761,24.6988703740305,24.7837903210938,
24.9799298746111,25.1207383490778,25.2327027835779,25.3283426169409,25.4995888239524,
25.6376391981639,25.7495081133103,25.8344271986969,26.0305591071743,26.1713654429127,
26.2755865933713,26.3613764208643,26.5590561568995,26.7016799031348,26.8097776151025,
26.907082060738,27.0739033264763,27.2112791614196,27.325154142349,27.5182505086529,
27.6797073494656,27.8571147537519,27.9498752178987,28.1297026103414,28.269443400461,
28.376645608559,28.4623502090655,28.6598040912766,28.8022060851135,28.9107074268383,
29.0078121207644,29.1748316803279,29.3121502107654,29.4261396767462,29.6186715357246,
29.7795702717774,29.9601421331204,30.0557572846878,30.2269559593022,30.3649693430795,
30.4768074783437,30.5617037610844,30.7577828820173,30.8837752445267),
 .UNSPECIFIED.);
#138=B_SPLINE_CURVE_WITH_KNOTS('',3,(#9756,#9757,#9758,#9759,#9760,#9761,
#9762,#9763,#9764,#9765,#9766,#9767,#9768,#9769,#9770,#9771),
 .UNSPECIFIED.,.F.,.F.,(4,3,3,3,3,4),(39.0083726877398,39.080749342486,
39.1531225734978,39.2254897186212,39.2978686649688,39.3655358516619),
 .UNSPECIFIED.);
#139=B_SPLINE_CURVE_WITH_KNOTS('',3,(#9772,#9773,#9774,#9775,#9776,#9777,
#9778,#9779,#9780,#9781,#9782,#9783,#9784,#9785,#9786,#9787,#9788,#9789,
#9790,#9791,#9792,#9793,#9794,#9795,#9796,#9797,#9798,#9799,#9800,#9801,
#9802,#9803,#9804,#9805,#9806,#9807,#9808,#9809,#9810,#9811,#9812,#9813,
#9814,#9815,#9816,#9817,#9818,#9819,#9820,#9821,#9822,#9823,#9824,#9825,
#9826,#9827,#9828,#9829,#9830,#9831,#9832,#9833,#9834,#9835,#9836,#9837,
#9838,#9839,#9840,#9841,#9842,#9843,#9844,#9845,#9846,#9847,#9848,#9849,
#9850,#9851,#9852,#9853,#9854,#9855,#9856,#9857,#9858,#9859,#9860,#9861),
 .UNSPECIFIED.,.F.,.F.,(4,2,2,2,2,2,2,2,2,2,2,2,2,2,2,2,2,2,2,2,2,2,2,2,
2,2,2,2,2,2,2,2,2,2,2,2,2,2,2,2,2,2,2,2,4),(0.000167115010632562,0.089463628004945,
0.250033227595873,0.40679334364094,0.599455029928833,0.709557528655732,
0.847466881949497,1.01852676597952,1.11408252919257,1.29448763332879,1.45527420990791,
1.64770353594286,1.76183295060474,1.89896780692874,2.06626165489344,2.16295304662853,
2.27218807214103,2.41408405866917,2.61102554534045,2.69650541653858,2.80439100592715,
2.94371708965856,3.12363136335108,3.21585090273878,3.39199485037615,3.55371328896186,
3.74598316810651,3.85235900021351,3.9922991398571,4.18810604298212,4.27229888220503,
4.37502957916033,4.51573723764941,4.71173916253334,4.79659919197649,4.90832981096552,
5.04628129377324,5.21729951277161,5.31294329014396,5.49270605398742,5.65389454952269,
5.84654957518262,5.95881353677797,6.09659716585997,6.23337760445098),
 .UNSPECIFIED.);
#140=B_SPLINE_CURVE_WITH_KNOTS('',3,(#9862,#9863,#9864,#9865,#9866,#9867,
#9868,#9869,#9870,#9871,#9872,#9873,#9874,#9875,#9876,#9877,#9878,#9879,
#9880,#9881,#9882,#9883,#9884,#9885,#9886,#9887,#9888,#9889,#9890,#9891,
#9892,#9893,#9894,#9895,#9896,#9897,#9898,#9899,#9900,#9901,#9902,#9903,
#9904,#9905,#9906,#9907,#9908,#9909,#9910,#9911,#9912,#9913,#9914,#9915,
#9916,#9917,#9918,#9919,#9920,#9921,#9922,#9923,#9924,#9925,#9926,#9927,
#9928,#9929,#9930,#9931,#9932,#9933,#9934,#9935,#9936,#9937,#9938,#9939,
#9940,#9941,#9942,#9943,#9944,#9945,#9946,#9947,#9948,#9949,#9950,#9951,
#9952,#9953,#9954,#9955,#9956,#9957,#9958,#9959,#9960,#9961,#9962,#9963),
 .UNSPECIFIED.,.F.,.F.,(4,2,2,2,2,2,2,2,2,2,2,2,2,2,2,2,2,2,2,2,2,2,2,2,
2,2,2,2,2,2,2,2,2,2,2,2,2,2,2,2,2,2,2,2,2,2,2,2,2,2,4),(30.8837752445267,
30.8985513929829,31.0027440740847,31.0885107450702,31.286137105715,31.4287223138741,
31.5367910962938,31.6340692241231,31.8008456401066,31.9381844314296,32.0520287869352,
32.2444973830893,32.4053508658922,32.5859358628873,32.6815315693023,32.8527112874765,
32.9907030816835,33.102527544385,33.1874107771474,33.3834603362991,33.5242072801014,
33.6283862497612,33.7141403102153,33.9117376999498,34.0543021429303,34.1623538351394,
34.2596179149756,34.4263689485974,34.5636873656241,34.6775144495382,34.7621518063255,
34.9580361662437,35.0984506837668,35.2110292174805,35.3062933455278,35.4782022778076,
35.6162659000383,35.7278089514407,35.8127161027665,36.0087700324591,36.1495508876168,
36.2522288887509,36.3364601035755,36.5322938606012,36.6722842831347,36.7786588078875,
36.9711336332874,37.1330696108447,37.3087527931773,37.4007818445533,37.4953062588109),
 .UNSPECIFIED.);
#141=B_SPLINE_CURVE_WITH_KNOTS('',3,(#9966,#9967,#9968,#9969,#9970,#9971,
#9972,#9973,#9974,#9975,#9976,#9977,#9978,#9979,#9980,#9981,#9982,#9983,
#9984,#9985,#9986,#9987,#9988,#9989,#9990,#9991,#9992,#9993,#9994,#9995,
#9996,#9997,#9998,#9999,#10000,#10001,#10002,#10003,#10004,#10005,#10006,
#10007,#10008,#10009,#10010,#10011,#10012,#10013,#10014,#10015,#10016,#10017,
#10018,#10019,#10020,#10021,#10022,#10023,#10024,#10025,#10026,#10027,#10028,
#10029,#10030,#10031,#10032,#10033,#10034,#10035,#10036,#10037,#10038,#10039,
#10040,#10041,#10042,#10043,#10044,#10045,#10046,#10047,#10048,#10049,#10050,
#10051,#10052,#10053,#10054,#10055,#10056,#10057,#10058,#10059,#10060,#10061),
 .UNSPECIFIED.,.F.,.F.,(4,2,2,2,2,2,2,2,2,2,2,2,2,2,2,2,2,2,2,2,2,2,2,2,
2,2,2,2,2,2,2,2,2,2,2,2,2,2,2,2,2,2,2,2,2,2,2,4),(37.4953062588109,37.580624778732,
37.7197557646577,37.8282792076654,37.9136581049212,38.1103703089893,38.2520187572005,
38.3618986649034,38.4583721738345,38.6259798462175,38.7631013939321,38.877424770735,
39.0700022564623,39.230922664749,39.4111958169609,39.506781849307,39.6778619379215,
39.8158050480093,39.9275760812986,40.0124351730281,40.2084252844014,40.3491389033369,
40.4518678475122,40.5360457888487,40.7318229906229,40.8717348049317,40.9781885420517,
41.1704701195794,41.332243773217,41.5082714258425,41.6004220997857,41.7802696498608,
41.9194967324815,42.0276105701555,42.220272096058,42.3820437005206,42.5580485181999,
42.6503136546282,42.8302519341941,42.9696994200002,43.0771426351419,43.2692475698609,
43.4296997938774,43.6106309098647,43.7071358476977,43.7706118235221,43.9091487174759,
44.0778884690173),.UNSPECIFIED.);
#142=B_SPLINE_CURVE_WITH_KNOTS('',3,(#10064,#10065,#10066,#10067,#10068,
#10069,#10070,#10071,#10072,#10073,#10074,#10075,#10076,#10077,#10078,#10079,
#10080,#10081,#10082,#10083,#10084,#10085,#10086,#10087,#10088,#10089,#10090,
#10091,#10092,#10093,#10094,#10095,#10096,#10097,#10098,#10099,#10100,#10101,
#10102,#10103,#10104,#10105,#10106,#10107,#10108,#10109,#10110,#10111,#10112,
#10113,#10114,#10115,#10116,#10117,#10118,#10119,#10120,#10121,#10122,#10123,
#10124,#10125,#10126,#10127,#10128,#10129,#10130,#10131,#10132,#10133,#10134,
#10135,#10136,#10137,#10138,#10139,#10140,#10141,#10142,#10143,#10144,#10145,
#10146,#10147,#10148,#10149,#10150,#10151,#10152,#10153,#10154,#10155,#10156,
#10157,#10158,#10159,#10160,#10161,#10162,#10163,#10164,#10165,#10166,#10167,
#10168,#10169,#10170,#10171,#10172,#10173,#10174,#10175,#10176,#10177,#10178,
#10179,#10180,#10181,#10182,#10183,#10184,#10185,#10186,#10187,#10188,#10189,
#10190,#10191,#10192,#10193,#10194,#10195,#10196,#10197,#10198,#10199,#10200,
#10201,#10202,#10203,#10204,#10205,#10206,#10207,#10208,#10209,#10210,#10211,
#10212,#10213,#10214,#10215,#10216,#10217,#10218,#10219,#10220,#10221,#10222,
#10223,#10224,#10225,#10226,#10227,#10228,#10229,#10230,#10231,#10232,#10233,
#10234,#10235,#10236,#10237,#10238,#10239,#10240,#10241,#10242,#10243,#10244,
#10245,#10246,#10247,#10248,#10249,#10250,#10251,#10252,#10253,#10254,#10255,
#10256),.UNSPECIFIED.,.F.,.F.,(4,3,3,3,3,3,3,3,3,3,3,3,3,3,3,3,3,3,3,3,
3,3,3,3,3,3,3,3,3,3,3,3,3,3,3,3,3,3,3,3,3,3,3,3,3,3,3,3,3,3,3,3,3,3,3,3,
3,3,3,3,3,3,3,3,4),(39.3655358516619,39.4205489266629,39.4932256719064,
39.5658896866156,39.6385455807481,39.7112072104722,39.7838675238176,39.856544881781,
39.9195432168738,39.9922242628658,40.0648925892348,40.1375527937686,40.2102187009694,
40.2828832672999,40.3555648079552,40.4185375070847,40.4912126225807,40.5638750101892,
40.6365292843827,40.7091893168006,40.7818480476756,40.8545238586228,40.9175317972957,
40.9902104856699,41.062876431308,41.1355342389029,41.2081977415302,41.2808599026547,
41.353539054321,41.4165260875066,41.4892161017965,41.561893459126,41.6345627313084,
41.7072376971512,41.7799113036542,41.8526017895959,41.9155203777175,41.988155950647,
42.0607786263891,42.1333931314236,42.2060135911872,42.2786329155975,42.3512698720499,
42.4145146679284,42.48729869792,42.5600703328061,42.632833872698,42.7056024032701,
42.7783690429378,42.8511510266575,42.9135089581394,42.9859787125309,43.0584354826672,
43.1308844455598,43.2033410888313,43.275797773863,43.3482751674385,43.4125032483503,
43.4856192267066,43.5587218933442,43.6318145250677,43.7049066040599,43.7779931512484,
43.8510867420094,43.9114975385612),.UNSPECIFIED.);
#143=B_SPLINE_CURVE_WITH_KNOTS('',3,(#10259,#10260,#10261,#10262,#10263,
#10264,#10265,#10266,#10267,#10268,#10269,#10270,#10271,#10272,#10273,#10274,
#10275,#10276,#10277,#10278,#10279,#10280,#10281,#10282,#10283,#10284,#10285,
#10286,#10287,#10288,#10289,#10290,#10291,#10292,#10293,#10294,#10295,#10296,
#10297,#10298,#10299,#10300,#10301,#10302,#10303,#10304,#10305,#10306,#10307,
#10308,#10309,#10310,#10311,#10312,#10313,#10314,#10315,#10316,#10317,#10318,
#10319,#10320,#10321,#10322,#10323,#10324,#10325,#10326,#10327,#10328,#10329,
#10330,#10331,#10332,#10333,#10334),.UNSPECIFIED.,.F.,.F.,(4,3,3,3,3,3,
3,3,3,3,3,3,3,3,3,3,3,3,3,3,3,3,3,3,3,4),(51.7052219494017,51.7752622461825,
51.8232741926851,51.8933148183004,51.9633435475172,52.0333645023577,52.1055904974923,
52.1756151937478,52.2489418383219,52.322268482896,52.3923090961645,52.4623378133711,
52.5323587565658,52.6045847607011,52.674609446344,52.7479361097254,52.8212627731069,
52.8913031445529,52.961331618526,53.0313523177225,53.1035785041213,53.1736029469128,
53.2469300051154,53.3202570633179,53.3951479415614,53.4070751110265),
 .UNSPECIFIED.);
#144=B_SPLINE_CURVE_WITH_KNOTS('',3,(#10336,#10337,#10338,#10339,#10340,
#10341,#10342,#10343,#10344),.UNSPECIFIED.,.F.,.F.,(4,1,1,1,1,1,4),(53.4070751344278,
53.8192513535288,54.3182456437397,54.8172399339506,55.3162342241615,55.8152285143725,
56.2866044747298),.UNSPECIFIED.);
#145=B_SPLINE_CURVE_WITH_KNOTS('',3,(#10348,#10349,#10350,#10351,#10352,
#10353,#10354,#10355),.UNSPECIFIED.,.F.,.F.,(4,1,1,1,1,4),(53.4070751110265,
53.7675563424624,54.2665506326734,54.7655449228843,55.2645392130952,55.7635335033061),
 .UNSPECIFIED.);
#146=B_SPLINE_CURVE_WITH_KNOTS('',3,(#10356,#10357,#10358,#10359,#10360,
#10361,#10362,#10363,#10364,#10365,#10366,#10367,#10368,#10369,#10370,#10371,
#10372,#10373,#10374,#10375,#10376,#10377,#10378,#10379,#10380,#10381,#10382,
#10383,#10384,#10385,#10386,#10387,#10388,#10389,#10390,#10391,#10392,#10393,
#10394,#10395,#10396,#10397,#10398,#10399,#10400,#10401,#10402,#10403,#10404,
#10405,#10406,#10407,#10408,#10409,#10410,#10411,#10412,#10413,#10414,#10415,
#10416,#10417,#10418,#10419,#10420,#10421,#10422,#10423,#10424,#10425,#10426,
#10427,#10428),.UNSPECIFIED.,.F.,.F.,(4,3,3,3,3,3,3,3,3,3,3,3,3,3,3,3,3,
3,3,3,3,3,3,3,4),(51.705223688797,51.7715791816187,51.8416224003585,51.9116537285312,
51.9816772813509,52.0539013289706,52.1239285887193,52.1972510302745,52.2705734718297,
52.3406109642765,52.4106365581925,52.4806543837547,52.5528827283262,52.6229043486391,
52.6962360553399,52.7695677620406,52.8396086885631,52.9096377028379,52.9796589263131,
53.0518847077977,53.1219096292928,53.1952358407721,53.2685620522515,53.3417764954199,
53.4070751084796),.UNSPECIFIED.);
#147=B_SPLINE_CURVE_WITH_KNOTS('',3,(#10794,#10795,#10796,#10797,#10798,
#10799,#10800,#10801,#10802,#10803,#10804,#10805,#10806,#10807,#10808,#10809,
#10810,#10811,#10812,#10813,#10814,#10815,#10816,#10817,#10818,#10819,#10820,
#10821,#10822,#10823,#10824,#10825,#10826,#10827,#10828,#10829,#10830,#10831,
#10832,#10833,#10834,#10835,#10836,#10837,#10838,#10839,#10840,#10841,#10842,
#10843,#10844,#10845,#10846,#10847,#10848,#10849,#10850,#10851,#10852,#10853,
#10854,#10855,#10856,#10857,#10858,#10859,#10860,#10861,#10862,#10863,#10864,
#10865,#10866,#10867,#10868,#10869,#10870,#10871,#10872,#10873,#10874,#10875,
#10876,#10877,#10878,#10879,#10880,#10881,#10882,#10883,#10884,#10885,#10886,
#10887,#10888,#10889,#10890,#10891,#10892,#10893,#10894,#10895,#10896,#10897,
#10898,#10899,#10900,#10901,#10902,#10903,#10904,#10905,#10906,#10907,#10908,
#10909,#10910,#10911,#10912,#10913,#10914),.UNSPECIFIED.,.F.,.F.,(4,3,3,
3,3,3,3,3,3,3,3,3,3,3,3,3,3,3,3,3,3,3,3,3,3,3,3,3,3,3,3,3,3,3,3,3,3,3,3,
3,4),(0.,0.0847077516937711,0.170225033889545,0.255907500532044,0.341119279232027,
0.425059357774081,0.455383656591401,0.465770691009882,0.474513364932373,
0.558298342951859,0.600642802906426,0.684662560232661,0.768686524706548,
0.851862297329437,0.912900878915177,0.924214418880625,0.933065505594978,
1.0153136859126,1.09836343076414,1.18141317561567,1.26373325194697,1.34541324334634,
1.36175593088453,1.37449997082537,1.4548533829364,1.53535345080198,1.61538859658373,
1.69412331509383,1.74187144182578,1.78111905912933,1.79651186345433,1.80847555043388,
1.88768501687034,1.96689410707861,2.04543359504746,2.05585238025418,2.07005430121714,
2.14795915943215,2.2248426348574,2.28089532743822,2.31010750305873),
 .UNSPECIFIED.);
#148=B_SPLINE_CURVE_WITH_KNOTS('',3,(#10915,#10916,#10917,#10918),
 .UNSPECIFIED.,.F.,.F.,(4,4),(-0.00101472999876572,0.),.UNSPECIFIED.);
#149=B_SPLINE_CURVE_WITH_KNOTS('',3,(#10919,#10920,#10921,#10922,#10923,
#10924,#10925,#10926,#10927,#10928,#10929,#10930,#10931,#10932,#10933,#10934,
#10935,#10936,#10937,#10938,#10939,#10940,#10941,#10942,#10943,#10944,#10945,
#10946,#10947,#10948,#10949,#10950,#10951,#10952,#10953,#10954,#10955,#10956,
#10957,#10958,#10959,#10960,#10961,#10962,#10963,#10964,#10965,#10966,#10967,
#10968,#10969,#10970,#10971,#10972,#10973,#10974,#10975,#10976,#10977,#10978,
#10979,#10980,#10981,#10982,#10983,#10984,#10985,#10986,#10987,#10988,#10989,
#10990,#10991,#10992,#10993,#10994,#10995,#10996,#10997,#10998,#10999,#11000,
#11001,#11002,#11003,#11004,#11005,#11006,#11007,#11008,#11009,#11010,#11011,
#11012,#11013,#11014,#11015,#11016,#11017,#11018,#11019,#11020,#11021,#11022,
#11023,#11024,#11025,#11026,#11027,#11028,#11029,#11030,#11031,#11032,#11033),
 .UNSPECIFIED.,.F.,.F.,(4,3,3,3,3,3,3,3,3,3,3,3,3,3,3,3,3,3,3,3,3,3,3,3,
3,3,3,3,3,3,3,3,3,3,3,3,3,3,4),(0.,0.0756021000860911,0.152393199558973,
0.230392842176159,0.308644925471132,0.386546669685798,0.408880923643587,
0.422045036140801,0.501691131550158,0.537249170842264,0.616137946028816,
0.695699298379207,0.775607582769941,0.834608203354004,0.843321085046558,
0.924172696188028,1.0095507158666,1.09492873554517,1.18019567138666,1.26546260722815,
1.27900992162839,1.28771744272705,1.36946368552726,1.45259721935328,1.53602421303373,
1.61905253984022,1.6726411664557,1.7128618032572,1.72976589348117,1.74248623587577,
1.82597852344175,1.91057121436523,1.99440626086767,2.0125183165509,2.02643670802463,
2.1120758801977,2.19783429697825,2.26933164573093,2.30291422475425),
 .UNSPECIFIED.);
#150=B_SPLINE_CURVE_WITH_KNOTS('',3,(#11398,#11399,#11400,#11401,#11402,
#11403,#11404,#11405,#11406,#11407,#11408,#11409,#11410,#11411,#11412,#11413,
#11414,#11415,#11416,#11417,#11418,#11419,#11420,#11421,#11422,#11423,#11424,
#11425,#11426,#11427,#11428,#11429,#11430,#11431,#11432,#11433,#11434,#11435,
#11436,#11437,#11438,#11439,#11440,#11441,#11442,#11443,#11444,#11445,#11446,
#11447,#11448,#11449,#11450,#11451,#11452,#11453,#11454,#11455,#11456,#11457,
#11458,#11459,#11460,#11461,#11462,#11463,#11464,#11465,#11466,#11467,#11468,
#11469,#11470,#11471,#11472,#11473,#11474,#11475,#11476,#11477,#11478,#11479,
#11480,#11481,#11482,#11483,#11484,#11485,#11486,#11487,#11488,#11489,#11490,
#11491,#11492,#11493,#11494,#11495,#11496,#11497,#11498,#11499,#11500,#11501,
#11502,#11503,#11504,#11505,#11506,#11507,#11508,#11509,#11510,#11511,#11512),
 .UNSPECIFIED.,.F.,.F.,(4,3,3,3,3,3,3,3,3,3,3,3,3,3,3,3,3,3,3,3,3,3,3,3,
3,3,3,3,3,3,3,3,3,3,3,3,3,3,4),(0.,0.0756020442574116,0.152393096832318,
0.230392716296112,0.308644793984952,0.386546557639097,0.408880856230141,
0.420928744427606,0.500569899331183,0.537249170842273,0.616073663427341,
0.695678467211851,0.775598186338839,0.815514504989629,0.834608290416057,
0.84847123329491,0.929373466901696,1.01215110122343,1.09492873554516,1.17606648597094,
1.25762667195969,1.27900990554167,1.28771743639829,1.3694636568822,1.45259718089028,
1.53602417080081,1.61905249837216,1.6726411664557,1.73231431654345,1.74174492869213,
1.82529436366379,1.90959642814042,1.99435898918172,2.01251832412271,2.02375496071478,
2.10938057767906,2.19514471614932,2.26933164573094,2.30291844692703),
 .UNSPECIFIED.);
#151=B_SPLINE_CURVE_WITH_KNOTS('',3,(#11513,#11514,#11515,#11516,#11517,
#11518,#11519,#11520,#11521,#11522,#11523,#11524,#11525,#11526,#11527,#11528,
#11529,#11530,#11531,#11532,#11533,#11534,#11535,#11536,#11537,#11538,#11539,
#11540,#11541,#11542,#11543,#11544,#11545,#11546,#11547,#11548,#11549,#11550,
#11551,#11552,#11553,#11554,#11555,#11556,#11557,#11558,#11559,#11560,#11561,
#11562,#11563,#11564,#11565,#11566,#11567,#11568,#11569,#11570,#11571,#11572,
#11573,#11574,#11575,#11576,#11577,#11578,#11579,#11580,#11581,#11582,#11583,
#11584,#11585,#11586,#11587,#11588,#11589,#11590,#11591,#11592,#11593,#11594,
#11595,#11596,#11597,#11598,#11599,#11600,#11601,#11602,#11603,#11604,#11605,
#11606,#11607,#11608,#11609,#11610,#11611,#11612,#11613,#11614,#11615,#11616,
#11617,#11618,#11619,#11620,#11621,#11622,#11623,#11624,#11625,#11626,#11627,
#11628,#11629,#11630,#11631,#11632,#11633,#11634,#11635,#11636),
 .UNSPECIFIED.,.F.,.F.,(4,3,3,3,3,3,3,3,3,3,3,3,3,3,3,3,3,3,3,3,3,3,3,3,
3,3,3,3,3,3,3,3,3,3,3,3,3,3,3,3,3,4),(6.61845341725208E-15,0.0849506171234816,
0.170583039076072,0.256324783691451,0.342404288495193,0.406963917098,0.455383638550105,
0.468536166046617,0.479421865514442,0.56319740127756,0.600642802906421,
0.684641773439832,0.768646494244517,0.852075754152883,0.893242931835729,
0.912628999565668,0.923529204327917,0.932945920282414,0.963808297499684,
1.04604185844047,1.12763182145717,1.18141317561565,1.26548811560765,1.34956305559966,
1.36175593015859,1.37449997074551,1.45485337915238,1.53535344652152,1.61538859015649,
1.6941233006684,1.74187144182573,1.79625541798791,1.80632110746682,1.88551239813008,
1.96470047939158,2.04374919140323,2.05752087865608,2.0731251477082,2.15101429053224,
2.22787487765179,2.28089532743819,2.31010750305869),.UNSPECIFIED.);
#152=B_SPLINE_CURVE_WITH_KNOTS('',3,(#11681,#11682,#11683,#11684,#11685,
#11686,#11687,#11688,#11689,#11690,#11691,#11692,#11693,#11694,#11695,#11696,
#11697,#11698,#11699,#11700,#11701,#11702,#11703,#11704,#11705,#11706,#11707,
#11708,#11709,#11710,#11711,#11712,#11713,#11714,#11715,#11716,#11717,#11718,
#11719,#11720,#11721,#11722,#11723,#11724,#11725,#11726,#11727,#11728,#11729,
#11730,#11731,#11732,#11733,#11734,#11735,#11736,#11737,#11738,#11739,#11740,
#11741,#11742,#11743,#11744,#11745,#11746,#11747,#11748,#11749,#11750,#11751,
#11752,#11753,#11754,#11755,#11756,#11757,#11758,#11759,#11760,#11761,#11762,
#11763,#11764,#11765,#11766,#11767,#11768,#11769,#11770,#11771,#11772,#11773,
#11774,#11775,#11776,#11777,#11778,#11779,#11780,#11781,#11782,#11783,#11784,
#11785,#11786,#11787,#11788,#11789,#11790,#11791,#11792),.UNSPECIFIED.,
 .F.,.F.,(4,3,3,3,3,3,3,3,3,3,3,3,3,3,3,3,3,3,3,3,3,3,3,3,3,3,3,3,3,3,3,
3,3,3,3,3,3,4),(10.3762723589309,10.4685607196145,10.560727614795,10.6549580113097,
10.7469711869423,10.838956356852,10.9309391472322,11.0268470571522,11.1189553523447,
11.2111259176515,11.3034309831953,11.3145707869122,11.4078036887453,11.500913534529,
11.5939277225349,11.6868775989975,11.779794413783,11.8727027895915,11.9656273355042,
12.0586527505373,12.151731115711,12.2449651361798,12.3145167992636,12.4074644695395,
12.5002843875549,12.5930043634112,12.6856547841058,12.778269017663,12.8708720387751,
12.9634888063115,13.0562045696504,13.1489717592456,13.2418953378247,13.314462811615,
13.4075374976835,13.5005018407416,13.5933639283471,13.6621109872984),
 .UNSPECIFIED.);
#153=B_SPLINE_CURVE_WITH_KNOTS('',3,(#11795,#11796,#11797,#11798,#11799,
#11800,#11801,#11802,#11803,#11804,#11805,#11806,#11807,#11808,#11809,#11810,
#11811,#11812,#11813,#11814,#11815,#11816,#11817,#11818,#11819,#11820,#11821,
#11822,#11823,#11824,#11825,#11826,#11827,#11828,#11829,#11830,#11831,#11832,
#11833,#11834,#11835,#11836,#11837,#11838,#11839,#11840,#11841,#11842,#11843,
#11844,#11845,#11846,#11847,#11848,#11849,#11850,#11851,#11852,#11853,#11854,
#11855,#11856,#11857,#11858,#11859,#11860,#11861,#11862,#11863,#11864),
 .UNSPECIFIED.,.F.,.F.,(4,3,3,3,3,3,3,3,3,3,3,3,3,3,3,3,3,3,3,3,3,3,3,4),
(11.6152142277549,11.7104627373194,11.8056562041118,11.900816792875,11.9959935195508,
12.0911845217967,12.1864099267108,12.2816898891895,12.3771113362023,12.4726110332727,
12.5682798807942,12.6151602401062,12.7072927880287,12.7992864602223,12.8911700806882,
12.9829719958292,13.0747303838343,13.1664710617718,13.25821982499,13.3500638544193,
13.4419557180476,13.5340072043485,13.6151062524576,13.661880832927),
 .UNSPECIFIED.);
#154=B_SPLINE_CURVE_WITH_KNOTS('',3,(#11870,#11871,#11872,#11873,#11874,
#11875,#11876,#11877,#11878,#11879,#11880,#11881,#11882,#11883,#11884,#11885,
#11886,#11887,#11888,#11889,#11890,#11891,#11892,#11893,#11894,#11895,#11896,
#11897,#11898,#11899,#11900,#11901,#11902,#11903,#11904,#11905,#11906,#11907,
#11908,#11909,#11910,#11911,#11912,#11913,#11914,#11915,#11916,#11917,#11918,
#11919,#11920,#11921,#11922,#11923,#11924,#11925,#11926,#11927,#11928,#11929,
#11930,#11931,#11932,#11933,#11934,#11935,#11936,#11937,#11938,#11939,#11940,
#11941,#11942,#11943,#11944,#11945,#11946,#11947,#11948,#11949,#11950,#11951,
#11952,#11953,#11954,#11955,#11956,#11957,#11958,#11959,#11960,#11961,#11962,
#11963,#11964,#11965,#11966,#11967,#11968,#11969,#11970,#11971,#11972,#11973,
#11974,#11975,#11976,#11977,#11978,#11979,#11980,#11981,#11982,#11983,#11984,
#11985,#11986,#11987,#11988,#11989,#11990,#11991,#11992,#11993,#11994,#11995,
#11996,#11997,#11998,#11999,#12000,#12001,#12002,#12003,#12004,#12005,#12006,
#12007,#12008,#12009,#12010,#12011,#12012,#12013,#12014,#12015,#12016,#12017,
#12018,#12019,#12020,#12021,#12022,#12023,#12024,#12025,#12026,#12027,#12028,
#12029,#12030,#12031,#12032,#12033,#12034,#12035,#12036,#12037,#12038,#12039,
#12040,#12041,#12042,#12043,#12044,#12045,#12046,#12047,#12048,#12049,#12050,
#12051,#12052,#12053,#12054,#12055,#12056,#12057,#12058,#12059,#12060,#12061,
#12062,#12063,#12064,#12065,#12066,#12067,#12068,#12069,#12070,#12071,#12072,
#12073),.UNSPECIFIED.,.F.,.F.,(4,2,2,2,2,2,2,2,2,2,2,2,2,2,2,2,2,2,2,2,
2,2,2,2,2,2,2,2,2,2,2,2,2,2,2,2,2,2,2,2,2,2,2,2,2,2,2,2,2,2,2,2,2,2,2,2,
2,2,2,2,2,2,2,2,2,2,2,2,2,2,2,2,2,2,2,2,2,2,2,2,2,2,2,2,2,2,2,2,2,2,2,2,
2,2,2,2,2,2,2,2,2,4),(-1.37022537659221,-1.34091059982744,-1.33432719131615,
-1.3303909319413,-1.32736015588578,-1.32409755164556,-1.31893198307468,
-1.30204871993472,-1.27436763409897,-1.20187882557325,-1.17377960928441,
-1.16957709291693,-1.1674464593617,-1.16576780553845,-1.16381408405481,
-1.16031516703387,-1.14355099392605,-1.06708577498172,-1.01778424944133,
-1.01119847934814,-1.00726192833468,-1.00423159012833,-1.00097011411607,
-0.995807742098134,-0.978947757724557,-0.951318348613338,-0.878272261227642,
-0.850624656984496,-0.846437417232639,-0.844310230135465,-0.84263193635636,
-0.840675834471548,-0.837166371180659,-0.820231465470602,-0.743896134944801,
-0.694656347337957,-0.688058434107688,-0.684117998593137,-0.681086638284101,
-0.67782599594984,-0.67266905232386,-0.655863294413673,-0.628358683882797,
-0.554289454404455,-0.527442810043846,-0.523282445163439,-0.521160607566312,
-0.519481936297915,-0.517519845927585,-0.513986917321571,-0.496687651642819,
-0.420510968432387,-0.371613687460086,-0.365020492697749,-0.361080668421583,
-0.358048465132614,-0.357989283934159,-0.357924385584965,-0.357868206524929,
-0.357819584317401,-0.357777508247663,-0.35774110059434,-0.35770959993251,
-0.357673452353779,-0.357638479118564,-0.35760463897588,-0.357571893371848,
-0.357540205087393,-0.357509538189687,-0.357479857999926,-0.35745113104381,
-0.357423325030654,-0.357396408793136,-0.357370352278429,-0.357345128720867,
-0.357320712405916,-0.357297072275671,-0.357274182330256,-0.357252017493811,
-0.353792555790826,-0.347636689923209,-0.340058218326234,-0.324125423490495,
-0.276678078069955,-0.208783494514185,-0.201629712397283,-0.198940634478145,
-0.197342528679399,-0.195628651904034,-0.193235011566351,-0.187440230609289,
-0.160248598865694,-0.0750892562821783,-0.0558604189753205,-0.0436152515609683,
-0.0388953015602837,-0.0360480651305796,-0.0331759803957967,-0.0302282624267043,
-0.0263905830487572,-0.0167964234972045,-0.000966734669669255),
 .UNSPECIFIED.);
#155=B_SPLINE_CURVE_WITH_KNOTS('',3,(#12074,#12075,#12076,#12077,#12078,
#12079,#12080,#12081,#12082,#12083,#12084,#12085,#12086,#12087,#12088,#12089,
#12090,#12091,#12092,#12093,#12094,#12095,#12096,#12097,#12098,#12099,#12100,
#12101,#12102,#12103,#12104,#12105,#12106,#12107,#12108,#12109,#12110,#12111,
#12112,#12113,#12114,#12115,#12116,#12117,#12118,#12119,#12120,#12121,#12122,
#12123,#12124,#12125,#12126,#12127,#12128,#12129,#12130,#12131,#12132,#12133,
#12134,#12135,#12136,#12137,#12138,#12139,#12140),.UNSPECIFIED.,.F.,.F.,
(4,3,3,3,3,3,3,3,3,3,3,3,3,3,3,3,3,3,3,3,3,3,4),(13.6621109872984,13.7548852435726,
13.8476426210203,13.9404079052831,14.0339081349539,14.1268150028064,14.2206119133864,
14.3144088239664,14.4074983292472,14.5004620657044,14.5933276454891,14.6861257703182,
14.7788889547583,14.8716420039164,14.9644097079295,15.0572768974958,15.1501960256872,
15.2432708035197,15.3143548363177,15.4182322755584,15.5217902671822,15.6247747852697,
15.7079632677622),.UNSPECIFIED.);
#156=B_SPLINE_CURVE_WITH_KNOTS('',3,(#12142,#12143,#12144,#12145,#12146,
#12147,#12148,#12149,#12150,#12151,#12152,#12153,#12154,#12155,#12156,#12157,
#12158,#12159,#12160,#12161,#12162,#12163,#12164,#12165,#12166,#12167,#12168,
#12169,#12170,#12171,#12172,#12173,#12174,#12175,#12176,#12177,#12178,#12179,
#12180,#12181,#12182,#12183,#12184,#12185,#12186,#12187,#12188,#12189,#12190,
#12191,#12192,#12193,#12194,#12195,#12196,#12197,#12198,#12199,#12200,#12201,
#12202,#12203,#12204,#12205,#12206,#12207,#12208,#12209,#12210,#12211),
 .UNSPECIFIED.,.F.,.F.,(4,3,3,3,3,3,3,3,3,3,3,3,3,3,3,3,3,3,3,3,3,3,3,4),
(13.661880832927,13.7550145535338,13.8480359180392,13.9439129613854,14.0367976849942,
14.1296597979391,14.222523956533,14.3154148117948,14.4084097402506,14.5014672535618,
14.5946633566942,14.615052264809,14.708285208079,14.8013950963811,14.894409327926,
14.9873592492917,15.0802761098038,15.173184532111,15.266109125244,15.3591345883359,
15.4522130021073,15.5454470715631,15.6149982771603,15.707963267949),
 .UNSPECIFIED.);
#157=B_SPLINE_CURVE_WITH_KNOTS('',3,(#12212,#12213,#12214,#12215,#12216,
#12217,#12218,#12219,#12220,#12221,#12222,#12223,#12224,#12225,#12226,#12227,
#12228,#12229,#12230,#12231,#12232,#12233,#12234,#12235,#12236,#12237,#12238,
#12239,#12240,#12241,#12242,#12243,#12244,#12245,#12246,#12247,#12248,#12249,
#12250,#12251,#12252,#12253,#12254,#12255,#12256,#12257,#12258,#12259,#12260,
#12261,#12262,#12263,#12264,#12265,#12266,#12267,#12268,#12269,#12270,#12271,
#12272,#12273,#12274,#12275,#12276,#12277,#12278,#12279,#12280,#12281,#12282,
#12283,#12284,#12285,#12286,#12287,#12288,#12289,#12290,#12291,#12292,#12293,
#12294,#12295,#12296,#12297,#12298,#12299,#12300,#12301,#12302,#12303,#12304,
#12305,#12306,#12307,#12308,#12309,#12310,#12311,#12312,#12313,#12314,#12315,
#12316,#12317,#12318,#12319,#12320,#12321,#12322,#12323,#12324,#12325,#12326,
#12327,#12328,#12329,#12330,#12331,#12332,#12333,#12334,#12335,#12336,#12337,
#12338,#12339,#12340,#12341,#12342,#12343,#12344,#12345,#12346,#12347,#12348,
#12349,#12350,#12351,#12352,#12353,#12354,#12355,#12356,#12357,#12358,#12359,
#12360,#12361,#12362,#12363,#12364,#12365,#12366,#12367,#12368,#12369),
 .UNSPECIFIED.,.F.,.F.,(4,2,2,2,2,2,2,2,2,2,2,2,2,2,2,2,2,2,2,2,2,2,2,2,
2,2,2,2,2,2,2,2,2,2,2,2,2,2,2,2,2,2,2,2,2,2,2,2,2,2,2,2,2,2,2,2,2,2,2,2,
2,2,2,2,2,2,2,2,2,2,2,2,2,2,2,2,2,2,4),(-4.06120255059993,-3.98563093651712,
-3.95648723998739,-3.93900363536026,-3.9337996512044,-3.93054568897629,
-3.927545495221,-3.92368079394536,-3.91728694917056,-3.87478652528743,-3.81154283654031,
-3.78641054291921,-3.77775083177261,-3.77363233946665,-3.77033862668475,
-3.76843724623808,-3.76843169727313,-3.7684261277979,-3.76842020266436,
-3.76841417858657,-3.76840805352903,-3.7684018254137,-3.76672725759988,
-3.76458526153515,-3.76018046412751,-3.70378742243041,-3.66048805565629,
-3.63238508052738,-3.61530721998266,-3.61011483988667,-3.60684262793018,
-3.60380790987669,-3.59987349968863,-3.59330806707067,-3.54518739555943,
-3.46818660168279,-3.45132555574338,-3.44781194086284,-3.44585052626606,
-3.44416849798318,-3.44203607305814,-3.43782912895715,-3.40949788501506,
-3.3373981623366,-3.30976078229524,-3.29289800496867,-3.2877355333589,-3.28447412216659,
-3.28144392589934,-3.27750767120283,-3.27092262666215,-3.22169970794755,
-3.14592784897398,-3.12832042484183,-3.12477302637789,-3.1228095549436,
-3.12113407500583,-3.1190219793966,-3.11489708395197,-3.0888726987146,-3.01373915889266,
-2.9864101678104,-2.96968546106006,-2.96454288763508,-2.96128898177692,
-2.9582622867068,-2.95432567725299,-2.94772929532905,-2.8975752535729,-2.81954364620963,
-2.80487885748976,-2.80152221963937,-2.79960157042717,-2.79792027503715,
-2.79574639791226,-2.79221594067299,-2.77172997379105,-2.76310662474663,
-2.69244553871344),.UNSPECIFIED.);
#158=B_SPLINE_CURVE_WITH_KNOTS('',3,(#12374,#12375,#12376,#12377,#12378,
#12379,#12380,#12381,#12382,#12383,#12384,#12385,#12386,#12387,#12388,#12389,
#12390,#12391,#12392,#12393,#12394,#12395,#12396,#12397,#12398,#12399,#12400,
#12401,#12402,#12403,#12404,#12405,#12406,#12407,#12408,#12409,#12410,#12411,
#12412,#12413,#12414,#12415,#12416,#12417,#12418,#12419,#12420,#12421,#12422,
#12423,#12424,#12425,#12426,#12427,#12428,#12429,#12430,#12431,#12432,#12433,
#12434,#12435,#12436,#12437,#12438,#12439,#12440,#12441,#12442,#12443,#12444,
#12445,#12446,#12447,#12448,#12449,#12450,#12451,#12452,#12453,#12454,#12455,
#12456,#12457,#12458,#12459,#12460,#12461,#12462,#12463,#12464,#12465,#12466,
#12467,#12468,#12469,#12470,#12471,#12472,#12473,#12474,#12475,#12476,#12477,
#12478,#12479,#12480,#12481,#12482,#12483,#12484,#12485,#12486,#12487,#12488,
#12489,#12490,#12491,#12492,#12493,#12494,#12495,#12496,#12497,#12498,#12499,
#12500,#12501,#12502,#12503,#12504,#12505,#12506,#12507,#12508,#12509,#12510,
#12511,#12512,#12513,#12514,#12515,#12516,#12517,#12518,#12519,#12520,#12521,
#12522,#12523,#12524,#12525,#12526,#12527,#12528,#12529,#12530,#12531,#12532,
#12533,#12534,#12535,#12536,#12537,#12538,#12539,#12540,#12541,#12542,#12543,
#12544,#12545,#12546,#12547,#12548,#12549,#12550,#12551,#12552,#12553,#12554,
#12555,#12556,#12557,#12558,#12559,#12560,#12561,#12562,#12563,#12564,#12565,
#12566,#12567,#12568,#12569,#12570,#12571,#12572,#12573,#12574,#12575,#12576,
#12577,#12578,#12579,#12580,#12581,#12582,#12583,#12584,#12585,#12586,#12587,
#12588,#12589),.UNSPECIFIED.,.F.,.F.,(4,2,2,2,2,2,2,2,2,2,2,2,2,2,2,2,2,
2,2,2,2,2,2,2,2,2,2,2,2,2,2,2,2,2,2,2,2,2,2,2,2,2,2,2,2,2,2,2,2,2,2,2,2,
2,2,2,2,2,2,2,2,2,2,2,2,2,2,2,2,2,2,2,2,2,2,2,2,2,2,2,2,2,2,2,2,2,2,2,2,
2,2,2,2,2,2,2,2,2,2,2,2,2,2,2,2,2,2,4),(-3.40022159451442,-3.3925401132152,
-3.3200050390171,-3.29235438762688,-3.27548412264847,-3.27032103375553,
-3.26705964286102,-3.26402975102361,-3.26009429546325,-3.25351143131809,
-3.20432783531026,-3.12804042133909,-3.11098569610243,-3.1074693544432,
-3.10551192600415,-3.10383397299881,-3.10170913726944,-3.09753242381139,
-3.07018138376164,-2.99683627903875,-2.96926380638888,-2.95242740298401,
-2.94726785950343,-2.94400713566057,-2.9409767780011,-2.93703917585256,
-2.93044932349352,-2.88092989287828,-2.80390463736647,-2.7878178537626,
-2.78436140521718,-2.78241699071641,-2.78073744627168,-2.77859408937043,
-2.77418488279155,-2.71819893788166,-2.67545672979554,-2.64679667237422,
-2.62948906307082,-2.62427798083233,-2.62100566616702,-2.61797889757186,
-2.614066204176,-2.60756229829595,-2.56201005594115,-2.4944036654252,-2.46825969003576,
-2.46258138440068,-2.46020576467742,-2.45849402512761,-2.45689066920433,
-2.45417405380509,-2.44683789853128,-2.39269897481404,-2.35094086384508,
-2.32325622336795,-2.30637011488509,-2.30120456608902,-2.29794217041142,
-2.29491172361986,-2.29097608412515,-2.28439409414145,-2.23531443419858,
-2.15923668276916,-2.14186746965592,-2.13833196816928,-2.13637011532168,
-2.13469222279945,-2.13257238790137,-2.12842018158147,-2.10178022082503,
-2.09186350730744,-2.03167536075008,-1.98694862586953,-1.98046071444936,
-1.9765524753541,-1.97352611548223,-1.97025122058457,-1.96502950273261,
-1.94762606752115,-1.9187391385546,-1.87617611232732,-1.82026864601881,
-1.81585648676625,-1.81371237128581,-1.81203256007626,-1.81008819935012,
-1.80663275527695,-1.79056621408816,-1.71355628532306,-1.66403361467725,
-1.65744290374154,-1.65350465165849,-1.6504737318586,-1.64721234376396,
-1.64205162508133,-1.62521044484006,-1.59762499205793,-1.52418393971989,
-1.49685097773187,-1.49267399540364,-1.49054880963011,-1.48887042187013,
-1.48691225260106,-1.48339422559622,-1.46632336136999,-1.39005788054266,
-1.37022537659221),.UNSPECIFIED.);
#159=B_SPLINE_CURVE_WITH_KNOTS('',3,(#12590,#12591,#12592,#12593,#12594,
#12595,#12596,#12597,#12598,#12599,#12600,#12601,#12602,#12603,#12604,#12605,
#12606,#12607,#12608,#12609,#12610,#12611,#12612,#12613,#12614,#12615,#12616,
#12617,#12618,#12619,#12620,#12621,#12622,#12623,#12624,#12625,#12626,#12627,
#12628,#12629,#12630,#12631,#12632,#12633,#12634,#12635,#12636,#12637,#12638,
#12639,#12640,#12641,#12642,#12643,#12644,#12645,#12646,#12647,#12648,#12649,
#12650,#12651,#12652,#12653,#12654,#12655,#12656,#12657,#12658,#12659,#12660,
#12661,#12662,#12663,#12664,#12665,#12666,#12667,#12668,#12669,#12670,#12671,
#12672,#12673,#12674,#12675,#12676,#12677,#12678,#12679,#12680,#12681,#12682,
#12683,#12684,#12685,#12686,#12687,#12688,#12689,#12690,#12691,#12692,#12693,
#12694,#12695,#12696,#12697,#12698,#12699,#12700,#12701,#12702,#12703,#12704,
#12705,#12706,#12707,#12708,#12709,#12710,#12711,#12712,#12713,#12714,#12715,
#12716,#12717,#12718,#12719,#12720,#12721,#12722,#12723,#12724,#12725,#12726,
#12727,#12728,#12729,#12730,#12731,#12732,#12733,#12734,#12735,#12736,#12737,
#12738,#12739,#12740,#12741,#12742,#12743,#12744,#12745,#12746,#12747,#12748,
#12749,#12750,#12751,#12752,#12753,#12754,#12755,#12756,#12757,#12758,#12759,
#12760,#12761,#12762,#12763,#12764,#12765,#12766,#12767,#12768,#12769,#12770,
#12771,#12772,#12773,#12774,#12775,#12776,#12777,#12778,#12779,#12780,#12781,
#12782,#12783,#12784,#12785,#12786,#12787,#12788,#12789,#12790,#12791,#12792,
#12793,#12794,#12795,#12796,#12797,#12798,#12799,#12800,#12801,#12802,#12803,
#12804,#12805,#12806,#12807,#12808,#12809,#12810,#12811),.UNSPECIFIED.,
 .F.,.F.,(4,2,2,2,2,2,2,2,2,2,2,2,2,2,2,2,2,2,2,2,2,2,2,2,2,2,2,2,2,2,2,
2,2,2,2,2,2,2,2,2,2,2,2,2,2,2,2,2,2,2,2,2,2,2,2,2,2,2,2,2,2,2,2,2,2,2,2,
2,2,2,2,2,2,2,2,2,2,2,2,2,2,2,2,2,2,2,2,2,2,2,2,2,2,2,2,2,2,2,2,2,2,2,2,
2,2,2,2,2,2,2,4),(-2.69244553871344,-2.69123390220975,-2.66351216289566,
-2.64661002537132,-2.64144315723391,-2.63818074862069,-2.63515085232453,
-2.63121671987635,-2.62463895963185,-2.57569886226652,-2.49956912753649,
-2.48221194837531,-2.47867692264336,-2.47671503442069,-2.47503737789983,
-2.47291794870337,-2.46876568067321,-2.44209528711233,-2.36786514684491,
-2.34040313139532,-2.32361626754396,-2.31846312957891,-2.31520444280347,
-2.31217459458479,-2.30823569593098,-2.30163938604602,-2.25173873785962,
-2.1739447321752,-2.15886500487573,-2.15547661035761,-2.15354760585632,
-2.15186677261722,-2.14970265785861,-2.14518476561153,-2.0977148457355,
-2.03153183178019,-2.00290916989459,-1.99711495885629,-1.99337526337154,
-1.99037851322074,-1.98697854965591,-1.98118591670721,-1.95745290307746,
-1.87805903643468,-1.83761200191641,-1.83311607563557,-1.83095618476786,
-1.82927563339033,-1.82734348673568,-1.82394164945751,-1.80867084322266,
-1.73105301696905,-1.68126353679017,-1.67466922392996,-1.67073064179387,
-1.66770053911554,-1.6644410886992,-1.65928569983533,-1.6424823358668,-1.61498019083181,
-1.54084252702486,-1.51406022810568,-1.50990364772197,-1.50778324838028,
-1.50610584586776,-1.50414570018307,-1.50061587033473,-1.48332583298547,
-1.40726644914206,-1.35815142411915,-1.35157078979615,-1.3476363163429,
-1.34460700185069,-1.34134606416725,-1.33618335185292,-1.31931176739594,
-1.29165341553657,-1.21889182349642,-1.1910209928546,-1.18682724618086,
-1.18469905141312,-1.18302118856845,-1.18106704238676,-1.17756453369895,
-1.16072947935636,-1.08434016724001,-1.03505412536001,-1.02847011594516,
-1.02453469032697,-1.02150526645892,-1.01824482560543,-1.01308421014322,
-0.99623121663964,-0.96861522334579,-0.895431670283169,-0.867901795449302,
-0.863719413968823,-0.861593638832768,-0.859915942506391,-0.857959975968885,
-0.854449260826696,-0.837479653525979,-0.761187883541069,-0.711973606440921,
-0.705378399957064,-0.701439648905281,-0.698409630433466,-0.69515048248527,
-0.689996026249312,-0.673199831892496,-0.662344722523992),.UNSPECIFIED.);
#160=B_SPLINE_CURVE_WITH_KNOTS('',3,(#12817,#12818,#12819,#12820,#12821,
#12822,#12823,#12824,#12825,#12826,#12827,#12828,#12829,#12830,#12831,#12832,
#12833,#12834,#12835,#12836,#12837,#12838,#12839,#12840,#12841,#12842,#12843,
#12844,#12845,#12846,#12847,#12848,#12849,#12850,#12851,#12852,#12853,#12854,
#12855,#12856,#12857,#12858,#12859,#12860,#12861,#12862,#12863,#12864,#12865,
#12866,#12867,#12868,#12869,#12870,#12871,#12872,#12873,#12874,#12875,#12876,
#12877,#12878,#12879,#12880,#12881,#12882,#12883,#12884,#12885,#12886,#12887,
#12888,#12889,#12890,#12891,#12892,#12893,#12894,#12895,#12896,#12897,#12898,
#12899,#12900,#12901,#12902,#12903,#12904,#12905,#12906,#12907,#12908,#12909,
#12910,#12911,#12912,#12913,#12914,#12915,#12916,#12917,#12918,#12919,#12920,
#12921,#12922,#12923,#12924,#12925,#12926,#12927,#12928,#12929,#12930,#12931,
#12932,#12933,#12934,#12935,#12936,#12937,#12938,#12939,#12940,#12941,#12942,
#12943,#12944,#12945,#12946,#12947,#12948,#12949,#12950,#12951,#12952,#12953,
#12954,#12955,#12956,#12957,#12958,#12959,#12960,#12961,#12962,#12963,#12964,
#12965,#12966,#12967,#12968,#12969,#12970,#12971,#12972,#12973,#12974),
 .UNSPECIFIED.,.F.,.F.,(4,2,2,2,2,2,2,2,2,2,2,2,2,2,2,2,2,2,2,2,2,2,2,2,
2,2,2,2,2,2,2,2,2,2,2,2,2,2,2,2,2,2,2,2,2,2,2,2,2,2,2,2,2,2,2,2,2,2,2,2,
2,2,2,2,2,2,2,2,2,2,2,2,2,2,2,2,2,2,4),(-1.36988642038638,-1.3413112663451,
-1.31332639502017,-1.30912817643698,-1.30699868518289,-1.30532029240606,
-1.30336605794606,-1.29986467780207,-1.28305909352352,-1.20662448920358,
-1.15736774933564,-1.15078323832296,-1.14684710852722,-1.14381689651347,
-1.14055535841533,-1.13539245967217,-1.11852678218158,-1.09088358878178,
-1.01805450344349,-0.990246337496509,-0.986053908400624,-0.983925649917715,
-0.982247352285227,-0.980292221850595,-0.976786736535938,-0.959913668674745,
-0.883529239114067,-0.834296324460669,-0.827712286680746,-0.823776293781452,
-0.820746101811455,-0.817484501228151,-0.812321324405555,-0.795453133645105,
-0.767804185329178,-0.695035676092615,-0.667178651308371,-0.662984483009059,
-0.660855853517954,-0.659177526655734,-0.657222664648347,-0.653718411777061,
-0.636865656306205,-0.560466115236699,-0.511225947278959,-0.50464176233137,
-0.500705725818408,-0.497675526209257,-0.494413942951445,-0.489250848012482,
-0.47238341260582,-0.444736199326516,-0.372935203092716,-0.344155914948134,
-0.339933756986813,-0.337799177424309,-0.336208633012441,-0.334334307168588,
-0.332334879940176,-0.329294205028423,-0.323654757567015,-0.310233371681277,
-0.208930142592438,-0.18583772763581,-0.179896465594955,-0.176428242222843,
-0.173436881472165,-0.169787214674185,-0.162839031221035,-0.11426220036506,
-0.0308869772400612,-0.0196703223883601,-0.0162071716242147,-0.0142404761879752,
-0.0125638474888604,-0.0109390323766698,-0.00886278152393431,-0.00528731446874136,
-0.000961764280122457),.UNSPECIFIED.);
#161=B_SPLINE_CURVE_WITH_KNOTS('',3,(#12975,#12976,#12977,#12978,#12979,
#12980,#12981,#12982,#12983,#12984,#12985,#12986,#12987,#12988,#12989,#12990,
#12991,#12992,#12993,#12994,#12995,#12996,#12997,#12998,#12999,#13000,#13001,
#13002,#13003,#13004,#13005,#13006,#13007,#13008,#13009,#13010,#13011,#13012,
#13013,#13014,#13015,#13016,#13017,#13018,#13019,#13020,#13021,#13022,#13023,
#13024,#13025,#13026,#13027,#13028,#13029,#13030,#13031,#13032,#13033,#13034,
#13035,#13036,#13037,#13038,#13039,#13040,#13041,#13042,#13043,#13044,#13045,
#13046,#13047,#13048,#13049,#13050,#13051,#13052,#13053,#13054,#13055,#13056,
#13057,#13058,#13059,#13060,#13061,#13062,#13063,#13064,#13065,#13066,#13067,
#13068),.UNSPECIFIED.,.F.,.F.,(4,2,2,2,2,2,2,2,2,2,2,2,2,2,2,2,2,2,2,2,
2,2,2,2,2,2,2,2,2,2,2,2,2,2,2,2,2,2,2,2,2,2,2,2,2,2,4),(-4.06143253580346,
-3.96549119249435,-3.9382033737247,-3.92149246432343,-3.91634736999491,
-3.91309020656234,-3.91005930184858,-3.90611550026312,-3.89950314368999,
-3.83153907990166,-3.76477803466754,-3.75874524557317,-3.75555607946893,
-3.7534952994355,-3.75157479538124,-3.75156849042742,-3.75156209358517,
-3.75155560294987,-3.7515490166095,-3.75154233261846,-3.7515355489364,-3.7515286634698,
-3.75152167405901,-3.75151457851469,-3.75150737455215,-3.74987537495363,
-3.74774297096556,-3.7435299674707,-3.71512361309314,-3.64275295956895,
-3.61528600507965,-3.59849634827436,-3.59334238005485,-3.5900831563305,
-3.58705279448121,-3.58311319904763,-3.57651562420591,-3.52656638707188,
-3.44833232271012,-3.43373212251742,-3.43037692763681,-3.42845490975064,
-3.42677231646694,-3.4245955666775,-3.4210563496417,-3.40040424022381,-3.40022159451442),
 .UNSPECIFIED.);
#162=B_SPLINE_CURVE_WITH_KNOTS('',3,(#13070,#13071,#13072,#13073,#13074,
#13075,#13076,#13077,#13078,#13079,#13080,#13081,#13082,#13083,#13084,#13085,
#13086,#13087,#13088,#13089,#13090,#13091,#13092,#13093,#13094,#13095,#13096,
#13097,#13098,#13099,#13100,#13101,#13102,#13103,#13104,#13105,#13106,#13107,
#13108,#13109,#13110,#13111,#13112,#13113,#13114,#13115,#13116,#13117,#13118,
#13119,#13120,#13121,#13122,#13123,#13124,#13125,#13126,#13127,#13128,#13129,
#13130,#13131,#13132,#13133,#13134,#13135,#13136,#13137,#13138,#13139,#13140,
#13141,#13142,#13143,#13144,#13145,#13146,#13147,#13148,#13149,#13150,#13151,
#13152,#13153,#13154,#13155,#13156,#13157,#13158,#13159,#13160,#13161,#13162,
#13163,#13164,#13165,#13166,#13167,#13168,#13169,#13170,#13171,#13172,#13173,
#13174,#13175,#13176,#13177,#13178,#13179,#13180,#13181,#13182,#13183,#13184,
#13185,#13186,#13187,#13188,#13189,#13190,#13191),.UNSPECIFIED.,.F.,.F.,
(4,2,2,2,2,2,2,2,2,2,2,2,2,2,2,2,2,2,2,2,2,2,2,2,2,2,2,2,2,2,2,2,2,2,2,
2,2,2,2,2,2,2,2,2,2,2,2,2,2,2,2,2,2,2,2,2,2,2,2,2,4),(-0.662344722523992,
-0.645714028626579,-0.571423472767882,-0.544750670504654,-0.540598227240143,
-0.538478802736249,-0.536801540409405,-0.534840810959558,-0.531308250736471,
-0.513971430648279,-0.437946925193404,-0.388871653187486,-0.382276442410484,
-0.378337696144331,-0.375307685860361,-0.375236453617864,-0.375175001757771,
-0.375121980981308,-0.375076228319364,-0.375036741775316,-0.37500265825663,
-0.374973234339956,-0.374937579532359,-0.374903097779416,-0.374869745847379,
-0.3748374835443,-0.374806272195281,-0.374776074601791,-0.374746854978714,
-0.374718578900171,-0.374691213247298,-0.37466472616437,-0.374639087009157,
-0.374614268603377,-0.374590244897587,-0.374566984420498,-0.374544460938557,
-0.374522649215573,-0.371071741422611,-0.364964378064538,-0.357446145143455,
-0.34168481445426,-0.295056650901346,-0.226075013085308,-0.218917170937421,
-0.216228308672131,-0.214630814899865,-0.212916245490462,-0.210521815706478,
-0.204728045970659,-0.177557726175298,-0.110034475114551,-0.0908275066279576,
-0.0641104113689985,-0.058437561695102,-0.0547350451309201,-0.0517409172081973,
-0.0489229383257218,-0.0455619196258216,-0.0406606372590674,-0.000962269056679762),
 .UNSPECIFIED.);
#163=B_SPLINE_CURVE_WITH_KNOTS('',3,(#13192,#13193,#13194,#13195,#13196,
#13197,#13198,#13199),.UNSPECIFIED.,.F.,.F.,(4,1,1,1,1,4),(28.2743413277526,
28.6142964377282,29.6142424500796,30.6141884624309,31.6141344747823,32.5106472410873),
 .UNSPECIFIED.);
#164=B_SPLINE_CURVE_WITH_KNOTS('',3,(#13204,#13205,#13206,#13207,#13208,
#13209,#13210,#13211,#13212,#13213,#13214,#13215,#13216,#13217,#13218,#13219,
#13220,#13221,#13222,#13223,#13224,#13225,#13226,#13227,#13228,#13229,#13230,
#13231,#13232,#13233,#13234,#13235,#13236,#13237,#13238,#13239,#13240,#13241,
#13242,#13243,#13244,#13245,#13246,#13247,#13248,#13249,#13250,#13251,#13252,
#13253,#13254,#13255,#13256,#13257,#13258,#13259,#13260,#13261,#13262,#13263,
#13264,#13265,#13266,#13267,#13268,#13269,#13270,#13271,#13272,#13273,#13274,
#13275,#13276,#13277,#13278,#13279,#13280,#13281,#13282,#13283,#13284,#13285,
#13286,#13287,#13288,#13289,#13290,#13291,#13292,#13293,#13294,#13295,#13296,
#13297,#13298,#13299,#13300,#13301,#13302,#13303,#13304,#13305,#13306,#13307,
#13308,#13309,#13310,#13311,#13312,#13313,#13314,#13315,#13316,#13317,#13318,
#13319,#13320,#13321,#13322,#13323,#13324,#13325,#13326,#13327,#13328,#13329,
#13330,#13331,#13332,#13333,#13334,#13335,#13336,#13337,#13338,#13339,#13340,
#13341,#13342,#13343,#13344,#13345,#13346,#13347,#13348,#13349,#13350,#13351,
#13352,#13353,#13354,#13355,#13356,#13357,#13358,#13359,#13360,#13361,#13362,
#13363,#13364,#13365,#13366,#13367,#13368,#13369,#13370,#13371,#13372,#13373,
#13374,#13375,#13376,#13377,#13378,#13379,#13380,#13381,#13382,#13383,#13384,
#13385,#13386,#13387,#13388,#13389,#13390,#13391,#13392,#13393,#13394,#13395,
#13396,#13397,#13398,#13399,#13400,#13401,#13402,#13403,#13404,#13405,#13406,
#13407,#13408,#13409,#13410,#13411,#13412,#13413,#13414,#13415,#13416,#13417,
#13418,#13419,#13420,#13421,#13422,#13423),.UNSPECIFIED.,.F.,.F.,(4,2,2,
2,2,2,2,2,2,2,2,2,2,2,2,2,2,2,2,2,2,2,2,2,2,2,2,2,2,2,2,2,2,2,2,2,2,2,2,
2,2,2,2,2,2,2,2,2,2,2,2,2,2,2,2,2,2,2,2,2,2,2,2,2,2,2,2,2,2,2,2,2,2,2,2,
2,2,2,2,2,2,2,2,2,2,2,2,2,2,2,2,2,2,2,2,2,2,2,2,2,2,2,2,2,2,2,2,2,2,4),
(-3.39981704860417,-3.39949957029591,-3.39290308880973,-3.34363862625196,
-3.26713372109305,-3.25038713773088,-3.24688975491302,-3.24493660514252,
-3.24325842520933,-3.24112829123458,-3.23692603631769,-3.20879373891644,
-3.13643276223271,-3.10876845785778,-3.09189253049485,-3.086729023892,-3.08346767212296,
-3.08043802567777,-3.0765031855718,-3.06992200454182,-3.02080523060401,
-2.94465027400736,-2.92742144649204,-2.92389489709134,-2.92193531909049,
-2.92025769523073,-2.91813606062682,-2.91397398964407,-2.88703691376175,
-2.81316510203951,-2.78565562204065,-2.76884704110681,-2.76369076189058,
-2.76043088517301,-2.75740047479573,-2.75346161034759,-2.74686701186692,
-2.69708932605819,-2.61938469249513,-2.60415005598616,-2.60075023644575,
-2.59881831473613,-2.59713716814004,-2.59497555505549,-2.59148693020392,
-2.57183182725261,-2.56242134371727,-2.49040724573827,-2.4627089495513,
-2.44581759615135,-2.44065197954643,-2.43738989560931,-2.43435998316739,
-2.43042538520751,-2.42384590304496,-2.37484858952389,-2.29892511217508,
-2.2813583025512,-2.27781168297495,-2.27584759086462,-2.27417016450779,
-2.27205396912217,-2.26791801437609,-2.24170629106371,-2.16585675567565,
-2.13911703470754,-2.12264675106471,-2.11752773573311,-2.11427580573156,
-2.11124192428133,-2.10728302503174,-2.10062041294131,-2.03647708621462,
-2.03071903932308,-1.96359321873984,-1.95657860119534,-1.95391099896981,
-1.95231722997155,-1.95059884869207,-1.94818612630463,-1.9422851200763,
-1.91415533048361,-1.88888017302048,-1.80868427644457,-1.79808778465268,
-1.7936350751821,-1.79083545880277,-1.78776045094286,-1.78349287729285,
-1.77324670208299,-1.72658686968809,-1.67283875181467,-1.66374855757199,
-1.63636339041546,-1.63218519025583,-1.63005996735404,-1.62838190255909,
-1.62642455720781,-1.62290890819997,-1.60586727707371,-1.52960738044998,
-1.48043483245754,-1.47385200532895,-1.46991636613453,-1.46688623012685,
-1.46362447666781,-1.45846060352996,-1.44158606679677,-1.41392256520755,
-1.36988642038638),.UNSPECIFIED.);
#165=B_SPLINE_CURVE_WITH_KNOTS('',3,(#13425,#13426,#13427,#13428,#13429,
#13430),.UNSPECIFIED.,.F.,.F.,(4,1,1,4),(32.5106472410873,32.6140804871337,
33.614026499485,34.5575121440499),.UNSPECIFIED.);
#166=B_SPLINE_CURVE_WITH_KNOTS('',3,(#13431,#13432,#13433,#13434,#13435,
#13436,#13437,#13438,#13439,#13440,#13441,#13442,#13443,#13444,#13445,#13446,
#13447,#13448,#13449,#13450,#13451,#13452,#13453,#13454,#13455,#13456,#13457,
#13458,#13459,#13460,#13461,#13462,#13463,#13464,#13465,#13466,#13467,#13468,
#13469,#13470,#13471,#13472,#13473,#13474,#13475,#13476,#13477,#13478,#13479,
#13480,#13481,#13482,#13483,#13484,#13485,#13486,#13487,#13488,#13489,#13490,
#13491,#13492,#13493,#13494,#13495,#13496,#13497,#13498,#13499,#13500,#13501,
#13502,#13503,#13504,#13505,#13506,#13507,#13508,#13509,#13510,#13511,#13512,
#13513,#13514,#13515,#13516,#13517,#13518,#13519,#13520,#13521,#13522,#13523,
#13524,#13525,#13526,#13527,#13528,#13529,#13530,#13531,#13532,#13533,#13534,
#13535,#13536,#13537,#13538,#13539,#13540,#13541,#13542,#13543,#13544,#13545,
#13546,#13547,#13548,#13549,#13550,#13551,#13552,#13553,#13554,#13555,#13556,
#13557,#13558,#13559,#13560,#13561,#13562,#13563,#13564,#13565,#13566,#13567,
#13568,#13569,#13570,#13571,#13572,#13573,#13574,#13575,#13576,#13577,#13578,
#13579,#13580,#13581,#13582,#13583,#13584,#13585,#13586,#13587,#13588,#13589,
#13590,#13591,#13592),.UNSPECIFIED.,.F.,.F.,(4,2,2,2,2,2,2,2,2,2,2,2,2,
2,2,2,2,2,2,2,2,2,2,2,2,2,2,2,2,2,2,2,2,2,2,2,2,2,2,2,2,2,2,2,2,2,2,2,2,
2,2,2,2,2,2,2,2,2,2,2,2,2,2,2,2,2,2,2,2,2,2,2,2,2,2,2,2,2,2,2,4),(-4.06085147293434,
-4.05310077188983,-4.04796490762521,-4.04572245654519,-4.04404186582043,
-4.04244042015484,-4.04083738496685,-4.03857436223626,-4.03249414860606,
-4.02032878775457,-3.93337662315455,-3.90664620310083,-3.89018244347752,
-3.88506615529543,-3.88181614393027,-3.87878418869646,-3.87482800649026,
-3.86817044713076,-3.80212119708593,-3.74694624012344,-3.73306234460286,
-3.72728776079619,-3.72419632428553,-3.72217634002965,-3.72028936261388,
-3.71867837800603,-3.71655666347782,-3.71225238564042,-3.68268555244652,
-3.61176490728404,-3.58415659727521,-3.56730666185997,-3.56214739635258,
-3.55888789026005,-3.55585939005812,-3.55192524019188,-3.54534348072126,
-3.49610042606097,-3.41978453366031,-3.40282543481444,-3.39931602836641,
-3.3973606943214,-3.39568345178764,-3.3935581594255,-3.38937649745657,-3.36183891339592,
-3.28874653477381,-3.26114796949512,-3.24430200803514,-3.23914298662774,
-3.23588341051888,-3.23285469050179,-3.22892003534876,-3.22233694632319,
-3.17304358878905,-3.0966243044284,-3.07979763755673,-3.07629610439543,
-3.07434241718201,-3.07266488956438,-3.07053705264485,-3.06634379496547,
-3.03846243566354,-2.96579113436638,-2.938149403629,-2.9212843159247,-2.91612299369249,
-2.91286278311782,-2.90983403881386,-2.90590015445412,-2.89932012257902,
-2.85019655859923,-2.77412278613023,-2.75681775538367,-2.7532874611796,
-2.7513274383532,-2.74965044806575,-2.74753094915117,-2.74337707861589,
-2.71664512289895,-2.69231343346385),.UNSPECIFIED.);
#167=B_SPLINE_CURVE_WITH_KNOTS('',3,(#13598,#13599,#13600,#13601,#13602,
#13603,#13604,#13605,#13606,#13607,#13608,#13609,#13610,#13611,#13612,#13613,
#13614,#13615,#13616,#13617,#13618,#13619,#13620,#13621,#13622,#13623,#13624,
#13625,#13626,#13627,#13628,#13629,#13630,#13631,#13632,#13633,#13634,#13635,
#13636,#13637,#13638,#13639,#13640,#13641,#13642,#13643,#13644,#13645,#13646,
#13647,#13648,#13649,#13650,#13651,#13652,#13653,#13654,#13655,#13656,#13657,
#13658,#13659,#13660,#13661,#13662,#13663,#13664,#13665,#13666,#13667,#13668,
#13669,#13670,#13671,#13672,#13673,#13674,#13675,#13676,#13677,#13678,#13679,
#13680,#13681,#13682,#13683,#13684,#13685,#13686,#13687,#13688,#13689,#13690,
#13691,#13692,#13693,#13694,#13695,#13696,#13697,#13698,#13699,#13700,#13701,
#13702,#13703,#13704,#13705,#13706,#13707,#13708,#13709,#13710,#13711,#13712,
#13713,#13714,#13715,#13716,#13717,#13718,#13719,#13720,#13721,#13722,#13723,
#13724,#13725,#13726,#13727,#13728,#13729,#13730,#13731,#13732,#13733,#13734,
#13735,#13736,#13737,#13738,#13739,#13740,#13741,#13742,#13743,#13744,#13745,
#13746,#13747,#13748,#13749,#13750,#13751,#13752,#13753,#13754,#13755,#13756,
#13757,#13758,#13759,#13760,#13761,#13762,#13763,#13764,#13765,#13766,#13767,
#13768,#13769,#13770,#13771,#13772,#13773,#13774,#13775,#13776,#13777,#13778,
#13779),.UNSPECIFIED.,.F.,.F.,(4,2,2,2,2,2,2,2,2,2,2,2,2,2,2,2,2,2,2,2,
2,2,2,2,2,2,2,2,2,2,2,2,2,2,2,2,2,2,2,2,2,2,2,2,2,2,2,2,2,2,2,2,2,2,2,2,
2,2,2,2,2,2,2,2,2,2,2,2,2,2,2,2,2,2,2,2,2,2,2,2,2,2,2,2,2,2,2,2,2,2,4),
(-1.36989260040055,-1.34694907025288,-1.29727439722468,-1.29068106761255,
-1.286742178582,-1.2837113098679,-1.28045050923884,-1.27529185373621,-1.25846753342456,
-1.23092008416594,-1.15715155332722,-1.13007914422047,-1.12591148078631,
-1.12378838841277,-1.12211033476853,-1.12015107721843,-1.11662718200838,
-1.09945141006572,-1.02328098131251,-0.974151816281154,-0.96756931407155,
-0.96363357310733,-0.960603185648537,-0.957340990987224,-0.952176055765177,
-0.935294788795801,-0.907616928940878,-0.835127854039516,-0.80703471412696,
-0.802832671510397,-0.800702246102006,-0.799023633445816,-0.797069735581214,
-0.793570427280163,-0.776802713138018,-0.700331202766069,-0.651082868466669,
-0.644482445262207,-0.640541479382043,-0.637510273701122,-0.634250350689317,
-0.62909572183803,-0.61230804644454,-0.584844443998596,-0.510423746113522,
-0.48384351450654,-0.479693475653538,-0.477574144930029,-0.475896353579631,
-0.473934272881937,-0.470397444343366,-0.453002478716234,-0.376989927622464,
-0.327967436876231,-0.320789114192507,-0.31701197919373,-0.314077215359215,
-0.314011445492452,-0.31395001612433,-0.313892464978884,-0.313838393819533,
-0.313787460593142,-0.313739368673774,-0.313693859328444,-0.313650705654848,
-0.313609707688398,-0.313570688401014,-0.313533490397462,-0.313497973192461,
-0.313464010937888,-0.313431490500467,-0.313400309848774,-0.313370376705422,
-0.313341607360951,-0.313313925675485,-0.309734378318534,-0.305877998963111,
-0.288584007343764,-0.259951770413244,-0.217139399379979,-0.161104772996814,
-0.156695254884214,-0.154551761741178,-0.15287212300594,-0.150927600882317,
-0.147470983225329,-0.131383103492649,-0.0543953119851398,-0.0142431875939723,
-0.00563614058459413,-0.000962618911395125),.UNSPECIFIED.);
#168=B_SPLINE_CURVE_WITH_KNOTS('',3,(#13780,#13781,#13782,#13783,#13784,
#13785,#13786,#13787,#13788,#13789,#13790,#13791,#13792,#13793,#13794,#13795,
#13796,#13797,#13798,#13799,#13800,#13801,#13802,#13803,#13804,#13805,#13806,
#13807,#13808,#13809,#13810,#13811,#13812,#13813,#13814,#13815,#13816,#13817,
#13818,#13819,#13820,#13821,#13822,#13823,#13824,#13825,#13826,#13827,#13828,
#13829,#13830,#13831,#13832,#13833,#13834,#13835,#13836,#13837,#13838,#13839,
#13840,#13841,#13842,#13843,#13844,#13845,#13846,#13847,#13848,#13849,#13850,
#13851,#13852,#13853,#13854,#13855,#13856,#13857),.UNSPECIFIED.,.F.,.F.,
(4,2,2,2,2,2,2,2,2,2,2,2,2,2,2,2,2,2,2,2,2,2,2,2,2,2,2,2,2,2,2,2,2,2,2,
2,2,2,4),(-4.0609098086769,-4.05711133593753,-4.05417360536516,-4.05128946276244,
-4.04842506637434,-4.04362140952887,-4.03084245516691,-3.93391530616202,
-3.90084440751831,-3.89442701347254,-3.89193235729023,-3.89019869557731,
-3.88862368915904,-3.88605254837563,-3.87962813169656,-3.80516967931925,
-3.74159650188201,-3.7365006198925,-3.7330591784387,-3.72977770511242,-3.72685566977004,
-3.72308032737714,-3.71590642563688,-3.66684648587034,-3.59076004029415,
-3.57345066016846,-3.56991965018618,-3.5679592390965,-3.56628191276532,
-3.56416194845147,-3.56000702082474,-3.53325930510304,-3.4591499057468,
-3.43167510792401,-3.41488225249231,-3.40972809161283,-3.40646892852742,
-3.40343874917258,-3.39981704860417),.UNSPECIFIED.);
#169=B_SPLINE_CURVE_WITH_KNOTS('',3,(#13858,#13859,#13860,#13861,#13862,
#13863,#13864,#13865,#13866,#13867,#13868,#13869,#13870,#13871,#13872,#13873,
#13874,#13875,#13876,#13877,#13878,#13879,#13880,#13881,#13882,#13883,#13884,
#13885,#13886,#13887,#13888,#13889,#13890,#13891,#13892,#13893,#13894,#13895,
#13896,#13897,#13898,#13899,#13900,#13901,#13902,#13903,#13904,#13905,#13906,
#13907,#13908,#13909,#13910,#13911,#13912,#13913,#13914,#13915,#13916,#13917,
#13918,#13919,#13920,#13921,#13922,#13923,#13924,#13925,#13926,#13927,#13928,
#13929,#13930,#13931,#13932,#13933,#13934,#13935,#13936,#13937,#13938,#13939,
#13940,#13941,#13942,#13943,#13944,#13945,#13946,#13947,#13948,#13949,#13950,
#13951,#13952,#13953,#13954,#13955,#13956,#13957,#13958,#13959,#13960,#13961,
#13962,#13963,#13964,#13965,#13966,#13967,#13968,#13969,#13970,#13971,#13972,
#13973,#13974,#13975,#13976,#13977,#13978,#13979,#13980,#13981,#13982,#13983,
#13984,#13985,#13986,#13987,#13988,#13989,#13990,#13991,#13992,#13993,#13994,
#13995,#13996,#13997,#13998,#13999,#14000,#14001,#14002,#14003,#14004,#14005,
#14006,#14007,#14008,#14009,#14010,#14011,#14012,#14013,#14014,#14015,#14016,
#14017,#14018,#14019,#14020,#14021,#14022,#14023,#14024,#14025,#14026,#14027,
#14028,#14029,#14030,#14031,#14032,#14033,#14034,#14035,#14036,#14037,#14038,
#14039,#14040,#14041,#14042,#14043,#14044,#14045,#14046,#14047,#14048,#14049,
#14050,#14051,#14052,#14053,#14054,#14055,#14056,#14057,#14058,#14059,#14060,
#14061,#14062,#14063,#14064,#14065,#14066,#14067,#14068,#14069),
 .UNSPECIFIED.,.F.,.F.,(4,2,2,2,2,2,2,2,2,2,2,2,2,2,2,2,2,2,2,2,2,2,2,2,
2,2,2,2,2,2,2,2,2,2,2,2,2,2,2,2,2,2,2,2,2,2,2,2,2,2,2,2,2,2,2,2,2,2,2,2,
2,2,2,2,2,2,2,2,2,2,2,2,2,2,2,2,2,2,2,2,2,2,2,2,2,2,2,2,2,2,2,2,2,2,2,2,
2,2,2,2,2,2,2,2,2,4),(-2.69231343346385,-2.64250090796024,-2.61502009310778,
-2.59822504553809,-2.59307125462505,-2.58981258871412,-2.58678306006822,
-2.58284500332925,-2.57625103693778,-2.52643937039689,-2.44876246795497,
-2.4335256364613,-2.43012637766502,-2.42819494839645,-2.42651435251194,
-2.42435364374961,-2.41985377925528,-2.37059577266759,-2.32147112749855,
-2.29267881511926,-2.27531589822419,-2.27010010604013,-2.26682753811948,
-2.26380238651174,-2.25989439124412,-2.25340399660443,-2.2083829963703,
-2.14090920941316,-2.1141736347455,-2.10842901595149,-2.10604276362931,
-2.10432963063252,-2.10272997071654,-2.10003013447172,-2.09280039695301,
-2.03153620018936,-1.961826828632,-1.95076205203216,-1.94623309039102,-1.94342036938971,
-1.94035875644004,-1.93616045256383,-1.92631918996058,-1.8830810832417,
-1.80824312733514,-1.78825875186903,-1.7847535240704,-1.78258718618012,
-1.78090593238775,-1.7789779189676,-1.77559458578027,-1.76059050459986,
-1.68275474821951,-1.63289141875531,-1.62629611977262,-1.62235743848731,
-1.61932754688473,-1.61606860761162,-1.61091463562352,-1.5941214073392,
-1.56664193409925,-1.49231135303828,-1.46567075175513,-1.46151963551514,
-1.45940055901531,-1.45772339337683,-1.45576256705092,-1.45222934083547,
-1.43487944453747,-1.358867986863,-1.3097724587627,-1.30319234920908,-1.29925808218646,
-1.29622886413424,-1.2929679686192,-1.28780519123183,-1.2709321980056,-1.24327018294436,
-1.17057353209847,-1.14265439142622,-1.1384591123928,-1.13633060376794,
-1.13465273026236,-1.13269883987765,-1.12919745761532,-1.11238054035069,
-1.03597847812415,-0.986689714546489,-0.980105733530443,-0.976170336867778,
-0.973140941759397,-0.969880537869576,-0.964719992859611,-0.947867318275063,
-0.920251879620666,-0.847074944040324,-0.819542446406734,-0.815360019889002,
-0.813234248561001,-0.811556582967808,-0.809600692896254,-0.80609015138467,
-0.789122092021607,-0.712831953229946,-0.663619336930725,-0.662240502390468),
 .UNSPECIFIED.);
#170=B_SPLINE_CURVE_WITH_KNOTS('',3,(#14074,#14075,#14076,#14077,#14078,
#14079,#14080,#14081,#14082,#14083,#14084,#14085,#14086,#14087,#14088,#14089,
#14090,#14091,#14092,#14093,#14094,#14095,#14096,#14097,#14098,#14099,#14100,
#14101,#14102,#14103,#14104,#14105,#14106,#14107,#14108,#14109,#14110,#14111,
#14112,#14113,#14114,#14115,#14116,#14117,#14118,#14119,#14120,#14121,#14122,
#14123,#14124,#14125,#14126,#14127,#14128,#14129,#14130,#14131,#14132,#14133,
#14134,#14135,#14136,#14137,#14138,#14139,#14140,#14141,#14142,#14143,#14144,
#14145,#14146,#14147,#14148,#14149,#14150,#14151,#14152,#14153,#14154,#14155,
#14156,#14157,#14158,#14159,#14160,#14161,#14162,#14163,#14164,#14165,#14166,
#14167,#14168,#14169,#14170,#14171,#14172,#14173,#14174,#14175,#14176,#14177,
#14178,#14179,#14180,#14181,#14182,#14183,#14184,#14185,#14186,#14187,#14188,
#14189,#14190,#14191,#14192,#14193,#14194,#14195,#14196,#14197,#14198,#14199,
#14200,#14201,#14202,#14203,#14204,#14205,#14206,#14207,#14208,#14209,#14210,
#14211,#14212,#14213,#14214,#14215,#14216,#14217,#14218,#14219,#14220,#14221,
#14222,#14223,#14224,#14225,#14226,#14227,#14228,#14229,#14230,#14231,#14232,
#14233,#14234,#14235,#14236,#14237,#14238,#14239,#14240,#14241,#14242,#14243,
#14244,#14245,#14246,#14247,#14248,#14249,#14250,#14251,#14252,#14253,#14254,
#14255,#14256,#14257,#14258,#14259,#14260,#14261,#14262,#14263,#14264,#14265,
#14266,#14267,#14268,#14269,#14270,#14271,#14272,#14273,#14274,#14275,#14276,
#14277,#14278,#14279,#14280,#14281,#14282,#14283,#14284,#14285,#14286,#14287,
#14288,#14289,#14290,#14291,#14292,#14293,#14294,#14295,#14296,#14297,#14298,
#14299,#14300,#14301),.UNSPECIFIED.,.F.,.F.,(4,2,2,2,2,2,2,2,2,2,2,2,2,
2,2,2,2,2,2,2,2,2,2,2,2,2,2,2,2,2,2,2,2,2,2,2,2,2,2,2,2,2,2,2,2,2,2,2,2,
2,2,2,2,2,2,2,2,2,2,2,2,2,2,2,2,2,2,2,2,2,2,2,2,2,2,2,2,2,2,2,2,2,2,2,2,
2,2,2,2,2,2,2,2,2,2,2,2,2,2,2,2,2,2,2,2,2,2,2,2,2,2,2,2,4),(-3.39991588284246,
-3.39040284696551,-3.38689701771358,-3.38494201102694,-3.38326400840224,
-3.38113637903207,-3.37694595249143,-3.3491808323736,-3.27636701760464,
-3.24874414704973,-3.23188624426278,-3.22672468256399,-3.2234637365705,
-3.22043389940239,-3.21649800573895,-3.20991328716416,-3.16062262439996,
-3.08411107232553,-3.06736478764203,-3.06386724474948,-3.0619139741981,
-3.06023567099159,-3.05810535544347,-3.05390266630649,-3.02576425173291,
-2.95340304389138,-2.92573630206508,-2.90885896452811,-2.90369506419902,
-2.9004334724363,-2.89740360904243,-2.8934684956751,-2.88688687634004,-2.83776838184286,
-2.76161152416422,-2.74437649931954,-2.74084940251167,-2.73888961936069,
-2.73721188076596,-2.73509017907659,-2.73092820990048,-2.70400051020518,
-2.63010853649165,-2.60259890823962,-2.58578991792256,-2.58063335541558,
-2.57737326315395,-2.57434262722422,-2.57040343381606,-2.5638082056094,
-2.51401906798455,-2.43628635191589,-2.42107779675773,-2.41767959355126,
-2.41574794175036,-2.41406661262627,-2.41190421795168,-2.40739823800769,
-2.3658438194634,-2.30700794897804,-2.27953082753528,-2.2627355829291,-2.25758020882409,
-2.2543201675795,-2.2512890950447,-2.24734864596555,-2.24074979664955,-2.19080413950868,
-2.11260225637664,-2.09793948662124,-2.09457925819915,-2.09265584853259,
-2.0909730130786,-2.08879723726757,-2.08526214730072,-2.06470505519974,
-2.03142818364736,-1.94831592242864,-1.93796263568773,-1.93399190062331,
-1.93113525016105,-1.92810055832378,-1.92406894905081,-1.91517481777322,
-1.87941363195954,-1.80918440574648,-1.80004154742277,-1.79251830471457,
-1.7754415385953,-1.77209921129998,-1.76998180359689,-1.7683041530891,-1.76634064031836,
-1.76279720824143,-1.74528870808485,-1.66935766903248,-1.62035207886556,
-1.61377204035047,-1.60983700933843,-1.60680672218784,-1.60354419568562,
-1.59837779704592,-1.58148333137201,-1.55377524021807,-1.48163442798051,
-1.47180014855695,-1.45257718007089,-1.44911104050935,-1.44695605148667,
-1.44527532218127,-1.44333850822202,-1.43991723989069,-1.42437016231373,
-1.36989260040055),.UNSPECIFIED.);
#171=B_SPLINE_CURVE_WITH_KNOTS('',3,(#14303,#14304,#14305,#14306,#14307,
#14308,#14309,#14310,#14311,#14312,#14313,#14314,#14315,#14316,#14317,#14318,
#14319,#14320,#14321,#14322,#14323,#14324,#14325,#14326,#14327,#14328,#14329,
#14330,#14331,#14332,#14333,#14334,#14335,#14336,#14337,#14338,#14339,#14340,
#14341,#14342,#14343,#14344,#14345,#14346,#14347,#14348,#14349,#14350,#14351,
#14352,#14353,#14354,#14355,#14356,#14357,#14358,#14359,#14360,#14361,#14362,
#14363,#14364,#14365,#14366,#14367,#14368,#14369,#14370,#14371,#14372,#14373,
#14374,#14375,#14376,#14377,#14378,#14379,#14380,#14381,#14382),
 .UNSPECIFIED.,.F.,.F.,(4,2,2,2,2,2,2,2,2,2,2,2,2,2,2,2,2,2,2,2,2,2,2,2,
2,2,2,2,2,2,2,2,2,2,2,2,2,2,2,4),(-0.662240502390468,-0.657023929679327,
-0.653085195757008,-0.650055270679035,-0.646796302300343,-0.641642298961981,
-0.624849099321322,-0.597369805596174,-0.523035054525191,-0.496396691937766,
-0.492245623831593,-0.490126544756246,-0.488449362968123,-0.486488501472852,
-0.482955170959465,-0.465603944879306,-0.389592518454238,-0.340518345836509,
-0.333343563923072,-0.329643268468981,-0.326711683522161,-0.323450021335688,
-0.320037521603015,-0.308539299509218,-0.250181783322074,-0.176853417000301,
-0.170311927293518,-0.167721023336038,-0.166142277370552,-0.16441218979227,
-0.161935838127768,-0.155636135072824,-0.12373585073483,-0.0337146530897698,
-0.023749165330492,-0.0122727340884673,-0.0077672268730303,-0.004928086174024,
-0.00247151203102761,-0.000962250865292755),.UNSPECIFIED.);
#172=B_SPLINE_CURVE_WITH_KNOTS('',3,(#14383,#14384,#14385,#14386,#14387,
#14388,#14389,#14390,#14391,#14392,#14393,#14394,#14395,#14396,#14397,#14398,
#14399,#14400,#14401,#14402,#14403,#14404,#14405,#14406,#14407,#14408,#14409,
#14410,#14411,#14412,#14413,#14414,#14415,#14416,#14417,#14418,#14419,#14420,
#14421,#14422,#14423,#14424,#14425,#14426,#14427,#14428,#14429,#14430,#14431,
#14432,#14433,#14434,#14435,#14436,#14437,#14438,#14439,#14440,#14441,#14442,
#14443,#14444,#14445,#14446,#14447,#14448,#14449,#14450,#14451,#14452,#14453,
#14454,#14455,#14456,#14457,#14458,#14459,#14460,#14461,#14462,#14463,#14464,
#14465,#14466,#14467,#14468,#14469,#14470,#14471,#14472,#14473,#14474,#14475,
#14476,#14477,#14478,#14479,#14480,#14481,#14482,#14483,#14484,#14485,#14486,
#14487,#14488,#14489,#14490,#14491,#14492,#14493,#14494,#14495,#14496,#14497,
#14498,#14499,#14500,#14501,#14502,#14503,#14504,#14505,#14506,#14507,#14508,
#14509,#14510,#14511,#14512,#14513,#14514,#14515,#14516,#14517,#14518,#14519,
#14520,#14521,#14522,#14523,#14524,#14525,#14526,#14527,#14528,#14529,#14530,
#14531,#14532,#14533,#14534,#14535,#14536,#14537,#14538,#14539,#14540,#14541,
#14542,#14543,#14544,#14545,#14546,#14547,#14548,#14549,#14550,#14551,#14552,
#14553,#14554,#14555,#14556,#14557,#14558,#14559,#14560,#14561,#14562,#14563,
#14564),.UNSPECIFIED.,.F.,.F.,(4,2,2,2,2,2,2,2,2,2,2,2,2,2,2,2,2,2,2,2,
2,2,2,2,2,2,2,2,2,2,2,2,2,2,2,2,2,2,2,2,2,2,2,2,2,2,2,2,2,2,2,2,2,2,2,2,
2,2,2,2,2,2,2,2,2,2,2,2,2,2,2,2,2,2,2,2,2,2,2,2,2,2,2,2,2,2,2,2,2,2,4),
(-4.06006550870592,-4.0592979539179,-4.05690831414429,-4.04988864926168,
-4.00079261892183,-3.92311550633048,-3.90791900336471,-3.90452337110743,
-3.90259317387311,-3.90091311683915,-3.89875240228628,-3.89425010106067,
-3.85281521416176,-3.79516080279116,-3.75651367782774,-3.74724431336817,
-3.74323583404368,-3.74313274029429,-3.74303270359105,-3.74293529208593,
-3.74284007719896,-3.74274662742569,-3.74265450090998,-3.74256323630275,
-3.74247234116765,-3.74238127681489,-3.74228943786694,-3.74219612378574,
-3.74210049780654,-3.74200152542122,-3.74189787807022,-3.74178777431335,
-3.74166870048804,-3.74153687676995,-3.74141647185602,-3.73854358165865,
-3.73484440097036,-3.72767081526953,-3.6786148649635,-3.60262224632263,
-3.58523119680468,-3.58169640628854,-3.57973566424315,-3.57805914823915,
-3.57594164255294,-3.57179583430777,-3.54526655032527,-3.47087245667017,
-3.44343455577428,-3.42665932795555,-3.4215084437827,-3.41825088115425,
-3.41522187038504,-3.41128376470012,-3.40468812234878,-3.35543216565346,
-3.27903782638549,-3.2621901185483,-3.25868756521093,-3.25673377981595,
-3.25505645985484,-3.25292926179518,-3.24873839710274,-3.22091943381247,
-3.14818227289282,-3.12055035179458,-3.10369004703682,-3.09852959671027,
-3.09526980055343,-3.0922413471849,-3.08830770720035,-3.08172778999415,
-3.03258070930082,-2.95645870697833,-2.93923310378528,-2.93570775579726,
-2.93374893395435,-2.93207202140456,-2.92995140406656,-2.92579170429336,
-2.89888776713552,-2.82498254972042,-2.79747486259023,-2.78066855746512,
-2.77551386788707,-2.77225522429316,-2.76922612439584,-2.76528920487724,
-2.75869842201576,-2.70901924957822,-2.69160338547236),.UNSPECIFIED.);
#173=B_SPLINE_CURVE_WITH_KNOTS('',3,(#14570,#14571,#14572,#14573,#14574,
#14575,#14576,#14577,#14578,#14579,#14580,#14581,#14582,#14583,#14584,#14585,
#14586,#14587,#14588,#14589,#14590,#14591,#14592,#14593,#14594,#14595,#14596,
#14597,#14598,#14599,#14600,#14601,#14602,#14603,#14604,#14605,#14606,#14607,
#14608,#14609,#14610,#14611,#14612,#14613,#14614,#14615,#14616,#14617,#14618,
#14619,#14620,#14621,#14622,#14623,#14624,#14625,#14626,#14627,#14628,#14629,
#14630,#14631,#14632,#14633,#14634,#14635,#14636,#14637,#14638,#14639,#14640,
#14641,#14642,#14643,#14644,#14645,#14646,#14647,#14648,#14649,#14650,#14651,
#14652,#14653,#14654,#14655,#14656,#14657,#14658,#14659,#14660,#14661,#14662,
#14663,#14664,#14665,#14666,#14667,#14668,#14669,#14670,#14671,#14672,#14673,
#14674,#14675,#14676,#14677,#14678,#14679,#14680,#14681,#14682,#14683,#14684,
#14685,#14686,#14687,#14688,#14689,#14690,#14691,#14692,#14693,#14694,#14695,
#14696,#14697,#14698,#14699,#14700,#14701,#14702,#14703,#14704,#14705,#14706,
#14707,#14708,#14709,#14710,#14711,#14712,#14713,#14714,#14715,#14716,#14717,
#14718,#14719,#14720,#14721,#14722,#14723,#14724,#14725),.UNSPECIFIED.,
 .F.,.F.,(4,2,2,2,2,2,2,2,2,2,2,2,2,2,2,2,2,2,2,2,2,2,2,2,2,2,2,2,2,2,2,
2,2,2,2,2,2,2,2,2,2,2,2,2,2,2,2,2,2,2,2,2,2,2,2,2,2,2,2,2,2,2,2,2,2,2,2,
2,2,2,2,2,2,2,2,2,2,4),(-1.36992615419562,-1.29786960198346,-1.27000623472678,
-1.2658121564844,-1.26368361046342,-1.26200536880233,-1.26005062826733,
-1.25654664849401,-1.23969626482832,-1.16329957818781,-1.1140614775962,
-1.10747762566089,-1.10354179120432,-1.10051174888973,-1.09725033664901,
-1.09208751607606,-1.07522100961626,-1.04757535235962,-0.974790884145844,
-0.946951072229813,-0.942757767494469,-0.940629385759145,-0.938951156192367,
-0.936996294856674,-0.933491763576773,-0.916632318306228,-0.8402423289104,
-0.791007413912739,-0.784423623193408,-0.780487805690802,-0.777457764946563,
-0.77419634308704,-0.769033483182266,-0.752166632294715,-0.724520190387477,
-0.651743874951846,-0.623897137704172,-0.619703790814916,-0.617575399580141,
-0.615897168643255,-0.613942312741393,-0.61043780866106,-0.593578828407068,
-0.517188456225025,-0.467953353339218,-0.461369556521858,-0.457433736398397,
-0.454403694235402,-0.451142271438742,-0.445979411307835,-0.429112570946092,
-0.401466157773912,-0.357735009114619,-0.30112070793025,-0.296719915350321,
-0.294578338139885,-0.292899088590012,-0.292892478182276,-0.292885973240311,
-0.292879571660865,-0.292873271404119,-0.292867070494959,-0.292860966976924,
-0.290939922527024,-0.28760362101891,-0.283428771869717,-0.27463130011459,
-0.248962733052717,-0.186448793622971,-0.144654555862752,-0.138251386563788,
-0.13436852232334,-0.131346504133501,-0.128060943473425,-0.122788705748904,
-0.104897435176136,-0.0748538664662228,-0.0009633702098371),
 .UNSPECIFIED.);
#174=B_SPLINE_CURVE_WITH_KNOTS('',3,(#14726,#14727,#14728,#14729,#14730,
#14731,#14732,#14733,#14734,#14735,#14736,#14737,#14738,#14739,#14740,#14741,
#14742,#14743,#14744,#14745,#14746,#14747,#14748,#14749,#14750,#14751,#14752,
#14753,#14754,#14755,#14756,#14757,#14758,#14759,#14760,#14761,#14762,#14763,
#14764,#14765,#14766,#14767,#14768,#14769,#14770,#14771,#14772,#14773,#14774,
#14775,#14776,#14777,#14778,#14779,#14780,#14781,#14782,#14783,#14784,#14785,
#14786,#14787,#14788,#14789,#14790,#14791,#14792,#14793,#14794,#14795,#14796,
#14797,#14798,#14799,#14800,#14801,#14802,#14803,#14804,#14805,#14806,#14807,
#14808,#14809,#14810,#14811,#14812,#14813,#14814,#14815),.UNSPECIFIED.,
 .F.,.F.,(4,2,2,2,2,2,2,2,2,2,2,2,2,2,2,2,2,2,2,2,2,2,2,2,2,2,2,2,2,2,2,
2,2,2,2,2,2,2,2,2,2,2,2,2,4),(-4.06063762530162,-4.03738770533439,-4.03445526959851,
-4.03250078196954,-4.03091014967505,-4.02923446840462,-4.02713968381193,
-4.02386997406795,-4.00790352707352,-3.99522786418767,-3.92512436701015,
-3.89564592231692,-3.87799147570487,-3.87274461236604,-3.86946504639217,
-3.86644189698296,-3.86254831866582,-3.85610745447437,-3.81293127607245,
-3.75042378113196,-3.72575725523217,-3.71718896198902,-3.71309254312229,
-3.709780503098,-3.70787879974509,-3.70787380863913,-3.70786878904772,-3.70786374080227,
-3.70785866372855,-3.70785355758587,-3.70617268426424,-3.70401080379363,
-3.69950564525158,-3.65768203768179,-3.59939529228445,-3.57176226710138,
-3.55490021929956,-3.54973839915619,-3.54647752275402,-3.54344791093525,
-3.53951253812888,-3.53292919354584,-3.48369066638352,-3.40728760675519,
-3.39991588284246),.UNSPECIFIED.);
#175=B_SPLINE_CURVE_WITH_KNOTS('',3,(#14816,#14817,#14818,#14819,#14820,
#14821,#14822,#14823,#14824,#14825,#14826,#14827,#14828,#14829,#14830,#14831,
#14832,#14833,#14834,#14835,#14836,#14837,#14838,#14839,#14840,#14841,#14842,
#14843,#14844,#14845,#14846,#14847,#14848,#14849,#14850,#14851,#14852,#14853,
#14854,#14855,#14856,#14857,#14858,#14859,#14860,#14861,#14862,#14863,#14864,
#14865,#14866,#14867,#14868,#14869,#14870,#14871,#14872,#14873,#14874,#14875,
#14876,#14877,#14878,#14879,#14880,#14881,#14882,#14883,#14884,#14885,#14886,
#14887,#14888,#14889,#14890,#14891,#14892,#14893,#14894,#14895,#14896,#14897,
#14898,#14899,#14900,#14901,#14902,#14903,#14904,#14905,#14906,#14907,#14908,
#14909,#14910,#14911,#14912,#14913,#14914,#14915,#14916,#14917,#14918,#14919,
#14920,#14921,#14922,#14923,#14924,#14925,#14926,#14927,#14928,#14929,#14930,
#14931,#14932,#14933,#14934,#14935,#14936,#14937,#14938,#14939,#14940,#14941,
#14942,#14943,#14944,#14945,#14946,#14947,#14948,#14949,#14950,#14951,#14952,
#14953,#14954,#14955,#14956,#14957,#14958,#14959,#14960,#14961,#14962,#14963,
#14964,#14965,#14966,#14967,#14968,#14969,#14970,#14971,#14972,#14973,#14974,
#14975,#14976,#14977,#14978,#14979,#14980,#14981,#14982,#14983,#14984,#14985,
#14986,#14987,#14988,#14989,#14990,#14991,#14992,#14993,#14994,#14995,#14996,
#14997,#14998,#14999,#15000,#15001,#15002,#15003,#15004,#15005,#15006,#15007,
#15008,#15009,#15010,#15011,#15012,#15013,#15014,#15015,#15016,#15017,#15018,
#15019,#15020,#15021,#15022,#15023,#15024,#15025,#15026,#15027,#15028,#15029,
#15030,#15031,#15032,#15033,#15034,#15035,#15036,#15037,#15038,#15039,#15040,
#15041),.UNSPECIFIED.,.F.,.F.,(4,2,2,2,2,2,2,2,2,2,2,2,2,2,2,2,2,2,2,2,
2,2,2,2,2,2,2,2,2,2,2,2,2,2,2,2,2,2,2,2,2,2,2,2,2,2,2,2,2,2,2,2,2,2,2,2,
2,2,2,2,2,2,2,2,2,2,2,2,2,2,2,2,2,2,2,2,2,2,2,2,2,2,2,2,2,2,2,2,2,2,2,2,
2,2,2,2,2,2,2,2,2,2,2,2,2,2,2,2,2,2,2,2,4),(-2.69160338547236,-2.63169763039443,
-2.61603620327971,-2.6126086148271,-2.61067108797478,-2.60899156713524,
-2.60684056011834,-2.60338555899897,-2.58434312529108,-2.57435193343334,
-2.50224056241301,-2.47454852745384,-2.45766141641091,-2.45249761626397,
-2.44923682113843,-2.44620821005473,-2.44227545821738,-2.4356994332569,
-2.38677994524135,-2.31108733551206,-2.29324310216633,-2.28968164861194,
-2.28771483513348,-2.28603843603407,-2.28392784197441,-2.27981558166157,
-2.25419228103839,-2.17815034654899,-2.15113320638569,-2.13454176865548,
-2.12941052990453,-2.12615680590718,-2.12312540723192,-2.11917569807003,
-2.11254179305805,-2.06060314336006,-2.0302492262792,-1.975946280875,-1.96861215431759,
-1.96589664490868,-1.96429404515234,-1.96258319875142,-1.96020902120597,
-1.954535131085,-1.92842248779088,-1.86059325504999,-1.81529831746807,-1.80880298356115,
-1.80489372650911,-1.80186862656731,-1.7985971393049,-1.79338528459779,
-1.77605625035436,-1.74733766376055,-1.70462100284471,-1.64863944958662,
-1.64423085205556,-1.64208817429198,-1.64040935585446,-1.6384660221207,
-1.63501212653966,-1.61894821253835,-1.54198442551393,-1.49244918587806,
-1.48586115261748,-1.48192487853785,-1.47889571040262,-1.47563643902858,
-1.47047957836215,-1.45365584825761,-1.42610503732193,-1.35238242333136,
-1.32529198141123,-1.32112526146239,-1.31900302705165,-1.3173258530745,
-1.31536788739084,-1.31184700577633,-1.29469998304932,-1.21855437731766,
-1.16939216187519,-1.16281153069785,-1.15887740574886,-1.15584856249118,
-1.15258833187219,-1.14742716450561,-1.13056442768403,-1.10292431826243,
-1.03004854267861,-1.00228710228514,-0.998097491470576,-0.995970370025444,
-0.9942928239992,-0.992338434980571,-0.988833973630052,-0.971960456269705,
-0.895613419525241,-0.846352700140486,-0.839770092228908,-0.835835388658402,
-0.832806452472319,-0.829546469028812,-0.824386432930255,-0.807534018756594,
-0.779917579449145,-0.706800711878549,-0.679232755252589,-0.675049604754214,
-0.6729238583611,-0.671246415025316,-0.669291016990579,-0.665781938503568,
-0.661808055719697),.UNSPECIFIED.);
#176=B_SPLINE_CURVE_WITH_KNOTS('',3,(#15046,#15047,#15048,#15049,#15050,
#15051,#15052,#15053,#15054,#15055,#15056,#15057,#15058,#15059,#15060,#15061,
#15062,#15063,#15064,#15065,#15066,#15067,#15068,#15069,#15070,#15071,#15072,
#15073,#15074,#15075,#15076,#15077,#15078,#15079,#15080,#15081,#15082,#15083,
#15084,#15085,#15086,#15087,#15088,#15089,#15090,#15091,#15092,#15093,#15094,
#15095,#15096,#15097,#15098,#15099,#15100,#15101,#15102,#15103,#15104,#15105,
#15106,#15107,#15108,#15109,#15110,#15111,#15112,#15113,#15114,#15115,#15116,
#15117,#15118,#15119,#15120,#15121,#15122,#15123,#15124,#15125,#15126,#15127,
#15128,#15129,#15130,#15131,#15132,#15133,#15134,#15135,#15136,#15137,#15138,
#15139,#15140,#15141,#15142,#15143,#15144,#15145,#15146,#15147,#15148,#15149,
#15150,#15151,#15152,#15153,#15154,#15155,#15156,#15157,#15158,#15159,#15160,
#15161,#15162,#15163,#15164,#15165,#15166,#15167,#15168,#15169,#15170,#15171,
#15172,#15173,#15174,#15175,#15176,#15177,#15178,#15179,#15180,#15181,#15182,
#15183,#15184,#15185,#15186,#15187,#15188,#15189,#15190,#15191,#15192,#15193,
#15194,#15195,#15196,#15197,#15198,#15199,#15200,#15201,#15202,#15203,#15204,
#15205,#15206,#15207,#15208,#15209,#15210,#15211,#15212,#15213,#15214,#15215,
#15216,#15217,#15218,#15219,#15220,#15221,#15222,#15223,#15224,#15225,#15226,
#15227,#15228,#15229,#15230,#15231,#15232,#15233,#15234,#15235,#15236,#15237,
#15238,#15239,#15240,#15241,#15242,#15243,#15244,#15245,#15246,#15247,#15248,
#15249,#15250,#15251,#15252,#15253,#15254,#15255,#15256,#15257,#15258,#15259,
#15260,#15261,#15262,#15263,#15264,#15265,#15266,#15267,#15268,#15269,#15270,
#15271,#15272,#15273,#15274,#15275,#15276,#15277),.UNSPECIFIED.,.F.,.F.,
(4,2,2,2,2,2,2,2,2,2,2,2,2,2,2,2,2,2,2,2,2,2,2,2,2,2,2,2,2,2,2,2,2,2,2,
2,2,2,2,2,2,2,2,2,2,2,2,2,2,2,2,2,2,2,2,2,2,2,2,2,2,2,2,2,2,2,2,2,2,2,2,
2,2,2,2,2,2,2,2,2,2,2,2,2,2,2,2,2,2,2,2,2,2,2,2,2,2,2,2,2,2,2,2,2,2,2,2,
2,2,2,2,2,2,2,2,4),(-3.39970068703626,-3.38822341450344,-3.37147224508822,
-3.36632248943194,-3.36306416816673,-3.36003342691036,-3.35609160446387,
-3.34948647033446,-3.29976259537378,-3.22214765718618,-3.20681025573698,
-3.20340356533925,-3.20147020024205,-3.19978937757082,-3.19763024820342,
-3.19314012417513,-3.15469551958324,-3.09608666142328,-3.06641567919309,
-3.04867903176444,-3.04342293528804,-3.04014094686719,-3.03711782984798,
-3.03322745010955,-3.02679868926118,-2.98409455781559,-2.9221363862561,
-2.89670505813259,-2.88354629257996,-2.88030061337599,-2.87840278215447,
-2.87671535732535,-2.87453456777442,-2.87090308380529,-2.84834499806466,
-2.84152974728029,-2.77016756950921,-2.72839145468897,-2.72164869208634,
-2.71804209643894,-2.7150805448175,-2.71158648043496,-2.70553332989776,
-2.68114216087857,-2.66895089149459,-2.60260511242225,-2.57465929545017,
-2.56066125965985,-2.55735023382665,-2.5554379177877,-2.55375349146361,
-2.55159693740608,-2.54804776866578,-2.52719625669397,-2.45410663409195,
-2.40571028839893,-2.39876675791672,-2.39511794686555,-2.39241538267134,
-2.38904782324688,-2.38340527241454,-2.36411630727703,-2.27772581888842,
-2.25108164116281,-2.23751202712445,-2.23423365472209,-2.23232848841202,
-2.23064250068112,-2.22847382980477,-2.22488384927387,-2.20319614940122,
-2.18702461353068,-2.10477793037042,-2.08063460603756,-2.07480929135583,
-2.0714012544123,-2.06840411055488,-2.06467272335975,-2.05890804313187,
-2.0307786704277,-1.96685490333648,-1.94420771690159,-1.9161254167198,-1.91192421517328,
-1.90979415316076,-1.90811579447316,-1.90616215509294,-1.90266321770517,
-1.88589553381497,-1.80943727698247,-1.76017008038009,-1.75358565287927,
-1.74964965273988,-1.74661958715082,-1.74335825256084,-1.73819577380495,
-1.72133234459799,-1.69369372928755,-1.62083562102662,-1.59305541313776,
-1.58886407900056,-1.58673611822124,-1.58505792246039,-1.58310275800837,
-1.57959683243826,-1.56271437411727,-1.4863415447981,-1.43711483893621,
-1.43053121675512,-1.4265954499599,-1.42356541899705,-1.42030397884951,
-1.41514102857145,-1.3982733321828,-1.37062494350533,-1.36992615419562),
 .UNSPECIFIED.);
#177=B_SPLINE_CURVE_WITH_KNOTS('',3,(#15279,#15280,#15281,#15282,#15283,
#15284,#15285,#15286,#15287,#15288,#15289,#15290,#15291,#15292,#15293,#15294,
#15295,#15296,#15297,#15298,#15299,#15300,#15301,#15302,#15303,#15304,#15305,
#15306,#15307,#15308,#15309,#15310,#15311,#15312,#15313,#15314,#15315,#15316,
#15317,#15318,#15319,#15320,#15321,#15322,#15323,#15324,#15325,#15326,#15327,
#15328,#15329,#15330,#15331,#15332,#15333,#15334,#15335,#15336,#15337,#15338,
#15339,#15340,#15341,#15342,#15343,#15344,#15345,#15346,#15347,#15348,#15349,
#15350,#15351,#15352,#15353,#15354,#15355,#15356,#15357,#15358,#15359,#15360,
#15361,#15362,#15363,#15364,#15365,#15366,#15367,#15368,#15369,#15370,#15371,
#15372,#15373,#15374,#15375,#15376,#15377,#15378,#15379,#15380,#15381,#15382,
#15383,#15384,#15385,#15386),.UNSPECIFIED.,.F.,.F.,(4,2,2,2,2,2,2,2,2,2,
2,2,2,2,2,2,2,2,2,2,2,2,2,2,2,2,2,2,2,2,2,2,2,2,2,2,2,2,2,2,2,2,2,2,2,2,
2,2,2,2,2,2,2,4),(-0.661808055719697,-0.648832150577172,-0.572541433096579,
-0.523307773563162,-0.516725694804676,-0.512791141391924,-0.509762223683841,
-0.506502164486976,-0.501341804656795,-0.484486508268001,-0.456863486888756,
-0.389214614274023,-0.356439867090687,-0.352056010808638,-0.349918244540708,
-0.348321158104792,-0.348315809881205,-0.348310492428431,-0.34830520551964,
-0.348299948981064,-0.348294722610798,-0.348289526212797,-0.348284359534354,
-0.348279222357803,-0.348274114517763,-0.348269035862146,-0.348263986144369,
-0.348258965155043,-0.348253972718448,-0.346351750232364,-0.343031734571514,
-0.33892635730641,-0.330331700068644,-0.305551107034789,-0.243159137770574,
-0.200065231136631,-0.193627565821907,-0.189735279233183,-0.18671277699546,
-0.183433564530137,-0.178186525865762,-0.160525001770526,-0.131024497779064,
-0.0548895685140513,-0.0425981494905788,-0.0418966775377889,-0.0313058078813465,
-0.028166581753517,-0.0262927986908994,-0.0246670930059718,-0.0230104890773531,
-0.0208364519660099,-0.017373362411351,-0.000961441519558661),
 .UNSPECIFIED.);
#178=B_SPLINE_CURVE_WITH_KNOTS('',3,(#15387,#15388,#15389,#15390,#15391,
#15392,#15393,#15394,#15395,#15396,#15397,#15398,#15399,#15400,#15401,#15402,
#15403,#15404,#15405,#15406,#15407,#15408,#15409,#15410,#15411,#15412,#15413,
#15414,#15415,#15416,#15417,#15418,#15419,#15420,#15421,#15422,#15423,#15424,
#15425,#15426,#15427,#15428,#15429,#15430,#15431,#15432,#15433,#15434,#15435,
#15436,#15437,#15438,#15439,#15440,#15441,#15442,#15443,#15444,#15445,#15446,
#15447,#15448,#15449,#15450,#15451,#15452,#15453,#15454,#15455,#15456,#15457,
#15458,#15459,#15460,#15461,#15462,#15463,#15464,#15465,#15466,#15467,#15468,
#15469,#15470,#15471,#15472,#15473,#15474,#15475,#15476,#15477,#15478,#15479,
#15480,#15481,#15482,#15483,#15484,#15485,#15486,#15487,#15488,#15489,#15490,
#15491,#15492,#15493,#15494,#15495,#15496,#15497,#15498,#15499,#15500,#15501,
#15502,#15503,#15504,#15505,#15506,#15507,#15508,#15509,#15510,#15511,#15512,
#15513,#15514,#15515,#15516,#15517,#15518,#15519,#15520,#15521,#15522,#15523,
#15524,#15525,#15526,#15527,#15528,#15529,#15530),.UNSPECIFIED.,.F.,.F.,
(4,2,2,2,2,2,2,2,2,2,2,2,2,2,2,2,2,2,2,2,2,2,2,2,2,2,2,2,2,2,2,2,2,2,2,
2,2,2,2,2,2,2,2,2,2,2,2,2,2,2,2,2,2,2,2,2,2,2,2,2,2,2,2,2,2,2,2,2,2,2,2,
4),(-4.06154323901497,-3.97971723338825,-3.9409087536146,-3.93161870694837,
-3.92751754463492,-3.92447353549115,-3.92163907437441,-3.91774791945187,
-3.90787067438528,-3.82027383305999,-3.80171307894705,-3.78045720960814,
-3.77270265519819,-3.76888882502671,-3.76579087781818,-3.76392446850604,
-3.76231566211645,-3.76015547690693,-3.75565646608519,-3.71467064316284,
-3.65549872007339,-3.62789111064862,-3.61104151951261,-3.60588231837622,
-3.60262284349152,-3.5995943657568,-3.59566023580679,-3.58907848922892,
-3.53983382886483,-3.46351440828317,-3.44656104949759,-3.44305200892795,
-3.4410967641527,-3.43941952734521,-3.4372941512235,-3.43311205032648,-3.40557409353817,
-3.33248391660804,-3.30488540748622,-3.28803950890903,-3.28288052085286,
-3.2796209690648,-3.27659227388823,-3.27265765418958,-3.26607463149876,
-3.21678235585174,-3.14036513428093,-3.12353665298247,-3.12003502926618,
-3.11808133182462,-3.11640382041477,-3.11427603619539,-3.11008297947165,
-3.08220694854588,-3.00952993261914,-2.98188901256543,-2.96502431710805,
-2.95986306452819,-2.95660288634488,-2.95357416412611,-2.94964029708805,
-2.94306026915623,-2.89393466180563,-2.81785675018311,-2.80055843400905,
-2.79702855490374,-2.79506863194744,-2.79339164691385,-2.79127205197907,
-2.78711768670855,-2.76037130570713,-2.69271526571019),.UNSPECIFIED.);
#179=B_SPLINE_CURVE_WITH_KNOTS('',3,(#15536,#15537,#15538,#15539,#15540,
#15541,#15542,#15543,#15544,#15545,#15546,#15547,#15548,#15549,#15550,#15551,
#15552,#15553,#15554,#15555,#15556,#15557,#15558,#15559,#15560,#15561,#15562,
#15563,#15564,#15565,#15566,#15567,#15568,#15569,#15570,#15571,#15572,#15573,
#15574,#15575,#15576,#15577,#15578,#15579,#15580,#15581,#15582,#15583,#15584,
#15585,#15586,#15587,#15588,#15589,#15590,#15591,#15592,#15593,#15594,#15595,
#15596,#15597,#15598,#15599,#15600,#15601,#15602,#15603,#15604,#15605,#15606,
#15607,#15608,#15609,#15610,#15611,#15612,#15613,#15614,#15615,#15616,#15617,
#15618,#15619,#15620,#15621,#15622,#15623,#15624,#15625,#15626,#15627,#15628,
#15629,#15630,#15631,#15632,#15633,#15634,#15635,#15636,#15637,#15638,#15639,
#15640,#15641,#15642,#15643,#15644,#15645,#15646,#15647,#15648,#15649,#15650,
#15651,#15652,#15653,#15654,#15655,#15656,#15657,#15658,#15659,#15660,#15661,
#15662,#15663,#15664,#15665,#15666,#15667,#15668,#15669,#15670,#15671,#15672,
#15673,#15674,#15675,#15676,#15677),.UNSPECIFIED.,.F.,.F.,(4,2,2,2,2,2,
2,2,2,2,2,2,2,2,2,2,2,2,2,2,2,2,2,2,2,2,2,2,2,2,2,2,2,2,2,2,2,2,2,2,2,2,
2,2,2,2,2,2,2,2,2,2,2,2,2,2,2,2,2,2,2,2,2,2,2,2,2,2,2,2,4),(-1.36961882394012,
-1.30315593555376,-1.25364920307832,-1.24705976090669,-1.24312220915139,
-1.24009179395163,-1.2368309148216,-1.23167092891767,-1.21483149344873,
-1.18724833492873,-1.11382929870891,-1.08649270731871,-1.08231619034621,
-1.08019133305969,-1.07851330353662,-1.07655570765878,-1.07303888099454,
-1.05597737726654,-0.979732518490505,-0.930567441324095,-0.923984792423174,
-0.920049215438583,-0.917019101398693,-0.913757346043541,-0.908593415447113,
-0.891718202841784,-0.864053095476609,-0.791461329552479,-0.763460987737648,
-0.759262283343022,-0.75713269499197,-0.755454302435665,-0.753500156353745,
-0.749999152986304,-0.733199537098949,-0.656760944098597,-0.607501131360064,
-0.6009173033429,-0.596981383293664,-0.59395121668842,-0.590689613147879,
-0.585526367143234,-0.568657372482014,-0.541006517204668,-0.46826047777152,
-0.440385557689011,-0.436190948455384,-0.434062232241406,-0.432383907460957,
-0.430429128763035,-0.426925226197747,-0.410077998389506,-0.333674856318948,
-0.284452516327641,-0.277857575520124,-0.273918413492927,-0.270887737321598,
-0.268085403544718,-0.26354363846413,-0.251056102059236,-0.232524046960948,
-0.196005841666166,-0.120601370192909,-0.114217157975272,-0.111652348357135,
-0.110078217528788,-0.10834273572402,-0.105840673203071,-0.0993779921424752,
-0.0658658239895591,-0.000963213376137151),.UNSPECIFIED.);
#180=B_SPLINE_CURVE_WITH_KNOTS('',3,(#15678,#15679,#15680,#15681,#15682,
#15683,#15684,#15685,#15686,#15687,#15688,#15689,#15690,#15691,#15692,#15693,
#15694,#15695,#15696,#15697,#15698,#15699,#15700,#15701,#15702,#15703,#15704,
#15705,#15706,#15707,#15708,#15709,#15710,#15711,#15712,#15713,#15714,#15715,
#15716,#15717,#15718,#15719,#15720,#15721,#15722,#15723,#15724,#15725,#15726,
#15727,#15728,#15729,#15730,#15731,#15732,#15733,#15734,#15735,#15736,#15737,
#15738,#15739,#15740,#15741,#15742,#15743,#15744,#15745,#15746,#15747,#15748,
#15749,#15750,#15751,#15752,#15753,#15754,#15755,#15756,#15757,#15758,#15759),
 .UNSPECIFIED.,.F.,.F.,(4,2,2,2,2,2,2,2,2,2,2,2,2,2,2,2,2,2,2,2,2,2,2,2,
2,2,2,2,2,2,2,2,2,2,2,2,2,2,2,2,4),(-4.06102161170475,-4.02199582972615,
-4.01663778008757,-4.01308748452359,-4.01022730211651,-4.00752733239566,
-4.00414887591018,-3.99845407020849,-3.97865998740159,-3.96660944868934,
-3.94585223754946,-3.86808864668337,-3.85295615226867,-3.84956401701976,
-3.84763412207103,-3.84595323132078,-3.84378997006057,-3.83927720957401,
-3.79651224000436,-3.7414405954293,-3.71233471562289,-3.70074635282836,
-3.69208785735269,-3.68811704164995,-3.68526437890688,-3.68244780870993,
-3.67789828083094,-3.66671097613844,-3.6641851664845,-3.55730709132919,
-3.53944397463258,-3.53255799146753,-3.52750558145803,-3.52524014707967,
-3.5235463740722,-3.5216733201392,-3.51853886765252,-3.5079953174975,-3.50579466494038,
-3.41560235753592,-3.39970068703626),.UNSPECIFIED.);
#181=B_SPLINE_CURVE_WITH_KNOTS('',3,(#15760,#15761,#15762,#15763,#15764,
#15765,#15766,#15767,#15768,#15769,#15770,#15771,#15772,#15773,#15774,#15775,
#15776,#15777,#15778,#15779,#15780,#15781,#15782,#15783,#15784,#15785,#15786,
#15787,#15788,#15789,#15790,#15791,#15792,#15793,#15794,#15795,#15796,#15797,
#15798,#15799,#15800,#15801,#15802,#15803,#15804,#15805,#15806,#15807,#15808,
#15809,#15810,#15811,#15812,#15813,#15814,#15815,#15816,#15817,#15818,#15819,
#15820,#15821,#15822,#15823,#15824,#15825,#15826,#15827,#15828,#15829,#15830,
#15831,#15832,#15833,#15834,#15835,#15836,#15837,#15838,#15839,#15840,#15841,
#15842,#15843,#15844,#15845,#15846,#15847,#15848,#15849,#15850,#15851,#15852,
#15853,#15854,#15855,#15856,#15857,#15858,#15859,#15860,#15861,#15862,#15863,
#15864,#15865,#15866,#15867,#15868,#15869,#15870,#15871,#15872,#15873,#15874,
#15875,#15876,#15877,#15878,#15879,#15880,#15881,#15882,#15883,#15884,#15885,
#15886,#15887,#15888,#15889,#15890,#15891,#15892,#15893,#15894,#15895,#15896,
#15897,#15898,#15899,#15900,#15901,#15902,#15903,#15904,#15905,#15906,#15907,
#15908,#15909,#15910,#15911,#15912,#15913,#15914,#15915,#15916,#15917,#15918,
#15919,#15920,#15921,#15922,#15923,#15924,#15925,#15926,#15927,#15928,#15929,
#15930,#15931,#15932,#15933,#15934,#15935,#15936,#15937,#15938,#15939,#15940,
#15941,#15942,#15943,#15944,#15945,#15946,#15947,#15948,#15949,#15950,#15951,
#15952,#15953,#15954,#15955,#15956,#15957,#15958,#15959,#15960,#15961,#15962,
#15963,#15964,#15965,#15966,#15967,#15968,#15969,#15970,#15971,#15972,#15973,
#15974,#15975,#15976,#15977,#15978,#15979,#15980,#15981,#15982,#15983,#15984,
#15985,#15986,#15987),.UNSPECIFIED.,.F.,.F.,(4,2,2,2,2,2,2,2,2,2,2,2,2,
2,2,2,2,2,2,2,2,2,2,2,2,2,2,2,2,2,2,2,2,2,2,2,2,2,2,2,2,2,2,2,2,2,2,2,2,
2,2,2,2,2,2,2,2,2,2,2,2,2,2,2,2,2,2,2,2,2,2,2,2,2,2,2,2,2,2,2,2,2,2,2,2,
2,2,2,2,2,2,2,2,2,2,2,2,2,2,2,2,2,2,2,2,2,2,2,2,2,2,2,2,4),(-2.69271526571019,
-2.68624721463361,-2.65876402825057,-2.64196798111432,-2.63681410617141,
-2.63355543861204,-2.63052594401115,-2.62658798210346,-2.6199942861044,
-2.57019414145632,-2.4925494406474,-2.47727445615202,-2.47387261079431,
-2.47194062244171,-2.47026012526584,-2.46810030952158,-2.46461647622999,
-2.44503892072068,-2.4401978299325,-2.43135039808765,-2.36099685825411,
-2.32523145639768,-2.31633787189987,-2.31230745805228,-2.30927405643316,
-2.30602496996308,-2.30091535062292,-2.28602584244716,-2.18138882295176,
-2.16360151354676,-2.15673574234555,-2.15169498153557,-2.1494317829581,
-2.14773844567741,-2.14586457914324,-2.14272604785922,-2.13214483596618,
-2.12833675454628,-2.03158982424865,-1.99849962339315,-1.99244100403821,
-1.98862018070773,-1.98561497893053,-1.9822646182488,-1.97669766881371,
-1.95571553615086,-1.8748323874128,-1.83271608318859,-1.82820635004418,
-1.826043559173,-1.82436258819426,-1.82243211625727,-1.81903786643855,-1.80387764838228,
-1.7261679426778,-1.67634625841352,-1.66975150667458,-1.66581288820987,
-1.66278289082836,-1.65952368621272,-1.65436897211488,-1.63757045203986,
-1.61007940440053,-1.53582075189944,-1.50912267008506,-1.50496931584516,
-1.50284970165496,-1.50117242468987,-1.49921183084357,-1.49567993431371,
-1.47835473980605,-1.40232125814328,-1.35321389968435,-1.34663328600624,
-1.34269877597881,-1.33966940497848,-1.33640837846621,-1.33124546542001,
-1.31437267194065,-1.28671164011955,-1.2139866990388,-1.18608639192274,
-1.1818915727963,-1.17976310322527,-1.17808516061701,-1.1761310750648,-1.17262905843022,
-1.15580366272312,-1.07940367470053,-1.0301152666782,-1.02353102547234,
-1.01959545674416,-1.01656591951338,-1.01330535314141,-1.00814453066496,
-0.991290768345315,-0.963673362337573,-0.890499311629776,-0.862960415142799,
-0.85877761718957,-0.856651707779826,-0.854973959360891,-0.853018002796683,
-0.849507416817777,-0.832540589674147,-0.756245304467527,-0.70702883626328,
-0.700433528011964,-0.696494726806326,-0.693464676183969,-0.690205500202847,
-0.685051014157872,-0.668254866052211,-0.662349049559275),.UNSPECIFIED.);
#182=B_SPLINE_CURVE_WITH_KNOTS('',3,(#15992,#15993,#15994,#15995,#15996,
#15997,#15998,#15999,#16000,#16001,#16002,#16003,#16004,#16005,#16006,#16007,
#16008,#16009,#16010,#16011,#16012,#16013,#16014,#16015,#16016,#16017,#16018,
#16019,#16020,#16021,#16022,#16023,#16024,#16025,#16026,#16027,#16028,#16029,
#16030,#16031,#16032,#16033,#16034,#16035,#16036,#16037,#16038,#16039,#16040,
#16041,#16042,#16043,#16044,#16045,#16046,#16047,#16048,#16049,#16050,#16051,
#16052,#16053,#16054,#16055,#16056,#16057,#16058,#16059,#16060,#16061,#16062,
#16063,#16064,#16065,#16066,#16067,#16068,#16069,#16070,#16071,#16072,#16073,
#16074,#16075,#16076,#16077,#16078,#16079,#16080,#16081,#16082,#16083,#16084,
#16085,#16086,#16087,#16088,#16089,#16090,#16091,#16092,#16093,#16094,#16095,
#16096,#16097,#16098,#16099,#16100,#16101,#16102,#16103,#16104,#16105,#16106,
#16107,#16108,#16109,#16110,#16111,#16112,#16113,#16114,#16115,#16116,#16117,
#16118,#16119,#16120,#16121,#16122,#16123,#16124,#16125,#16126,#16127,#16128,
#16129,#16130,#16131,#16132,#16133,#16134,#16135,#16136,#16137,#16138,#16139,
#16140,#16141,#16142,#16143,#16144,#16145,#16146,#16147,#16148,#16149,#16150,
#16151,#16152,#16153,#16154,#16155,#16156,#16157,#16158,#16159,#16160,#16161,
#16162,#16163,#16164,#16165,#16166,#16167,#16168,#16169,#16170,#16171,#16172,
#16173,#16174,#16175,#16176,#16177,#16178,#16179,#16180,#16181,#16182,#16183,
#16184,#16185,#16186,#16187,#16188,#16189,#16190,#16191,#16192,#16193,#16194,
#16195,#16196,#16197,#16198,#16199,#16200,#16201,#16202,#16203,#16204,#16205,
#16206,#16207,#16208,#16209,#16210,#16211,#16212,#16213,#16214,#16215,#16216,
#16217,#16218,#16219),.UNSPECIFIED.,.F.,.F.,(4,2,2,2,2,2,2,2,2,2,2,2,2,
2,2,2,2,2,2,2,2,2,2,2,2,2,2,2,2,2,2,2,2,2,2,2,2,2,2,2,2,2,2,2,2,2,2,2,2,
2,2,2,2,2,2,2,2,2,2,2,2,2,2,2,2,2,2,2,2,2,2,2,2,2,2,2,2,2,2,2,2,2,2,2,2,
2,2,2,2,2,2,2,2,2,2,2,2,2,2,2,2,2,2,2,2,2,2,2,2,2,2,2,2,4),(-3.39964083351492,
-3.36365087206928,-3.34678077620974,-3.3432756693511,-3.34132074014372,
-3.33964260244493,-3.3375145426246,-3.33332248596686,-3.30551171339091,
-3.23274707438292,-3.20511715466561,-3.18825585182105,-3.18309369335482,
-3.17983247271473,-3.1768024510124,-3.17286641792817,-3.1662816870958,-3.11700934454949,
-3.04053866167242,-3.02372963752752,-3.02022809592353,-3.01827387292569,
-3.01659554617584,-3.01446622347939,-3.01026858715903,-2.98229350650707,
-2.90972509345195,-2.88207473063289,-2.86520421687862,-2.86004084563294,
-2.85677922902745,-2.85374909486574,-2.84981327827797,-2.84322970839898,
-2.79403246661742,-2.717719295123,-2.70069023416851,-2.69717523709525,-2.69521800906385,
-2.69353988657468,-2.69141439938574,-2.68723509897752,-2.65981606356893,
-2.58654863464378,-2.55896508096669,-2.54212345194394,-2.53696306561767,
-2.5337019839676,-2.53067141446083,-2.52673370839752,-2.52014405970235,
-2.4706577015763,-2.39371343017052,-2.37751324304274,-2.37404934384091,
-2.37210320212424,-2.37042371508873,-2.36828243821504,-2.36388427273072,
-2.3070464387066,-2.26249989183244,-2.23555375468513,-2.218991567172,-2.21386183379691,
-2.2106072771075,-2.20757385386497,-2.20361971358468,-2.1969743579148,-2.13040400241445,
-2.08297340398918,-2.06429494999913,-2.05719346066002,-2.0520176405405,
-2.04972954812474,-2.04803212316265,-2.0461691242003,-2.04308095280988,
-2.03294629747931,-2.03090298239736,-2.00858613066327,-1.91910146310902,
-1.89732612426433,-1.89150265071687,-1.88806124926346,-1.88506732512373,
-1.88138184085324,-1.87426317867405,-1.81790382035216,-1.75704433491111,
-1.73244874736278,-1.72837642684058,-1.72627388458271,-1.72459728666606,
-1.72262251508973,-1.71902685373257,-1.70058567033811,-1.62115250355916,
-1.57650792932064,-1.57002050655558,-1.5661127055394,-1.56308676936036,
-1.55981241672749,-1.55459174376434,-1.53719345280849,-1.50831675095391,
-1.46575548046262,-1.40985460921982,-1.40544316768122,-1.40329937886659,
-1.40161981358235,-1.39967572403598,-1.39622072167918,-1.3801554698927,
-1.36961882394012),.UNSPECIFIED.);
#183=B_SPLINE_CURVE_WITH_KNOTS('',3,(#16221,#16222,#16223,#16224,#16225,
#16226,#16227,#16228,#16229,#16230,#16231,#16232,#16233,#16234,#16235,#16236,
#16237,#16238,#16239,#16240,#16241,#16242,#16243,#16244,#16245,#16246,#16247,
#16248,#16249,#16250,#16251,#16252,#16253,#16254,#16255,#16256,#16257,#16258,
#16259,#16260,#16261,#16262,#16263,#16264,#16265,#16266,#16267,#16268,#16269,
#16270,#16271,#16272,#16273,#16274,#16275,#16276,#16277,#16278,#16279,#16280,
#16281,#16282,#16283,#16284,#16285,#16286,#16287,#16288,#16289,#16290,#16291,
#16292,#16293,#16294,#16295,#16296,#16297,#16298,#16299,#16300,#16301,#16302,
#16303,#16304,#16305,#16306,#16307,#16308,#16309,#16310,#16311,#16312,#16313,
#16314,#16315,#16316,#16317,#16318,#16319,#16320,#16321,#16322,#16323,#16324,
#16325,#16326,#16327,#16328,#16329,#16330,#16331,#16332,#16333,#16334,#16335,
#16336,#16337,#16338,#16339,#16340,#16341,#16342),.UNSPECIFIED.,.F.,.F.,
(4,2,2,2,2,2,2,2,2,2,2,2,2,2,2,2,2,2,2,2,2,2,2,2,2,2,2,2,2,2,2,2,2,2,2,
2,2,2,2,2,2,2,2,2,2,2,2,2,2,2,2,2,2,2,2,2,2,2,2,2,4),(-0.662349049559275,
-0.64076935233397,-0.566466931283648,-0.539800645169952,-0.535648410883396,
-0.533529023672387,-0.53185174726018,-0.529890947402202,-0.526358160710187,
-0.509018246169802,-0.432994462499759,-0.383918563847769,-0.377323282030764,
-0.373384472547141,-0.370354401509297,-0.370298975441233,-0.370234676619521,
-0.370179135744734,-0.370131156433472,-0.370089705560998,-0.370053891319813,
-0.370022944097521,-0.369986958714127,-0.369952150661377,-0.369918477084106,
-0.369885898069153,-0.369854375178348,-0.369823871418894,-0.369794351172866,
-0.369765780142296,-0.369738125323371,-0.369711354947079,-0.369685438411946,
-0.369660348552099,-0.369636059309752,-0.369612539282026,-0.369589762222112,
-0.369567702865705,-0.366116070446883,-0.35999913953825,-0.352470758189602,
-0.336679856203082,-0.289908620168167,-0.221133027376399,-0.213965351312048,
-0.211274959536918,-0.209677145139871,-0.20796274220465,-0.205569383331507,
-0.199782212265901,-0.172671316670112,-0.0998764316644174,-0.0808381187294856,
-0.05849686903062,-0.0526228188635247,-0.0491704671463769,-0.0464777890897304,
-0.0436385767213315,-0.0401730278245112,-0.0350189293278793,-0.000961519009988408),
 .UNSPECIFIED.);
#184=B_SPLINE_CURVE_WITH_KNOTS('',3,(#16343,#16344,#16345,#16346,#16347,
#16348,#16349,#16350,#16351,#16352,#16353,#16354,#16355,#16356,#16357,#16358,
#16359,#16360,#16361,#16362,#16363,#16364,#16365,#16366,#16367,#16368,#16369,
#16370,#16371,#16372,#16373,#16374,#16375,#16376,#16377,#16378,#16379,#16380,
#16381,#16382,#16383,#16384,#16385,#16386,#16387,#16388,#16389,#16390,#16391,
#16392,#16393,#16394,#16395,#16396,#16397,#16398,#16399,#16400,#16401,#16402,
#16403,#16404,#16405,#16406,#16407,#16408,#16409,#16410,#16411,#16412,#16413,
#16414,#16415,#16416,#16417,#16418,#16419,#16420,#16421,#16422,#16423,#16424,
#16425,#16426,#16427,#16428,#16429,#16430,#16431,#16432,#16433,#16434,#16435,
#16436,#16437,#16438,#16439,#16440,#16441,#16442,#16443,#16444,#16445,#16446,
#16447,#16448,#16449,#16450,#16451,#16452,#16453,#16454,#16455,#16456,#16457,
#16458,#16459,#16460,#16461,#16462,#16463,#16464,#16465,#16466,#16467,#16468,
#16469,#16470,#16471,#16472,#16473,#16474,#16475,#16476,#16477,#16478,#16479,
#16480,#16481,#16482,#16483,#16484,#16485,#16486,#16487,#16488,#16489,#16490,
#16491,#16492,#16493,#16494,#16495,#16496,#16497,#16498,#16499,#16500,#16501,
#16502,#16503,#16504,#16505,#16506,#16507,#16508,#16509,#16510,#16511,#16512,
#16513,#16514,#16515,#16516,#16517,#16518,#16519,#16520,#16521,#16522,#16523,
#16524,#16525,#16526,#16527,#16528),.UNSPECIFIED.,.F.,.F.,(4,2,2,2,2,2,
2,2,2,2,2,2,2,2,2,2,2,2,2,2,2,2,2,2,2,2,2,2,2,2,2,2,2,2,2,2,2,2,2,2,2,2,
2,2,2,2,2,2,2,2,2,2,2,2,2,2,2,2,2,2,2,2,2,2,2,2,2,2,2,2,2,2,2,2,2,2,2,2,
2,2,2,2,2,2,2,2,2,2,2,2,2,2,4),(-4.05998649109244,-3.99044868653892,-3.95612417468513,
-3.94958391300245,-3.94707104933022,-3.94533430297176,-3.94376374512821,
-3.94121389091149,-3.93491224071497,-3.85853970920352,-3.82135288996109,
-3.80378814948435,-3.79566392369472,-3.78917575318832,-3.78563392535796,
-3.78560114851417,-3.78556784745785,-3.78553400521955,-3.78549960416932,
-3.78546462596605,-3.78542905154357,-3.78540460852495,-3.78537816989084,
-3.78534955275616,-3.78531855429528,-3.785284949052,-3.78524848581845,-3.7852088840022,
-3.78516582932394,-3.7851189688123,-3.78506790484846,-3.78501218741791,
-3.78495130647743,-3.78488468463758,-3.78483352903948,-3.78475309657443,
-3.78462521567022,-3.78159649199966,-3.77765922839595,-3.77106603115191,
-3.72190272564037,-3.64569823574233,-3.62860089635745,-3.62508347628936,
-3.62312652790441,-3.62144965938125,-3.6193270972924,-3.61515758637774,
-3.58796333120841,-3.51444776445119,-3.48689846473251,-3.47007455659889,
-3.46491833212194,-3.46165961012969,-3.4586310533177,-3.45469571475831,
-3.44810950833233,-3.39886746926262,-3.32253510474421,-3.30560476888439,
-3.30209723125821,-3.30014236860668,-3.29846517792746,-3.29633949836763,
-3.29215571008368,-3.26454875851421,-3.19154894760421,-3.16394290735498,
-3.14709393960933,-3.14193476460322,-3.13867526825463,-3.13564674437131,
-3.13171251726629,-3.12513052616731,-3.07587720907922,-2.99954021199146,
-2.98260909029999,-2.97910135939408,-2.97714638476761,-2.97546909538644,
-2.97334328734951,-2.96915923600524,-2.94155014115303,-2.86854670069039,
-2.84093897507871,-2.82408899006877,-2.81892950917996,-2.81566982087076,
-2.81264111952099,-2.80870666314254,-2.80212429125671,-2.75286835703161,
-2.69164525988063),.UNSPECIFIED.);
#185=B_SPLINE_CURVE_WITH_KNOTS('',3,(#16534,#16535,#16536,#16537,#16538,
#16539,#16540,#16541),.UNSPECIFIED.,.F.,.F.,(4,1,1,1,1,4),(78.5398167494604,
79.3108996268056,80.3108456391569,81.3107916515083,82.3107376638597,82.7769112748486),
 .UNSPECIFIED.);
#186=B_SPLINE_CURVE_WITH_KNOTS('',3,(#16542,#16543,#16544,#16545,#16546,
#16547,#16548,#16549,#16550,#16551,#16552,#16553,#16554,#16555,#16556,#16557,
#16558,#16559,#16560,#16561,#16562,#16563,#16564,#16565,#16566,#16567,#16568,
#16569,#16570,#16571,#16572,#16573,#16574,#16575,#16576,#16577,#16578,#16579,
#16580,#16581,#16582,#16583,#16584,#16585,#16586,#16587,#16588,#16589,#16590,
#16591,#16592,#16593,#16594,#16595,#16596,#16597,#16598,#16599,#16600,#16601,
#16602,#16603,#16604,#16605,#16606,#16607,#16608,#16609,#16610,#16611,#16612,
#16613,#16614,#16615,#16616,#16617,#16618,#16619),.UNSPECIFIED.,.F.,.F.,
(4,2,2,2,2,2,2,2,2,2,2,2,2,2,2,2,2,2,2,2,2,2,2,2,2,2,2,2,2,2,2,2,2,2,2,
2,2,2,4),(-4.06030800713201,-3.99779701166778,-3.99312814877567,-3.99046496624178,
-3.98808965641954,-3.98637825904871,-3.98477533221798,-3.98205964130569,
-3.97472713607147,-3.92005396922612,-3.88678614013887,-3.84270727902733,
-3.83245010789196,-3.82911518963075,-3.82585347827722,-3.82282375369924,
-3.81888917523367,-3.81230923142789,-3.76326775465827,-3.71118612747833,
-3.68340591382533,-3.6694906936369,-3.66619873825633,-3.66427581734111,
-3.66259343172322,-3.66041826683211,-3.65688422741131,-3.63633485598899,
-3.62776215225491,-3.55051218449303,-3.52626917547153,-3.51099361480606,
-3.50612870745672,-3.5028676261734,-3.4998378056662,-3.49590213574806,-3.48931823678396,
-3.44007079154322,-3.39964083351492),.UNSPECIFIED.);
#187=B_SPLINE_CURVE_WITH_KNOTS('',3,(#16620,#16621,#16622,#16623,#16624,
#16625,#16626,#16627,#16628,#16629,#16630,#16631,#16632,#16633,#16634,#16635,
#16636,#16637,#16638,#16639,#16640,#16641,#16642,#16643,#16644,#16645,#16646,
#16647,#16648,#16649,#16650,#16651,#16652,#16653,#16654,#16655,#16656,#16657,
#16658,#16659,#16660,#16661,#16662,#16663,#16664,#16665,#16666,#16667,#16668,
#16669,#16670,#16671,#16672,#16673,#16674,#16675,#16676,#16677,#16678,#16679,
#16680,#16681,#16682,#16683,#16684,#16685,#16686,#16687,#16688,#16689,#16690,
#16691,#16692,#16693,#16694,#16695,#16696,#16697,#16698,#16699,#16700,#16701,
#16702,#16703,#16704,#16705,#16706,#16707,#16708,#16709,#16710,#16711,#16712,
#16713,#16714,#16715,#16716,#16717,#16718,#16719,#16720,#16721,#16722,#16723,
#16724,#16725,#16726,#16727,#16728,#16729,#16730,#16731,#16732,#16733,#16734,
#16735,#16736,#16737,#16738,#16739,#16740,#16741,#16742,#16743,#16744,#16745,
#16746,#16747,#16748,#16749,#16750,#16751,#16752,#16753,#16754,#16755,#16756,
#16757,#16758,#16759,#16760,#16761,#16762,#16763,#16764,#16765,#16766,#16767,
#16768,#16769,#16770,#16771,#16772,#16773,#16774,#16775,#16776,#16777,#16778,
#16779,#16780,#16781,#16782,#16783,#16784,#16785,#16786,#16787,#16788,#16789,
#16790,#16791,#16792,#16793,#16794,#16795,#16796,#16797,#16798,#16799,#16800,
#16801,#16802,#16803,#16804,#16805,#16806,#16807,#16808,#16809,#16810,#16811,
#16812,#16813,#16814,#16815,#16816,#16817,#16818,#16819,#16820,#16821,#16822,
#16823,#16824,#16825,#16826,#16827,#16828,#16829,#16830,#16831,#16832,#16833,
#16834,#16835,#16836,#16837,#16838,#16839,#16840,#16841,#16842,#16843,#16844,
#16845),.UNSPECIFIED.,.F.,.F.,(4,2,2,2,2,2,2,2,2,2,2,2,2,2,2,2,2,2,2,2,
2,2,2,2,2,2,2,2,2,2,2,2,2,2,2,2,2,2,2,2,2,2,2,2,2,2,2,2,2,2,2,2,2,2,2,2,
2,2,2,2,2,2,2,2,2,2,2,2,2,2,2,2,2,2,2,2,2,2,2,2,2,2,2,2,2,2,2,2,2,2,2,2,
2,2,2,2,2,2,2,2,2,2,2,2,2,2,2,2,2,2,2,2,4),(-2.69164525988063,-2.67652744625314,
-2.65959456612067,-2.65608658319691,-2.65413148378648,-2.65245409704284,
-2.65032817806746,-2.64614394591702,-2.61853515913257,-2.5455250255624,
-2.51791592128734,-2.50106505291842,-2.49590528089034,-2.49264540388283,
-2.48961652392077,-2.48568183085011,-2.47909905269859,-2.42983922230729,
-2.35349174717579,-2.33656069266682,-2.33305267414528,-2.33109749712599,
-2.32942000805571,-2.3272939134671,-2.32310919728146,-2.29549168176191,
-2.22248614591935,-2.19487453263666,-2.17802228732432,-2.17286216975934,
-2.16960209198305,-2.16657303758154,-2.16263813508684,-2.15605504442876,
-2.10679602888215,-2.03045174837929,-2.01380491832151,-2.01049077376697,
-2.00838249328433,-2.00670618453229,-2.00473743880578,-2.00116731427396,
-1.98317011768556,-1.90762229780562,-1.85877966320953,-1.8522051012188,
-1.84827261098029,-1.84524385997702,-1.84198257919614,-1.83681729749719,
-1.81991911702346,-1.7921984464339,-1.72020846029211,-1.71111613148174,
-1.69110900349414,-1.68760281185066,-1.68543627544157,-1.68375512195578,
-1.68182750962024,-1.67844555674473,-1.66345853408425,-1.58561588569702,
-1.53575222944299,-1.52915738590937,-1.52521900312959,-1.52218935663289,
-1.51893069621455,-1.51377719761044,-1.49698580023694,-1.46950961555556,
-1.39517766611248,-1.36854480229695,-1.36439422904569,-1.36227536989895,
-1.36059834518428,-1.35863764771494,-1.35510456347838,-1.33775356205248,
-1.26175017341635,-1.21265962203328,-1.20608007213211,-1.2021461339271,
-1.19911716565885,-1.19585653569015,-1.19069417160215,-1.17382246525547,
-1.14616249481071,-1.07347428975496,-1.04555543473885,-1.04136043479394,
-1.0392320871024,-1.03755435039807,-1.03560063073145,-1.03209958271399,
-1.01528481095655,-0.938888458637008,-0.889603476585265,-0.883020031294518,
-0.879084956491885,-0.876055810106649,-0.872795674853165,-0.86763555705628,
-0.85078429566735,-0.823171191116063,-0.74999963593344,-0.722469906107444,
-0.718287840389341,-0.716162247404762,-0.714484719962632,-0.712528987965407,
-0.709018722734614,-0.69205185495633,-0.66172580755329),.UNSPECIFIED.);
#188=B_SPLINE_CURVE_WITH_KNOTS('',3,(#16851,#16852,#16853,#16854,#16855,
#16856,#16857,#16858,#16859,#16860,#16861,#16862,#16863,#16864,#16865,#16866,
#16867,#16868,#16869,#16870,#16871,#16872,#16873,#16874,#16875,#16876,#16877,
#16878,#16879,#16880,#16881,#16882,#16883,#16884,#16885,#16886,#16887,#16888,
#16889,#16890,#16891,#16892,#16893,#16894,#16895,#16896,#16897,#16898,#16899,
#16900,#16901,#16902,#16903,#16904,#16905,#16906,#16907,#16908,#16909,#16910,
#16911,#16912,#16913,#16914,#16915,#16916,#16917,#16918,#16919,#16920,#16921,
#16922,#16923,#16924,#16925,#16926,#16927,#16928,#16929,#16930,#16931,#16932,
#16933,#16934,#16935,#16936,#16937,#16938,#16939,#16940,#16941,#16942,#16943,
#16944,#16945,#16946,#16947,#16948,#16949,#16950,#16951,#16952,#16953,#16954,
#16955,#16956,#16957,#16958,#16959,#16960,#16961,#16962,#16963,#16964,#16965,
#16966,#16967,#16968,#16969,#16970,#16971,#16972,#16973,#16974,#16975,#16976,
#16977,#16978,#16979,#16980,#16981,#16982,#16983,#16984,#16985,#16986,#16987,
#16988,#16989,#16990,#16991,#16992,#16993,#16994,#16995,#16996,#16997,#16998,
#16999,#17000,#17001,#17002,#17003,#17004,#17005,#17006,#17007,#17008,#17009,
#17010,#17011,#17012,#17013,#17014,#17015,#17016,#17017,#17018,#17019,#17020,
#17021,#17022,#17023,#17024,#17025,#17026,#17027,#17028,#17029,#17030,#17031,
#17032,#17033,#17034,#17035,#17036,#17037,#17038,#17039,#17040),
 .UNSPECIFIED.,.F.,.F.,(4,2,2,2,2,2,2,2,2,2,2,2,2,2,2,2,2,2,2,2,2,2,2,2,
2,2,2,2,2,2,2,2,2,2,2,2,2,2,2,2,2,2,2,2,2,2,2,2,2,2,2,2,2,2,2,2,2,2,2,2,
2,2,2,2,2,2,2,2,2,2,2,2,2,2,2,2,2,2,2,2,2,2,2,2,2,2,2,2,2,2,2,2,2,2,4),
(-1.37000516159202,-1.32982235070187,-1.30088677921817,-1.29507105438874,
-1.29132394001103,-1.2883254321715,-1.28492796263422,-1.27915059295163,
-1.25563521732469,-1.17675103002816,-1.13557854015604,-1.13107525122225,
-1.1289133898409,-1.12723212717903,-1.12530014487673,-1.12190041465387,
-1.1066688211435,-1.02899722392388,-0.979233631022262,-0.972639024540158,
-0.968699933566932,-0.965669236953448,-0.962408943672752,-0.95725177657945,
-0.940438429841211,-0.912915163360214,-0.838971107817674,-0.812040641643707,
-0.807878264526655,-0.805756405411002,-0.80407856986728,-0.802118694677714,
-0.798591504142505,-0.781356576663223,-0.705236566564479,-0.656157545825954,
-0.649562872356873,-0.645623749486369,-0.64259303306983,-0.639332723147275,
-0.63417553965061,-0.617362227933496,-0.589839108652345,-0.515892035835737,
-0.488963362485876,-0.484801029417397,-0.482679172153062,-0.481001327390222,
-0.479041429115078,-0.47551416617306,-0.458278274677027,-0.382158419390071,
-0.333079370543377,-0.325901714702702,-0.32220015647419,-0.319325300356319,
-0.319201804662897,-0.319098681490327,-0.319010062672658,-0.318932276434972,
-0.318862866167265,-0.318800104331356,-0.31874272871045,-0.318689788455967,
-0.318640549072348,-0.318594431079622,-0.318550968963718,-0.318509782802414,
-0.318470558165119,-0.318433031537635,-0.318396979522895,-0.318362210721167,
-0.318328559515459,-0.318295881248411,-0.318264048433537,-0.318232947722156,
-0.318163601624379,-0.318094221438091,-0.318024701903007,-0.317954942841739,
-0.314230023579432,-0.306387687448059,-0.24462636351261,-0.16918610614987,
-0.162802602600097,-0.160237844753108,-0.15866367422278,-0.156928082368122,
-0.154425746987008,-0.147961734233512,-0.0990691438969175,-0.0207871264132375,
-0.00677755631971555,-0.00293676047487332,-0.00101485485105488),
 .UNSPECIFIED.);
#189=B_SPLINE_CURVE_WITH_KNOTS('',3,(#17041,#17042,#17043,#17044,#17045,
#17046),.UNSPECIFIED.,.F.,.F.,(4,1,1,4),(82.7769112748486,83.3106836762111,
84.3106296885624,84.8230016469246),.UNSPECIFIED.);
#190=B_SPLINE_CURVE_WITH_KNOTS('',3,(#17048,#17049,#17050,#17051,#17052,
#17053,#17054,#17055,#17056,#17057,#17058,#17059,#17060,#17061,#17062,#17063,
#17064,#17065,#17066,#17067,#17068,#17069,#17070,#17071,#17072,#17073,#17074,
#17075,#17076,#17077,#17078,#17079,#17080,#17081,#17082,#17083,#17084,#17085,
#17086,#17087,#17088,#17089,#17090,#17091,#17092,#17093,#17094,#17095,#17096,
#17097,#17098,#17099,#17100,#17101,#17102,#17103,#17104,#17105,#17106,#17107,
#17108,#17109,#17110,#17111,#17112,#17113,#17114,#17115,#17116,#17117,#17118,
#17119,#17120,#17121,#17122,#17123),.UNSPECIFIED.,.F.,.F.,(4,2,2,2,2,2,
2,2,2,2,2,2,2,2,2,2,2,2,2,2,2,2,2,2,2,2,2,2,2,2,2,2,2,2,2,2,2,4),(-0.66172580755329,
-0.615768135562443,-0.566537092661659,-0.559954712151595,-0.556019943285156,
-0.552990839211819,-0.549730559234709,-0.544569806894018,-0.52804181333161,
-0.501027722968988,-0.423398787581568,-0.4222793957237,-0.399108186475157,
-0.395451222298192,-0.393263280845654,-0.391575308553205,-0.389682444530973,
-0.386522450347328,-0.374257392356896,-0.351272631358261,-0.29881050401711,
-0.243668379532499,-0.236993498479392,-0.233031688399543,-0.229998136996049,
-0.226749065290884,-0.221639837704353,-0.205642210257806,-0.164450525013423,
-0.131305979381181,-0.0767137492516896,-0.0722792425654901,-0.0701313490448679,
-0.0684519482407693,-0.066511922119817,-0.0644633838945868,-0.0613034965144324,
-0.000962151141444392),.UNSPECIFIED.);
#191=B_SPLINE_CURVE_WITH_KNOTS('',3,(#17124,#17125,#17126,#17127,#17128,
#17129,#17130,#17131,#17132,#17133,#17134,#17135,#17136,#17137,#17138,#17139,
#17140,#17141,#17142,#17143,#17144,#17145,#17146,#17147,#17148,#17149,#17150,
#17151,#17152,#17153,#17154,#17155,#17156,#17157,#17158,#17159,#17160,#17161,
#17162,#17163,#17164,#17165,#17166,#17167,#17168,#17169,#17170,#17171,#17172,
#17173,#17174,#17175,#17176,#17177,#17178,#17179,#17180,#17181,#17182,#17183,
#17184,#17185,#17186,#17187,#17188,#17189,#17190,#17191,#17192,#17193,#17194,
#17195,#17196,#17197,#17198,#17199,#17200,#17201,#17202,#17203,#17204,#17205,
#17206,#17207,#17208,#17209,#17210,#17211,#17212,#17213,#17214,#17215,#17216,
#17217,#17218,#17219,#17220,#17221,#17222,#17223,#17224,#17225,#17226,#17227,
#17228,#17229,#17230,#17231,#17232,#17233,#17234,#17235,#17236,#17237,#17238,
#17239,#17240,#17241,#17242,#17243,#17244,#17245,#17246,#17247,#17248,#17249,
#17250,#17251,#17252,#17253,#17254,#17255,#17256,#17257,#17258,#17259,#17260,
#17261,#17262,#17263,#17264,#17265,#17266,#17267,#17268,#17269,#17270,#17271,
#17272,#17273),.UNSPECIFIED.,.F.,.F.,(4,2,2,2,2,2,2,2,2,2,2,2,2,2,2,2,2,
2,2,2,2,2,2,2,2,2,2,2,2,2,2,2,2,2,2,2,2,2,2,2,2,2,2,2,2,2,2,2,2,2,2,2,2,
2,2,2,2,2,2,2,2,2,2,2,2,2,2,2,2,2,2,2,2,2,4),(-4.06115038023093,-3.99429509258559,
-3.98279511263255,-3.97679793062009,-3.97165267525303,-3.96839642445301,
-3.96536707786196,-3.96142632143306,-3.95482134705909,-3.8860872897746,
-3.85413284097312,-3.8182929323426,-3.81083640844067,-3.80879905270211,
-3.80686710321459,-3.80518722628126,-3.80302897507252,-3.79853953745811,
-3.75860831996345,-3.69128076668005,-3.65665186120019,-3.65021792731777,
-3.64656568227414,-3.64357572969109,-3.64011310782554,-3.63419116237318,
-3.61129640472461,-3.60184646027432,-3.52563564692273,-3.50157524369334,
-3.48893334798986,-3.48570807793765,-3.48381544371097,-3.4821280323054,
-3.47994130355179,-3.47628740115911,-3.45316911977267,-3.44248572875624,
-3.37541484079659,-3.3478082031626,-3.3309590937197,-3.32579998517169,-3.32254055612835,
-3.31951211225338,-3.31557801389033,-3.30899629283811,-3.25974954865934,
-3.18342551933013,-3.16647983977272,-3.16297129204163,-3.16101616893573,
-3.15933894190941,-3.15721345666721,-3.15303077504045,-3.12546002509056,
-3.0524112953787,-3.02480899577556,-3.00796149928777,-3.00280237468692,
-2.99954281795653,-2.99651417431887,-2.99257970127295,-2.98599709957066,
-2.9367226200479,-2.86034245058973,-2.8434655504661,-2.83996101611495,-2.83800669816343,
-2.83632927564846,-2.83420240347714,-2.83001355703396,-2.80226401775156,
-2.72943180907567,-2.70180606633594,-2.69239263445687),.UNSPECIFIED.);
#192=B_SPLINE_CURVE_WITH_KNOTS('',3,(#17278,#17279,#17280,#17281,#17282,
#17283,#17284,#17285,#17286,#17287,#17288,#17289,#17290,#17291,#17292,#17293,
#17294,#17295,#17296,#17297,#17298,#17299,#17300,#17301,#17302,#17303,#17304,
#17305,#17306,#17307,#17308,#17309,#17310,#17311,#17312,#17313,#17314,#17315,
#17316,#17317,#17318,#17319,#17320,#17321,#17322,#17323,#17324,#17325,#17326,
#17327,#17328,#17329,#17330,#17331,#17332,#17333,#17334,#17335,#17336,#17337,
#17338,#17339,#17340,#17341,#17342,#17343,#17344,#17345,#17346,#17347,#17348,
#17349,#17350,#17351,#17352,#17353,#17354,#17355,#17356,#17357,#17358,#17359,
#17360,#17361,#17362,#17363,#17364,#17365,#17366,#17367,#17368,#17369,#17370,
#17371,#17372,#17373,#17374,#17375,#17376,#17377,#17378,#17379,#17380,#17381,
#17382,#17383,#17384,#17385,#17386,#17387,#17388,#17389,#17390,#17391,#17392,
#17393,#17394,#17395,#17396,#17397,#17398,#17399,#17400,#17401,#17402,#17403,
#17404,#17405,#17406,#17407,#17408,#17409,#17410,#17411,#17412,#17413,#17414,
#17415,#17416,#17417,#17418,#17419,#17420,#17421,#17422,#17423,#17424,#17425,
#17426,#17427,#17428,#17429,#17430,#17431,#17432,#17433,#17434,#17435,#17436,
#17437,#17438,#17439,#17440,#17441,#17442,#17443,#17444,#17445,#17446,#17447,
#17448,#17449,#17450,#17451,#17452,#17453,#17454,#17455,#17456,#17457,#17458,
#17459,#17460,#17461,#17462,#17463,#17464,#17465,#17466,#17467,#17468,#17469,
#17470,#17471,#17472,#17473,#17474,#17475,#17476,#17477,#17478,#17479,#17480,
#17481,#17482,#17483,#17484,#17485,#17486,#17487,#17488,#17489,#17490,#17491,
#17492,#17493,#17494,#17495,#17496,#17497,#17498,#17499,#17500,#17501,#17502,
#17503,#17504,#17505),.UNSPECIFIED.,.F.,.F.,(4,2,2,2,2,2,2,2,2,2,2,2,2,
2,2,2,2,2,2,2,2,2,2,2,2,2,2,2,2,2,2,2,2,2,2,2,2,2,2,2,2,2,2,2,2,2,2,2,2,
2,2,2,2,2,2,2,2,2,2,2,2,2,2,2,2,2,2,2,2,2,2,2,2,2,2,2,2,2,2,2,2,2,2,2,2,
2,2,2,2,2,2,2,2,2,2,2,2,2,2,2,2,2,2,2,2,2,2,2,2,2,2,2,2,4),(-3.39962357914392,
-3.39506088796122,-3.3915554724998,-3.38960072794962,-3.38792296976071,
-3.38579567531718,-3.3816059838441,-3.35384994273638,-3.2810404240971,-3.25342214272944,
-3.23656693633569,-3.23140614882391,-3.2281456800974,-3.2251162781971,-3.22118093836022,
-3.21459712076029,-3.16531107070317,-3.08880520796687,-3.07206850046493,
-3.06857190097623,-3.06661900812461,-3.06494093677447,-3.06281079620667,
-3.05860809086884,-3.03045428610733,-2.958127260132,-2.93046241794374,-2.91358660328308,
-2.908423347958,-2.90516220481268,-2.90213278659885,-2.89819829177458,-2.89161779584987,
-2.84251503884156,-2.76638617725541,-2.7491301790426,-2.74560220543741,
-2.74364240355827,-2.74196493690716,-2.7398439479749,-2.73568448003327,
-2.70881402666259,-2.6348625953276,-2.6073657257391,-2.59056300616248,-2.58540761273744,
-2.58214808518325,-2.57911785369498,-2.57517901465898,-2.56858400175031,
-2.5187643998977,-2.44093339664959,-2.42585876816632,-2.42247013236351,
-2.42054075582029,-2.41885936595049,-2.41669421477148,-2.41217316321173,
-2.3676139551844,-2.31372474348187,-2.28500958960437,-2.26767905490894,
-2.26246596759375,-2.25919349503569,-2.25616733200127,-2.25225647748129,
-2.24575792849089,-2.20040242075149,-2.13257354208228,-2.10646078717017,
-2.10078641632752,-2.09841165534728,-2.0967002468842,-2.09509698618824,
-2.0923800448108,-2.08504017463944,-2.0313624349916,-2.00076102426971,-1.94853200347732,
-1.94189176875138,-1.93793945320682,-1.93490673759133,-1.93165226422132,
-1.92652123554799,-1.90994253883999,-1.88295325472521,-1.80682085236967,
-1.78117681975093,-1.77706251318236,-1.77495098808381,-1.77327390651068,
-1.77130631613008,-1.7677435062251,-1.74989199927299,-1.67421247374382,
-1.62534480071989,-1.6187681644757,-1.6148343465868,-1.61180451299719,-1.60854200104179,
-1.60337461461672,-1.5864678405104,-1.55873028604816,-1.48699834313129,
-1.47913249852733,-1.4577920244589,-1.4542188432688,-1.45205514353547,-1.45036978714444,
-1.44846166020954,-1.44516987713201,-1.43142620396899,-1.40426158146784,
-1.37000516159202),.UNSPECIFIED.);
#193=B_SPLINE_CURVE_WITH_KNOTS('',3,(#17506,#17507,#17508,#17509,#17510,
#17511,#17512,#17513,#17514,#17515,#17516,#17517,#17518,#17519,#17520,#17521,
#17522,#17523,#17524,#17525,#17526,#17527,#17528,#17529,#17530,#17531,#17532,
#17533,#17534,#17535,#17536,#17537,#17538,#17539,#17540,#17541,#17542,#17543,
#17544,#17545,#17546,#17547,#17548,#17549,#17550,#17551,#17552,#17553,#17554,
#17555,#17556,#17557,#17558,#17559,#17560,#17561,#17562,#17563,#17564,#17565,
#17566,#17567,#17568,#17569,#17570,#17571,#17572,#17573,#17574,#17575,#17576,
#17577,#17578,#17579,#17580,#17581,#17582,#17583,#17584,#17585,#17586,#17587,
#17588,#17589,#17590,#17591,#17592,#17593,#17594,#17595,#17596,#17597,#17598,
#17599,#17600,#17601,#17602,#17603,#17604,#17605,#17606,#17607,#17608,#17609,
#17610,#17611,#17612,#17613,#17614,#17615,#17616,#17617,#17618,#17619,#17620,
#17621,#17622,#17623,#17624,#17625,#17626,#17627,#17628,#17629,#17630,#17631,
#17632,#17633,#17634,#17635,#17636,#17637,#17638,#17639,#17640,#17641,#17642,
#17643,#17644,#17645,#17646,#17647,#17648,#17649,#17650,#17651,#17652,#17653,
#17654,#17655,#17656,#17657,#17658,#17659,#17660,#17661,#17662,#17663,#17664,
#17665,#17666,#17667,#17668,#17669,#17670,#17671,#17672,#17673,#17674,#17675,
#17676,#17677,#17678,#17679,#17680,#17681,#17682,#17683,#17684,#17685,#17686,
#17687,#17688,#17689,#17690,#17691,#17692,#17693,#17694,#17695,#17696,#17697,
#17698,#17699,#17700,#17701,#17702,#17703,#17704,#17705,#17706,#17707,#17708,
#17709,#17710,#17711,#17712,#17713,#17714,#17715,#17716,#17717,#17718,#17719,
#17720,#17721,#17722,#17723,#17724,#17725,#17726,#17727),.UNSPECIFIED.,
 .F.,.F.,(4,2,2,2,2,2,2,2,2,2,2,2,2,2,2,2,2,2,2,2,2,2,2,2,2,2,2,2,2,2,2,
2,2,2,2,2,2,2,2,2,2,2,2,2,2,2,2,2,2,2,2,2,2,2,2,2,2,2,2,2,2,2,2,2,2,2,2,
2,2,2,2,2,2,2,2,2,2,2,2,2,2,2,2,2,2,2,2,2,2,2,2,2,2,2,2,2,2,2,2,2,2,2,2,
2,2,2,2,2,2,2,4),(-2.69239263445687,-2.68494805292635,-2.67978757582851,
-2.67652759501388,-2.67349885434821,-2.66956467689721,-2.66298349870764,
-2.61379696160392,-2.53759830361569,-2.52046772848944,-2.51694780762479,
-2.5149900667759,-2.51331288826232,-2.51119040705332,-2.5070224745021,-2.4798927647365,
-2.40627172202468,-2.37872696173466,-2.36190404259822,-2.35674724051752,
-2.35348795018369,-2.35045872477708,-2.34652231798558,-2.33993388396048,
-2.29039816588765,-2.21343866888421,-2.1973098812984,-2.19385165876666,
-2.19190731894903,-2.19022852360582,-2.18808704585153,-2.18368484504786,
-2.12738993921722,-2.07809390211431,-2.04143874025707,-2.03489625227751,
-2.03133286737907,-2.0286435069976,-2.02521479706254,-2.01929254210226,
-1.99380399589262,-1.90047394336956,-1.87536059273919,-1.87126783657065,
-1.86916122492772,-1.86748481286403,-1.86551428325093,-1.86193667845401,
-1.84381164453842,-1.76748207762536,-1.71950776176137,-1.71295045618029,
-1.7090227353855,-1.70599440352357,-1.7027303611341,-1.69755383773739,-1.68055691677225,
-1.6526106382063,-1.58404448324062,-1.57658767255684,-1.55222016781284,
-1.54815818923646,-1.54605823947949,-1.5443822550099,-1.54240654249387,
-1.53880490824678,-1.52023993554453,-1.43952662179443,-1.39620611486845,
-1.38976139100435,-1.38586671757373,-1.38284347951215,-1.37956458761676,
-1.37432049682264,-1.35669203415515,-1.32727163504134,-1.27006636671304,
-1.22975110607695,-1.22525614736234,-1.22309631817013,-1.22141572200668,
-1.21948350592894,-1.21608101054728,-1.20079837103807,-1.12319518883931,
-1.07341206272411,-1.06681839394118,-1.06288020816388,-1.05985041866396,
-1.05659131471602,-1.05143649823933,-1.03463531258242,-1.00713753647854,
-0.932945791112551,-0.906202381460083,-0.902047574576181,-0.899927721240331,
-0.898250515854938,-0.896290306607768,-0.892759858318587,-0.875456810432336,
-0.7994125013577,-0.750300164886178,-0.743719777385732,-0.739785450825536,
-0.736756249290266,-0.733495432987769,-0.728332911989022,-0.711461930755637,
-0.683804411334442,-0.662325194366873),.UNSPECIFIED.);
#194=B_SPLINE_CURVE_WITH_KNOTS('',3,(#17733,#17734,#17735,#17736,#17737,
#17738,#17739,#17740,#17741,#17742,#17743,#17744,#17745,#17746,#17747,#17748,
#17749,#17750,#17751,#17752,#17753,#17754,#17755,#17756,#17757,#17758,#17759,
#17760,#17761,#17762,#17763,#17764,#17765,#17766,#17767,#17768,#17769,#17770,
#17771,#17772,#17773,#17774,#17775,#17776,#17777,#17778,#17779,#17780,#17781,
#17782,#17783,#17784,#17785,#17786,#17787,#17788,#17789,#17790,#17791,#17792,
#17793,#17794,#17795,#17796,#17797,#17798,#17799,#17800,#17801,#17802,#17803,
#17804,#17805,#17806,#17807,#17808,#17809,#17810,#17811,#17812,#17813,#17814,
#17815,#17816,#17817,#17818,#17819,#17820,#17821,#17822,#17823,#17824,#17825,
#17826,#17827,#17828,#17829,#17830,#17831,#17832,#17833,#17834,#17835,#17836,
#17837,#17838,#17839,#17840,#17841,#17842,#17843,#17844,#17845,#17846,#17847,
#17848,#17849,#17850,#17851,#17852,#17853,#17854,#17855,#17856,#17857,#17858,
#17859,#17860,#17861,#17862,#17863,#17864,#17865,#17866,#17867,#17868,#17869,
#17870,#17871,#17872,#17873,#17874,#17875,#17876),.UNSPECIFIED.,.F.,.F.,
(4,2,2,2,2,2,2,2,2,2,2,2,2,2,2,2,2,2,2,2,2,2,2,2,2,2,2,2,2,2,2,2,2,2,2,
2,2,2,2,2,2,2,2,2,2,2,2,2,2,2,2,2,2,2,2,2,2,2,2,2,2,2,2,2,2,2,2,2,2,2,2,
4),(-1.37004935497571,-1.30316814073184,-1.27508590256901,-1.27088446362104,
-1.26875426131253,-1.26707578184677,-1.2651219901352,-1.26162275082394,
-1.24485306745913,-1.16838984102694,-1.11911934000211,-1.11253443969424,
-1.10859815524532,-1.10556786980449,-1.10230629761672,-1.09714344070059,
-1.08027875778301,-1.05263806889375,-0.979775356429106,-0.951992575268294,
-0.947800918301569,-0.945672799035891,-0.943994481073714,-0.942039177454788,
-0.938533010293787,-0.921649541242461,-0.845271004511879,-0.796040646420658,
-0.789456544497113,-0.78552049137532,-0.782490240252348,-0.77922856340077,
-0.774065238989404,-0.757196325440682,-0.729545946934489,-0.656785124254543,
-0.628922400823095,-0.624726474804089,-0.622597445431669,-0.620919056340561,
-0.618964412410942,-0.615461271852217,-0.598627651596522,-0.522212035718397,
-0.472963998196164,-0.466379541122371,-0.462443383869284,-0.459413115819201,
-0.456151483035575,-0.450988361150219,-0.434121298566828,-0.406475166261227,
-0.350586438844927,-0.306303489975825,-0.301784112712283,-0.299619152640829,
-0.298007594518476,-0.296141552441799,-0.293047574959632,-0.289240971296497,
-0.281509140178125,-0.260352216935445,-0.239235334321867,-0.154554828047918,
-0.144354980870009,-0.140409077232606,-0.137559226511286,-0.134521501711864,
-0.13046826243361,-0.121453444454761,-0.0678787593783522,-0.000963316407824259),
 .UNSPECIFIED.);
#195=B_SPLINE_CURVE_WITH_KNOTS('',3,(#17877,#17878,#17879,#17880,#17881,
#17882,#17883,#17884,#17885,#17886,#17887,#17888,#17889,#17890,#17891,#17892,
#17893,#17894,#17895,#17896,#17897,#17898,#17899,#17900,#17901,#17902,#17903,
#17904,#17905,#17906,#17907,#17908,#17909,#17910,#17911,#17912,#17913,#17914,
#17915,#17916,#17917,#17918,#17919,#17920,#17921,#17922,#17923,#17924,#17925,
#17926,#17927,#17928,#17929,#17930,#17931,#17932,#17933,#17934,#17935,#17936,
#17937,#17938,#17939,#17940,#17941,#17942,#17943,#17944,#17945,#17946,#17947,
#17948,#17949,#17950,#17951,#17952,#17953,#17954,#17955,#17956,#17957,#17958,
#17959,#17960,#17961,#17962,#17963,#17964,#17965,#17966,#17967,#17968,#17969,
#17970,#17971,#17972,#17973,#17974,#17975,#17976,#17977,#17978,#17979,#17980,
#17981,#17982,#17983,#17984),.UNSPECIFIED.,.F.,.F.,(4,2,2,2,2,2,2,2,2,2,
2,2,2,2,2,2,2,2,2,2,2,2,2,2,2,2,2,2,2,2,2,2,2,2,2,2,2,2,2,2,2,2,2,2,2,2,
2,2,2,2,2,2,2,4),(-4.06031153053636,-4.04337786345749,-4.03987712903709,
-4.03768755233355,-4.03602554017982,-4.03440578151757,-4.03254341866112,
-4.02945553836437,-4.01931539272372,-4.01724335198028,-4.00491278016662,
-3.92971739228819,-3.90024592326161,-3.88259511281969,-3.87734908052151,
-3.87406997879228,-3.87104721993485,-3.86715409244408,-3.86071386128505,
-3.81753542449335,-3.75502227978076,-3.73037489300684,-3.72181138694382,
-3.71771675965949,-3.71440415088888,-3.71250338171311,-3.71249836360561,
-3.71249331681531,-3.71248824113156,-3.71248313638129,-3.71247800235655,
-3.71247283886091,-3.71246764571772,-3.71246242269704,-3.7124571695903,
-3.71245188615722,-3.71244657221248,-3.71244122758163,-3.71243585200552,
-3.7108368205494,-3.70869548668606,-3.70429402468919,-3.67063532828294,
-3.60402318881109,-3.57639402337472,-3.55953435347856,-3.55437327240694,
-3.55111286546653,-3.54808369158684,-3.5441488901654,-3.53756650697364,
-3.48833563132933,-3.41194473479421,-3.39962357914392),.UNSPECIFIED.);
#196=B_SPLINE_CURVE_WITH_KNOTS('',3,(#17986,#17987,#17988,#17989,#17990,
#17991,#17992,#17993,#17994,#17995,#17996,#17997,#17998,#17999,#18000,#18001,
#18002,#18003,#18004,#18005,#18006,#18007,#18008,#18009,#18010,#18011,#18012,
#18013,#18014,#18015,#18016,#18017,#18018,#18019,#18020,#18021,#18022,#18023,
#18024,#18025,#18026,#18027,#18028,#18029,#18030,#18031,#18032,#18033,#18034,
#18035,#18036,#18037,#18038,#18039,#18040,#18041,#18042,#18043,#18044,#18045,
#18046,#18047,#18048,#18049,#18050,#18051,#18052,#18053,#18054,#18055,#18056,
#18057,#18058,#18059,#18060,#18061),.UNSPECIFIED.,.F.,.F.,(4,2,2,2,2,2,
2,2,2,2,2,2,2,2,2,2,2,2,2,2,2,2,2,2,2,2,2,2,2,2,2,2,2,2,2,2,2,4),(-0.662325194366873,
-0.621620560052431,-0.608018603129565,-0.583038657207035,-0.578951600005077,
-0.576846344508726,-0.575170178549449,-0.573198969096297,-0.569623919237428,
-0.551709241105021,-0.476114929834138,-0.42724563765023,-0.42067035999194,
-0.416737597903866,-0.413708728920349,-0.410447411189627,-0.405282263178068,
-0.388696553075173,-0.361559940071661,-0.301674190535358,-0.26057087022593,
-0.256069367877931,-0.253908347764074,-0.252227737227905,-0.250296533647604,
-0.248260527748304,-0.240825517343258,-0.203497007398002,-0.171011365616584,
-0.104354867742704,-0.0977149872544985,-0.0937633978297387,-0.0907315478861691,
-0.0874783116247841,-0.0823498995925742,-0.0763773277259736,-0.0649442964123356,
-0.000962519665250632),.UNSPECIFIED.);
#197=B_SPLINE_CURVE_WITH_KNOTS('',3,(#18062,#18063,#18064,#18065,#18066,
#18067,#18068,#18069,#18070,#18071,#18072,#18073,#18074,#18075,#18076,#18077,
#18078,#18079,#18080,#18081,#18082,#18083,#18084,#18085,#18086,#18087,#18088,
#18089,#18090,#18091,#18092,#18093,#18094,#18095,#18096,#18097,#18098,#18099,
#18100,#18101,#18102,#18103,#18104,#18105,#18106,#18107,#18108,#18109,#18110,
#18111,#18112,#18113,#18114,#18115,#18116,#18117,#18118,#18119,#18120,#18121,
#18122,#18123,#18124,#18125,#18126,#18127,#18128,#18129,#18130,#18131,#18132,
#18133,#18134,#18135,#18136,#18137,#18138,#18139,#18140,#18141,#18142,#18143,
#18144,#18145,#18146,#18147,#18148,#18149,#18150,#18151,#18152,#18153,#18154,
#18155,#18156,#18157,#18158,#18159,#18160,#18161,#18162,#18163,#18164,#18165,
#18166,#18167,#18168,#18169,#18170,#18171,#18172,#18173,#18174,#18175,#18176,
#18177,#18178,#18179,#18180,#18181,#18182,#18183,#18184,#18185,#18186,#18187,
#18188,#18189,#18190,#18191,#18192,#18193,#18194,#18195,#18196,#18197,#18198,
#18199,#18200,#18201,#18202,#18203,#18204,#18205,#18206,#18207,#18208,#18209,
#18210,#18211,#18212,#18213,#18214,#18215),.UNSPECIFIED.,.F.,.F.,(4,2,2,
2,2,2,2,2,2,2,2,2,2,2,2,2,2,2,2,2,2,2,2,2,2,2,2,2,2,2,2,2,2,2,2,2,2,2,2,
2,2,2,2,2,2,2,2,2,2,2,2,2,2,2,2,2,2,2,2,2,2,2,2,2,2,2,2,2,2,2,2,2,2,2,2,
2,4),(-4.06032274020453,-4.0029643398074,-3.99696048208845,-3.99378252294505,
-3.99172667450296,-3.98978165610366,-3.98810331451559,-3.98596376197808,
-3.98157005092537,-3.92462360203421,-3.89235197403768,-3.85324049661156,
-3.83678405184572,-3.83162472556174,-3.82836505943201,-3.82533632658513,
-3.82140175531127,-3.81481902818917,-3.76554685382997,-3.68917231439229,
-3.67230747717275,-3.6688197833286,-3.66685353860644,-3.66517720869091,
-3.66306617230716,-3.65895148834677,-3.63326063075447,-3.55733803239008,
-3.53029632549652,-3.51375363272254,-3.50859229192791,-3.50533207760003,
-3.50230333530921,-3.4983694613703,-3.49178946412029,-3.44266758315225,
-3.36659708823063,-3.34928753844733,-3.34575697895428,-3.3437968986097,
-3.34211991421794,-3.34000049329885,-3.33584698625794,-3.30912508433863,
-3.23496745662917,-3.20748843670299,-3.19069417538195,-3.18554047188149,
-3.18228182566897,-3.17925229075347,-3.17531419091688,-3.16872007524078,
-3.11890072808387,-3.04120185447702,-3.02599161240632,-3.0225941742133,
-3.02066314539534,-3.01898249002419,-3.01682117035122,-3.01231817897828,
-2.97099042824152,-2.89189611096141,-2.86875351755784,-2.86300673510385,
-2.85961678094982,-2.85661848955385,-2.85286316036893,-2.84701836752918,
-2.81766043200606,-2.74380101561582,-2.71651328172788,-2.70273126574828,
-2.69943726530728,-2.69752905649933,-2.69584443467197,-2.69368276982011,
-2.69185776365183),.UNSPECIFIED.);
#198=B_SPLINE_CURVE_WITH_KNOTS('',3,(#18220,#18221,#18222,#18223,#18224,
#18225,#18226,#18227,#18228,#18229,#18230,#18231,#18232,#18233,#18234,#18235,
#18236,#18237,#18238,#18239,#18240,#18241,#18242,#18243,#18244,#18245,#18246,
#18247,#18248,#18249,#18250,#18251,#18252,#18253,#18254,#18255,#18256,#18257,
#18258,#18259,#18260,#18261,#18262,#18263,#18264,#18265,#18266,#18267,#18268,
#18269,#18270,#18271,#18272,#18273,#18274,#18275,#18276,#18277,#18278,#18279,
#18280,#18281,#18282,#18283,#18284,#18285,#18286,#18287,#18288,#18289,#18290,
#18291,#18292,#18293,#18294,#18295,#18296,#18297,#18298,#18299,#18300,#18301,
#18302,#18303,#18304,#18305,#18306,#18307,#18308,#18309,#18310,#18311,#18312,
#18313,#18314,#18315,#18316,#18317,#18318,#18319,#18320,#18321,#18322,#18323,
#18324,#18325,#18326,#18327,#18328,#18329,#18330,#18331,#18332,#18333,#18334,
#18335,#18336,#18337,#18338,#18339,#18340,#18341,#18342,#18343,#18344,#18345,
#18346,#18347,#18348,#18349,#18350,#18351,#18352,#18353,#18354,#18355,#18356,
#18357,#18358,#18359,#18360,#18361,#18362,#18363,#18364,#18365,#18366,#18367,
#18368,#18369,#18370,#18371,#18372,#18373,#18374,#18375,#18376,#18377,#18378,
#18379,#18380,#18381,#18382,#18383,#18384,#18385,#18386,#18387,#18388,#18389,
#18390,#18391,#18392,#18393,#18394,#18395,#18396,#18397,#18398,#18399,#18400,
#18401,#18402,#18403,#18404,#18405,#18406,#18407,#18408,#18409,#18410,#18411,
#18412,#18413,#18414,#18415,#18416,#18417,#18418,#18419,#18420,#18421,#18422,
#18423,#18424,#18425,#18426,#18427,#18428,#18429,#18430,#18431,#18432,#18433,
#18434,#18435,#18436,#18437,#18438,#18439,#18440,#18441,#18442,#18443),
 .UNSPECIFIED.,.F.,.F.,(4,2,2,2,2,2,2,2,2,2,2,2,2,2,2,2,2,2,2,2,2,2,2,2,
2,2,2,2,2,2,2,2,2,2,2,2,2,2,2,2,2,2,2,2,2,2,2,2,2,2,2,2,2,2,2,2,2,2,2,2,
2,2,2,2,2,2,2,2,2,2,2,2,2,2,2,2,2,2,2,2,2,2,2,2,2,2,2,2,2,2,2,2,2,2,2,2,
2,2,2,2,2,2,2,2,2,2,2,2,2,2,2,4),(-3.39991501201283,-3.39345442372656,-3.37665005401964,
-3.37149486401831,-3.36823562909115,-3.36520578297209,-3.3612676059447,
-3.35467405689956,-3.30553505650724,-3.22928879242379,-3.21220158311604,
-3.2086837866258,-3.20672627421138,-3.2050486941596,-3.20292490283201,-3.19875196737591,
-3.17149249005129,-3.09805189021828,-3.07049681717889,-3.05366894177034,
-3.04851097485566,-3.04525100791085,-3.0422211882679,-3.03828405016965,
-3.03169445596438,-2.98213317121262,-2.90499601432808,-2.88907364817869,
-2.8856282865663,-2.88368652823139,-2.88200701387048,-2.87986075446862,
-2.87642247903201,-2.85769637695237,-2.84740651144653,-2.77524290204827,
-2.74756181080354,-2.73067861535782,-2.72551434636221,-2.72225284941904,
-2.71922330010793,-2.71528891535136,-2.70870922083855,-2.65966344348674,
-2.58364611166234,-2.56622778027109,-2.56269012550498,-2.56072814470679,
-2.55905077458164,-2.55693241659781,-2.55278559079498,-2.52626970400944,
-2.45183508084819,-2.42440177563854,-2.40762658908115,-2.40247403801786,
-2.3992150103115,-2.39618434659084,-2.39224367012597,-2.38564276453107,
-2.33586123923847,-2.25811321899252,-2.24293244070949,-2.23953634468984,
-2.23760525727645,-2.23592401148195,-2.23376118932813,-2.22925246092525,
-2.18727835725855,-2.10664200274483,-2.08540275664059,-2.07981265642086,
-2.07645674546735,-2.07345186214115,-2.06963865725166,-2.06360633982676,
-2.03102102860358,-1.93972231387027,-1.92057209399014,-1.91711005558114,
-1.91495638976978,-1.91327589711605,-1.91133845490602,-1.90791391122118,
-1.89231500458797,-1.81494268268359,-1.7652879232096,-1.75869541543018,
-1.75475692013079,-1.75172629759428,-1.74846570593911,-1.74330726207455,
-1.72648256991856,-1.69893343246994,-1.62520298955981,-1.59810754751318,
-1.59393932164531,-1.59181620342651,-1.59013826432075,-1.58817929600144,
-1.58465630998329,-1.56749261689379,-1.49132017802214,-1.44219083683902,
-1.43560875957085,-1.43167329690249,-1.42864313788405,-1.42538120308981,
-1.4202167090565,-1.40333715081822,-1.37566236463397,-1.37004935497571),
 .UNSPECIFIED.);
#199=B_SPLINE_CURVE_WITH_KNOTS('',3,(#18444,#18445,#18446,#18447,#18448,
#18449,#18450,#18451,#18452,#18453,#18454,#18455,#18456,#18457,#18458,#18459,
#18460,#18461,#18462,#18463,#18464,#18465,#18466,#18467,#18468,#18469,#18470,
#18471,#18472,#18473,#18474,#18475,#18476,#18477,#18478,#18479,#18480,#18481,
#18482,#18483,#18484,#18485,#18486,#18487,#18488,#18489,#18490,#18491,#18492,
#18493,#18494,#18495,#18496,#18497,#18498,#18499,#18500,#18501,#18502,#18503,
#18504,#18505,#18506,#18507,#18508,#18509,#18510,#18511,#18512,#18513,#18514,
#18515,#18516,#18517,#18518,#18519,#18520,#18521,#18522,#18523,#18524,#18525,
#18526,#18527,#18528,#18529,#18530,#18531,#18532,#18533,#18534,#18535,#18536,
#18537,#18538,#18539,#18540,#18541,#18542,#18543,#18544,#18545,#18546,#18547,
#18548,#18549,#18550,#18551,#18552,#18553,#18554,#18555,#18556,#18557,#18558,
#18559,#18560,#18561,#18562,#18563,#18564,#18565,#18566,#18567,#18568,#18569,
#18570,#18571,#18572,#18573,#18574,#18575,#18576,#18577,#18578,#18579,#18580,
#18581,#18582,#18583,#18584,#18585,#18586,#18587,#18588,#18589,#18590,#18591,
#18592,#18593,#18594,#18595,#18596,#18597,#18598,#18599,#18600,#18601,#18602,
#18603,#18604,#18605,#18606,#18607,#18608,#18609,#18610,#18611,#18612,#18613,
#18614,#18615,#18616,#18617,#18618,#18619,#18620,#18621,#18622,#18623,#18624,
#18625,#18626,#18627,#18628,#18629,#18630,#18631,#18632,#18633,#18634,#18635,
#18636,#18637,#18638,#18639,#18640,#18641,#18642,#18643,#18644,#18645,#18646,
#18647,#18648,#18649,#18650,#18651,#18652,#18653,#18654,#18655,#18656,#18657,
#18658,#18659),.UNSPECIFIED.,.F.,.F.,(4,2,2,2,2,2,2,2,2,2,2,2,2,2,2,2,2,
2,2,2,2,2,2,2,2,2,2,2,2,2,2,2,2,2,2,2,2,2,2,2,2,2,2,2,2,2,2,2,2,2,2,2,2,
2,2,2,2,2,2,2,2,2,2,2,2,2,2,2,2,2,2,2,2,2,2,2,2,2,2,2,2,2,2,2,2,2,2,2,2,
2,2,2,2,2,2,2,2,2,2,2,2,2,2,2,2,2,2,4),(-2.69185776365183,-2.69011522243236,
-2.66887324319072,-2.66578991693006,-2.59970034798892,-2.55286621498866,
-2.54260066877817,-2.53833082283421,-2.53525625018545,-2.53245844063289,
-2.52801166844107,-2.51744500526503,-2.43681858930947,-2.38241246471018,
-2.37741566449612,-2.37516066407725,-2.37346863349736,-2.3715910242174,
-2.36843513621108,-2.35769589049127,-2.35462114311805,-2.26430705004553,
-2.23770937025894,-2.22130331938517,-2.21619268735876,-2.21294337196981,
-2.20991004527207,-2.20594917554656,-2.19927726951026,-2.14453930563011,
-2.10359019015327,-2.0582639461155,-2.053956505212,-2.05183387784789,-2.0501565999447,
-2.04819875093182,-2.04477239962098,-2.03083609207311,-1.95379076131783,
-1.90228984726655,-1.89566395175114,-1.89171654248501,-1.88868549094888,
-1.88543075170768,-1.88029497582514,-1.8636632269489,-1.83655074693802,
-1.76056834394419,-1.73495980715647,-1.73084790252123,-1.72873734218499,
-1.72706089257217,-1.72509392070327,-1.72153194599341,-1.70367925176042,
-1.6280315823551,-1.57913246929307,-1.57255679112061,-1.56862398571894,
-1.56559519817769,-1.56233408129141,-1.55716949276554,-1.54027747389885,
-1.51257088787475,-1.44041285476932,-1.43041110572576,-1.4113661222423,
-1.4079107040605,-1.40575947822954,-1.40407980613193,-1.40214211369403,
-1.39871427561739,-1.38305180528749,-1.30576441560168,-1.25609922269104,
-1.24950829419693,-1.24557105796173,-1.24254159773214,-1.23928245321785,
-1.23412673238752,-1.21731510452061,-1.18979262820455,-1.11581588114309,
-1.08891594602433,-1.08475576897062,-1.08263485989711,-1.08095769287635,
-1.07899853584173,-1.07547250829191,-1.05824120998824,-0.982151646551871,
-0.933017011339356,-0.92643659949887,-0.922502418317421,-0.919473422223947,
-0.91621291918644,-0.911051090528244,-0.89418413186103,-0.86653500112858,
-0.793732316900753,-0.765906651706445,-0.761714723678455,-0.759587035115249,
-0.75790935535832,-0.755955170659562,-0.752451970165263,-0.735601654619297,
-0.661806132235414),.UNSPECIFIED.);
#200=B_SPLINE_CURVE_WITH_KNOTS('',3,(#18665,#18666,#18667,#18668,#18669,
#18670,#18671,#18672,#18673,#18674,#18675,#18676,#18677,#18678,#18679,#18680,
#18681,#18682,#18683,#18684,#18685,#18686,#18687,#18688,#18689,#18690,#18691,
#18692,#18693,#18694,#18695,#18696,#18697,#18698,#18699,#18700,#18701,#18702,
#18703,#18704,#18705,#18706,#18707,#18708,#18709,#18710,#18711,#18712,#18713,
#18714,#18715,#18716,#18717,#18718,#18719,#18720,#18721,#18722,#18723,#18724,
#18725,#18726,#18727,#18728,#18729,#18730,#18731,#18732,#18733,#18734,#18735,
#18736,#18737,#18738,#18739,#18740,#18741,#18742,#18743,#18744,#18745,#18746,
#18747,#18748,#18749,#18750,#18751,#18752,#18753,#18754,#18755,#18756,#18757,
#18758,#18759,#18760,#18761,#18762,#18763,#18764,#18765,#18766,#18767,#18768,
#18769,#18770,#18771,#18772,#18773,#18774,#18775,#18776,#18777,#18778,#18779,
#18780,#18781,#18782,#18783,#18784,#18785,#18786,#18787,#18788,#18789,#18790,
#18791,#18792,#18793,#18794,#18795,#18796,#18797,#18798,#18799,#18800,#18801,
#18802,#18803,#18804,#18805,#18806,#18807,#18808,#18809,#18810,#18811,#18812,
#18813,#18814,#18815,#18816,#18817,#18818,#18819,#18820,#18821,#18822,#18823,
#18824,#18825,#18826,#18827,#18828,#18829,#18830,#18831,#18832,#18833,#18834,
#18835,#18836,#18837,#18838,#18839,#18840,#18841,#18842,#18843,#18844,#18845,
#18846,#18847,#18848,#18849,#18850),.UNSPECIFIED.,.F.,.F.,(4,2,2,2,2,2,
2,2,2,2,2,2,2,2,2,2,2,2,2,2,2,2,2,2,2,2,2,2,2,2,2,2,2,2,2,2,2,2,2,2,2,2,
2,2,2,2,2,2,2,2,2,2,2,2,2,2,2,2,2,2,2,2,2,2,2,2,2,2,2,2,2,2,2,2,2,2,2,2,
2,2,2,2,2,2,2,2,2,2,2,2,2,2,4),(-1.36964398461014,-1.30787036768949,-1.25862000725445,
-1.2520356836026,-1.24809963001014,-1.24506945573577,-1.24180793764911,
-1.23664502665887,-1.21977891576258,-1.19213461110797,-1.11932109461955,
-1.09150126983046,-1.08730849104993,-1.08518017131057,-1.08350188516868,
-1.08154683679123,-1.07804166930726,-1.0611734016892,-0.984786360060719,
-0.935552333209351,-0.928968333089632,-0.925032372734004,-0.922002211681342,
-0.918740650150646,-0.913577547455394,-0.896709709080528,-0.869061450526312,
-0.796289558865995,-0.768436007700299,-0.76424211652404,-0.76211355924542,
-0.760435254081098,-0.758480376837962,-0.754975996212281,-0.738120704482538,
-0.661723985771594,-0.612490423452113,-0.605903513901242,-0.601966703963024,
-0.598936408806204,-0.595675214938031,-0.590513785297814,-0.573661179874451,
-0.546047837680169,-0.472918049055438,-0.445352232790946,-0.441167919476765,
-0.439041401817279,-0.437363250721846,-0.435406881119683,-0.431895666438514,
-0.414927493372728,-0.338614211363969,-0.289438801861166,-0.282842694337029,
-0.278903197516473,-0.275872475145974,-0.275744229622131,-0.275663461074198,
-0.275612027540513,-0.275545308692106,-0.275484326182795,-0.27542850359385,
-0.275377333937562,-0.27533036756179,-0.275287207698183,-0.275247502029057,
-0.275210936783149,-0.275177231737833,-0.275146135974347,-0.275117424244362,
-0.275090893867485,-0.275066362062654,-0.275030741949859,-0.274995717425154,
-0.274961269477776,-0.274927379821316,-0.274894030862295,-0.274861205675903,
-0.271315827317332,-0.264820300500427,-0.256683991552925,-0.23908598672357,
-0.20187095921567,-0.125478243713695,-0.119168203703918,-0.116615849001147,
-0.115044020776078,-0.113306101322337,-0.110791914038808,-0.104250209816162,
-0.0699368801188113,-0.00096324508092347),.UNSPECIFIED.);
#201=B_SPLINE_CURVE_WITH_KNOTS('',3,(#18851,#18852,#18853,#18854,#18855,
#18856,#18857,#18858,#18859,#18860,#18861,#18862,#18863,#18864,#18865,#18866,
#18867,#18868,#18869,#18870,#18871,#18872,#18873,#18874,#18875,#18876,#18877,
#18878,#18879,#18880,#18881,#18882,#18883,#18884,#18885,#18886,#18887,#18888,
#18889,#18890,#18891,#18892,#18893,#18894,#18895,#18896,#18897,#18898,#18899,
#18900,#18901,#18902,#18903,#18904,#18905,#18906,#18907,#18908,#18909,#18910,
#18911,#18912,#18913,#18914,#18915,#18916,#18917,#18918,#18919,#18920,#18921,
#18922,#18923,#18924,#18925,#18926,#18927,#18928,#18929,#18930,#18931,#18932,
#18933,#18934,#18935,#18936,#18937,#18938,#18939,#18940,#18941,#18942,#18943,
#18944,#18945,#18946,#18947,#18948,#18949,#18950,#18951,#18952,#18953,#18954,
#18955,#18956,#18957,#18958,#18959,#18960,#18961,#18962,#18963,#18964,#18965,
#18966,#18967,#18968,#18969,#18970,#18971,#18972),.UNSPECIFIED.,.F.,.F.,
(4,2,2,2,2,2,2,2,2,2,2,2,2,2,2,2,2,2,2,2,2,2,2,2,2,2,2,2,2,2,2,2,2,2,2,
2,2,2,2,2,2,2,2,2,2,2,2,2,2,2,2,2,2,2,2,2,2,2,2,2,4),(-4.06096075769659,
-4.02702016228667,-4.02161774880303,-4.01804907544626,-4.01518409485397,
-4.01219364805124,-4.00872859622936,-4.0027979321248,-3.97981170917957,
-3.9607497434034,-3.88878313622104,-3.86163760844338,-3.85584747678854,
-3.8534538355195,-3.85173957147312,-3.85014213452476,-3.84745286779896,
-3.84029096437282,-3.77158348104996,-3.72486017122474,-3.70908029182896,
-3.70155565958667,-3.69544145550076,-3.69199045646421,-3.69196840230189,
-3.69194563088792,-3.69192211695931,-3.69189783427802,-3.69187275351379,
-3.69184684426837,-3.69182008162368,-3.69179243499257,-3.69176387258149,
-3.69173436137362,-3.69170386705747,-3.69167235397824,-3.69163978510591,
-3.6916061219818,-3.6915713246456,-3.69153535089833,-3.69150443643219,-3.69146865913723,
-3.69142724960061,-3.69137931607739,-3.69132382527268,-3.69125958038549,
-3.69120454515646,-3.68817479713999,-3.68423640456368,-3.67764173760504,
-3.6285632828689,-3.55242734410894,-3.53519541240001,-3.53166915373654,
-3.52970986445656,-3.52803256597843,-3.52591144305972,-3.52175067559592,
-3.49483322852289,-3.42095634108256,-3.39991501201283),.UNSPECIFIED.);
#202=B_SPLINE_CURVE_WITH_KNOTS('',3,(#18974,#18975,#18976,#18977,#18978,
#18979,#18980,#18981,#18982,#18983,#18984,#18985,#18986,#18987,#18988,#18989,
#18990,#18991,#18992,#18993,#18994,#18995,#18996,#18997,#18998,#18999,#19000,
#19001,#19002,#19003,#19004,#19005,#19006,#19007,#19008,#19009,#19010,#19011,
#19012,#19013,#19014,#19015,#19016,#19017,#19018,#19019,#19020,#19021,#19022,
#19023,#19024,#19025,#19026,#19027,#19028,#19029,#19030,#19031,#19032,#19033,
#19034,#19035,#19036,#19037,#19038,#19039,#19040,#19041,#19042,#19043,#19044,
#19045,#19046,#19047),.UNSPECIFIED.,.F.,.F.,(4,2,2,2,2,2,2,2,2,2,2,2,2,
2,2,2,2,2,2,2,2,2,2,2,2,2,2,2,2,2,2,2,2,2,2,2,4),(-0.661806132235414,-0.659232099503259,
-0.609956994452256,-0.60337542136454,-0.599440900228318,-0.596411849531053,
-0.593151491739137,-0.587990327919851,-0.571129437951296,-0.543494225960171,
-0.470546102915199,-0.442837739933146,-0.438649694709232,-0.43652283227735,
-0.434845214607481,-0.432890425073598,-0.429384457480762,-0.412488561200852,
-0.336152749283856,-0.286917691182195,-0.280323175420384,-0.276384876704873,
-0.273355229687206,-0.270553938311786,-0.266011484641358,-0.253517352890303,
-0.234974049864926,-0.198665794027236,-0.123059326398487,-0.116682576387896,
-0.114119564698602,-0.112546173871279,-0.110811188703143,-0.108309325613893,
-0.101844355914692,-0.0529083787368607,-0.0009632262016002),
 .UNSPECIFIED.);
#203=B_SPLINE_CURVE_WITH_KNOTS('',3,(#19048,#19049,#19050,#19051,#19052,
#19053,#19054,#19055),.UNSPECIFIED.,.F.,.F.,(4,1,1,1,1,4),(109.955742875643,
110.609869450541,111.609815462892,112.609761475243,113.609707487595,114.192220932897),
 .UNSPECIFIED.);
#204=B_SPLINE_CURVE_WITH_KNOTS('',3,(#19060,#19061,#19062,#19063,#19064,
#19065,#19066,#19067,#19068,#19069,#19070,#19071,#19072,#19073,#19074,#19075,
#19076,#19077,#19078,#19079,#19080,#19081,#19082,#19083,#19084,#19085,#19086,
#19087,#19088,#19089,#19090,#19091,#19092,#19093,#19094,#19095,#19096,#19097,
#19098,#19099,#19100,#19101,#19102,#19103,#19104,#19105,#19106,#19107,#19108,
#19109,#19110,#19111,#19112,#19113,#19114,#19115,#19116,#19117,#19118,#19119,
#19120,#19121,#19122,#19123,#19124,#19125,#19126,#19127,#19128,#19129,#19130,
#19131,#19132,#19133,#19134,#19135,#19136,#19137,#19138,#19139,#19140,#19141,
#19142,#19143,#19144,#19145,#19146,#19147,#19148,#19149,#19150,#19151,#19152,
#19153,#19154,#19155,#19156,#19157,#19158,#19159,#19160,#19161,#19162,#19163,
#19164,#19165,#19166,#19167,#19168,#19169,#19170,#19171,#19172,#19173,#19174,
#19175,#19176,#19177,#19178,#19179,#19180,#19181,#19182,#19183,#19184,#19185,
#19186,#19187,#19188,#19189,#19190,#19191,#19192,#19193,#19194,#19195,#19196,
#19197,#19198,#19199,#19200,#19201,#19202,#19203,#19204,#19205,#19206,#19207,
#19208,#19209,#19210,#19211,#19212,#19213,#19214,#19215,#19216,#19217,#19218,
#19219,#19220,#19221,#19222,#19223,#19224,#19225,#19226,#19227,#19228,#19229,
#19230,#19231,#19232,#19233,#19234,#19235,#19236,#19237,#19238,#19239,#19240,
#19241,#19242,#19243,#19244,#19245,#19246,#19247,#19248,#19249,#19250,#19251,
#19252,#19253,#19254,#19255,#19256,#19257,#19258,#19259,#19260,#19261,#19262,
#19263,#19264,#19265,#19266,#19267,#19268,#19269,#19270,#19271,#19272,#19273,
#19274,#19275,#19276,#19277,#19278,#19279,#19280,#19281,#19282,#19283),
 .UNSPECIFIED.,.F.,.F.,(4,2,2,2,2,2,2,2,2,2,2,2,2,2,2,2,2,2,2,2,2,2,2,2,
2,2,2,2,2,2,2,2,2,2,2,2,2,2,2,2,2,2,2,2,2,2,2,2,2,2,2,2,2,2,2,2,2,2,2,2,
2,2,2,2,2,2,2,2,2,2,2,2,2,2,2,2,2,2,2,2,2,2,2,2,2,2,2,2,2,2,2,2,2,2,2,2,
2,2,2,2,2,2,2,2,2,2,2,2,2,2,2,4),(-3.39957621942377,-3.36840457402077,-3.35166715085571,
-3.34817048919824,-3.34621757395302,-3.34453949102032,-3.34240934561185,
-3.33820666059612,-3.31005425626266,-3.23772473101716,-3.21005985651988,
-3.19318399210446,-3.1880207067793,-3.18475954128355,-3.18173009996059,
-3.17779557179278,-3.17121501276587,-3.12211117812336,-3.0459803515002,
-3.02872615917451,-3.02519827356027,-3.02323848199042,-3.02156100045507,
-3.01943996233688,-3.01528030713941,-2.98840527157683,-2.91445906518644,
-2.88696126161422,-2.87015809802642,-2.86500263108062,-2.86174307153667,
-2.85871282032469,-2.85477396988832,-2.84817896930698,-2.79836212890475,
-2.72053977426467,-2.70545398054485,-2.70206455449886,-2.70013499531584,
-2.69845361887413,-2.6962887114841,-2.69176895887232,-2.64771555107662,
-2.59371778131214,-2.55418936333725,-2.54480517609524,-2.54068580713233,
-2.53763729196339,-2.53480505555941,-2.53092695068876,-2.52113495693993,
-2.4328015752523,-2.41310204462584,-2.38612393470597,-2.38035138889777,
-2.37796006629271,-2.37624566443678,-2.37464667622878,-2.37195182770506,
-2.36475777447206,-2.27243897285695,-2.24220878385379,-2.22423773717541,
-2.21895734552988,-2.21567003355091,-2.21264864466204,-2.20876969365635,
-2.20237959461258,-2.16107688477461,-2.07840245512471,-2.05965259231551,
-2.05604042559745,-2.05406215894052,-2.05238592155259,-2.05028804676869,
-2.04700914838919,-2.03091324113586,-1.95416082996037,-1.9047595121799,
-1.89817218983878,-1.89423526586641,-1.89120496046708,-1.8879438319143,
-1.88278266828884,-1.86593238656111,-1.83832433332555,-1.76514368924867,
-1.7376186902314,-1.73343576532241,-1.73130954748688,-1.72963142370578,
-1.72767484525042,-1.72416265627099,-1.70717818267533,-1.6308771854719,
-1.58168466051326,-1.57510149395278,-1.57116577769228,-1.56813565593813,
-1.56487399031081,-1.55971041075653,-1.54283821829316,-1.51517997197715,
-1.4425154598664,-1.41457483342667,-1.4103780916217,-1.40824892812153,-1.40657057713253,
-1.40461614273153,-1.40111378751317,-1.38429176281064,-1.36964398461014),
 .UNSPECIFIED.);
#205=B_SPLINE_CURVE_WITH_KNOTS('',3,(#19285,#19286,#19287,#19288,#19289,
#19290),.UNSPECIFIED.,.F.,.F.,(4,1,1,4),(114.192220932897,114.609653499946,
115.609599512298,116.238928182823),.UNSPECIFIED.);
#206=B_SPLINE_CURVE_WITH_KNOTS('',3,(#19291,#19292,#19293,#19294,#19295,
#19296,#19297,#19298,#19299,#19300,#19301,#19302,#19303,#19304,#19305,#19306,
#19307,#19308,#19309,#19310,#19311,#19312,#19313,#19314,#19315,#19316,#19317,
#19318,#19319,#19320,#19321,#19322,#19323,#19324,#19325,#19326,#19327,#19328,
#19329,#19330,#19331,#19332,#19333,#19334,#19335,#19336,#19337,#19338,#19339,
#19340,#19341,#19342,#19343,#19344,#19345,#19346,#19347,#19348,#19349,#19350,
#19351,#19352,#19353,#19354,#19355,#19356,#19357,#19358,#19359,#19360,#19361,
#19362,#19363,#19364,#19365,#19366,#19367,#19368,#19369,#19370,#19371,#19372,
#19373,#19374,#19375,#19376,#19377,#19378,#19379,#19380,#19381,#19382,#19383,
#19384,#19385,#19386,#19387,#19388,#19389,#19390,#19391,#19392,#19393,#19394,
#19395,#19396,#19397,#19398,#19399,#19400,#19401,#19402,#19403,#19404,#19405,
#19406,#19407,#19408,#19409,#19410,#19411,#19412,#19413,#19414,#19415,#19416,
#19417,#19418,#19419,#19420,#19421,#19422,#19423,#19424,#19425,#19426,#19427,
#19428,#19429,#19430,#19431,#19432,#19433,#19434,#19435,#19436,#19437,#19438,
#19439,#19440,#19441,#19442,#19443,#19444,#19445,#19446,#19447,#19448,#19449,
#19450,#19451,#19452,#19453,#19454,#19455,#19456,#19457,#19458,#19459,#19460,
#19461,#19462,#19463,#19464,#19465,#19466,#19467,#19468,#19469,#19470,#19471,
#19472,#19473,#19474,#19475,#19476,#19477,#19478,#19479,#19480),
 .UNSPECIFIED.,.F.,.F.,(4,2,2,2,2,2,2,2,2,2,2,2,2,2,2,2,2,2,2,2,2,2,2,2,
2,2,2,2,2,2,2,2,2,2,2,2,2,2,2,2,2,2,2,2,2,2,2,2,2,2,2,2,2,2,2,2,2,2,2,2,
2,2,2,2,2,2,2,2,2,2,2,2,2,2,2,2,2,2,2,2,2,2,2,2,2,2,2,2,2,2,2,2,2,2,4),
(-4.06040871516838,-3.98561996845687,-3.95150132255625,-3.94498018359608,
-3.94246973479271,-3.94073306247043,-3.93916136612688,-3.93660734122501,
-3.93028386314145,-3.85406055927773,-3.81663656903841,-3.79911177686931,
-3.79099999589345,-3.78451420574077,-3.78097493073977,-3.78094221922002,
-3.78090898252618,-3.78087520346131,-3.78084086414446,-3.78080594597525,
-3.78077042959487,-3.78074621756581,-3.78072001943858,-3.78069165202857,
-3.78066091199668,-3.78062757310575,-3.7805913830117,-3.78055205953629,
-3.78050928626375,-3.78046270733438,-3.78041192131598,-3.78035647317105,
-3.78029584627666,-3.7802294546284,-3.78017959401717,-3.78010083951496,
-3.77997499628559,-3.77694531454117,-3.77300702978469,-3.76641261758707,
-3.71738910161496,-3.64145606542709,-3.62394226675987,-3.62039952805431,
-3.61843667768679,-3.61675976645174,-3.61464355992879,-3.61050564369955,
-3.58421685958437,-3.50945136624098,-3.48205857617288,-3.46530159294761,
-3.46015167638995,-3.4568936522188,-3.45386346979838,-3.44992278447107,
-3.44332048862746,-3.39435577650409,-3.31850475123958,-3.3008691130312,
-3.29731921487219,-3.29535474861058,-3.29367789171355,-3.29156358497465,
-3.28743481430705,-3.26139297492324,-3.18542649623018,-3.15863614682001,
-3.14214428787527,-3.13702374619963,-3.13377208554197,-3.13073932471084,
-3.12678314106674,-3.12012791486282,-3.05394667575203,-3.00685862797471,
-2.98770205543889,-2.98047704821159,-2.9752315416193,-2.97293153549146,
-2.97123283850945,-2.96937644408859,-2.96631571418806,-2.9564082552727,
-2.85545011160786,-2.82140468195996,-2.81498172230503,-2.81144413211794,
-2.80875175576088,-2.80529961745094,-2.79942549166939,-2.77707903443562,
-2.7584321187987,-2.6934347578505,-2.69158011258058),.UNSPECIFIED.);
#207=B_SPLINE_CURVE_WITH_KNOTS('',3,(#19486,#19487,#19488,#19489,#19490,
#19491,#19492,#19493,#19494,#19495,#19496,#19497,#19498,#19499,#19500,#19501,
#19502,#19503,#19504,#19505,#19506,#19507,#19508,#19509,#19510,#19511,#19512,
#19513,#19514,#19515,#19516,#19517,#19518,#19519,#19520,#19521,#19522,#19523,
#19524,#19525,#19526,#19527,#19528,#19529,#19530,#19531,#19532,#19533,#19534,
#19535,#19536,#19537,#19538,#19539,#19540,#19541,#19542,#19543,#19544,#19545,
#19546,#19547,#19548,#19549,#19550,#19551,#19552,#19553,#19554,#19555,#19556,
#19557,#19558,#19559,#19560,#19561,#19562,#19563,#19564,#19565,#19566,#19567,
#19568,#19569,#19570,#19571,#19572,#19573,#19574,#19575,#19576,#19577,#19578,
#19579,#19580,#19581,#19582,#19583,#19584,#19585,#19586,#19587,#19588,#19589,
#19590,#19591,#19592,#19593,#19594,#19595,#19596,#19597,#19598,#19599,#19600,
#19601,#19602,#19603,#19604,#19605,#19606,#19607,#19608,#19609,#19610,#19611,
#19612,#19613,#19614,#19615,#19616,#19617,#19618,#19619,#19620,#19621,#19622,
#19623,#19624,#19625,#19626,#19627,#19628,#19629,#19630,#19631,#19632,#19633,
#19634,#19635,#19636,#19637,#19638,#19639),.UNSPECIFIED.,.F.,.F.,(4,2,2,
2,2,2,2,2,2,2,2,2,2,2,2,2,2,2,2,2,2,2,2,2,2,2,2,2,2,2,2,2,2,2,2,2,2,2,2,
2,2,2,2,2,2,2,2,2,2,2,2,2,2,2,2,2,2,2,2,2,2,2,2,2,2,2,2,2,2,2,2,2,2,2,2,
2,4),(-1.37009647383181,-1.36007120758124,-1.33238914503019,-1.25997509255448,
-1.23182677303776,-1.22762319405347,-1.22549253035165,-1.22381400741873,
-1.22186053234231,-1.2183627697852,-1.20161741699309,-1.12513556989821,
-1.07585628150257,-1.06927117945961,-1.06533482674828,-1.06230451934517,
-1.05904295364416,-1.05388017120111,-1.0370163065357,-1.00937754466157,
-0.936493073653841,-0.908727439832827,-0.90453633532472,-0.902408327938482,
-0.900730011415827,-0.898774609752667,-0.895268018965813,-0.878377755431324,
-0.80200383629688,-0.752775629770619,-0.746191544205418,-0.742255486244925,
-0.739225222851115,-0.735963524374353,-0.730800147787975,-0.71393090304407,
-0.686279817812463,-0.620043075587636,-0.607262979997527,-0.58527957811466,
-0.581674570659246,-0.579501484128356,-0.577814948772835,-0.575912393791931,
-0.572645820972912,-0.559502906135828,-0.53401869230696,-0.458125570387648,
-0.44329668618723,-0.440093210829008,-0.425657403656021,-0.420609276839719,
-0.417372941001814,-0.414332837504097,-0.410265374369678,-0.402539003607289,
-0.391838479710758,-0.365907843819049,-0.302577484777825,-0.263031189715583,
-0.258542730139443,-0.256383818323119,-0.254702897566626,-0.252769103630285,
-0.250729654327291,-0.243258628350318,-0.207137910367097,-0.175092905464798,
-0.106765832952291,-0.100163181064056,-0.096221743753303,-0.0931906767397102,
-0.0899313955779809,-0.0847788291937528,-0.0787717256972496,-0.0672476008797058,
-0.000962604047633078),.UNSPECIFIED.);
#208=B_SPLINE_CURVE_WITH_KNOTS('',3,(#19640,#19641,#19642,#19643,#19644,
#19645,#19646,#19647,#19648,#19649,#19650,#19651,#19652,#19653,#19654,#19655,
#19656,#19657,#19658,#19659,#19660,#19661,#19662,#19663,#19664,#19665,#19666,
#19667,#19668,#19669,#19670,#19671,#19672,#19673,#19674,#19675,#19676,#19677,
#19678,#19679,#19680,#19681,#19682,#19683,#19684,#19685,#19686,#19687,#19688,
#19689,#19690,#19691,#19692,#19693,#19694,#19695,#19696,#19697,#19698,#19699,
#19700,#19701,#19702,#19703,#19704,#19705,#19706,#19707,#19708,#19709,#19710,
#19711),.UNSPECIFIED.,.F.,.F.,(4,2,2,2,2,2,2,2,2,2,2,2,2,2,2,2,2,2,2,2,
2,2,2,2,2,2,2,2,2,2,2,2,2,2,2,4),(-4.06018374265953,-3.99925922791561,-3.99609684884804,
-3.99404731745362,-3.99210665623675,-3.99042738853674,-3.98828053155481,
-3.98385106327984,-3.92884133292906,-3.89601345881533,-3.85565089620048,
-3.8391579704278,-3.83399405823387,-3.83073297516012,-3.82770394030177,
-3.82377040811831,-3.8171925455825,-3.76819390702086,-3.69226326691795,
-3.67476651114301,-3.67124089224966,-3.66926603801155,-3.667590045921,-3.66548912856324,
-3.6614224700408,-3.63693574670112,-3.55970402444907,-3.53269462731506,
-3.51616674635414,-3.51100591816946,-3.507745424725,-3.50471600053358,-3.50078063269799,
-3.49419677036822,-3.44491056152456,-3.39957621942377),.UNSPECIFIED.);
#209=B_SPLINE_CURVE_WITH_KNOTS('',3,(#19712,#19713,#19714,#19715,#19716,
#19717,#19718,#19719,#19720,#19721,#19722,#19723,#19724,#19725,#19726,#19727,
#19728,#19729,#19730,#19731,#19732,#19733,#19734,#19735,#19736,#19737,#19738,
#19739,#19740,#19741,#19742,#19743,#19744,#19745,#19746,#19747,#19748,#19749,
#19750,#19751,#19752,#19753,#19754,#19755,#19756,#19757,#19758,#19759,#19760,
#19761,#19762,#19763,#19764,#19765,#19766,#19767,#19768,#19769,#19770,#19771,
#19772,#19773,#19774,#19775,#19776,#19777,#19778,#19779,#19780,#19781,#19782,
#19783,#19784,#19785,#19786,#19787,#19788,#19789,#19790,#19791,#19792,#19793,
#19794,#19795,#19796,#19797,#19798,#19799,#19800,#19801,#19802,#19803,#19804,
#19805,#19806,#19807,#19808,#19809,#19810,#19811,#19812,#19813,#19814,#19815,
#19816,#19817,#19818,#19819,#19820,#19821,#19822,#19823,#19824,#19825,#19826,
#19827,#19828,#19829,#19830,#19831,#19832,#19833,#19834,#19835,#19836,#19837,
#19838,#19839,#19840,#19841,#19842,#19843,#19844,#19845,#19846,#19847,#19848,
#19849,#19850,#19851,#19852,#19853,#19854,#19855,#19856,#19857,#19858,#19859,
#19860,#19861,#19862,#19863,#19864,#19865,#19866,#19867,#19868,#19869,#19870,
#19871,#19872,#19873,#19874,#19875,#19876,#19877,#19878,#19879,#19880,#19881,
#19882,#19883,#19884,#19885,#19886,#19887,#19888,#19889,#19890,#19891,#19892,
#19893,#19894,#19895,#19896,#19897,#19898,#19899,#19900,#19901,#19902,#19903,
#19904,#19905,#19906,#19907,#19908,#19909,#19910,#19911,#19912,#19913,#19914,
#19915,#19916,#19917,#19918,#19919,#19920,#19921,#19922,#19923,#19924,#19925,
#19926,#19927,#19928,#19929,#19930,#19931,#19932,#19933,#19934,#19935,#19936,
#19937,#19938,#19939,#19940,#19941),.UNSPECIFIED.,.F.,.F.,(4,2,2,2,2,2,
2,2,2,2,2,2,2,2,2,2,2,2,2,2,2,2,2,2,2,2,2,2,2,2,2,2,2,2,2,2,2,2,2,2,2,2,
2,2,2,2,2,2,2,2,2,2,2,2,2,2,2,2,2,2,2,2,2,2,2,2,2,2,2,2,2,2,2,2,2,2,2,2,
2,2,2,2,2,2,2,2,2,2,2,2,2,2,2,2,2,2,2,2,2,2,2,2,2,2,2,2,2,2,2,2,2,2,2,2,
4),(-2.69158011258058,-2.66747209160962,-2.65413313474391,-2.65087378958829,
-2.64897332994243,-2.6472872208842,-2.64511289033625,-2.64150211020656,
-2.61940237791487,-2.54942804121769,-2.49935068933227,-2.49236649225764,
-2.48870993803168,-2.48571902440178,-2.48225817200146,-2.4763462828739,
-2.45357720940759,-2.43987264941951,-2.37311790935624,-2.34519909737869,
-2.33121087227542,-2.32790133799036,-2.32598975616248,-2.32430590310611,
-2.32215002397714,-2.31860186046939,-2.29775462982861,-2.28945186031621,
-2.21556297611123,-2.18920249973549,-2.17290226605099,-2.16780376808769,
-2.1645572262376,-2.16152303366808,-2.15755606719589,-2.15086279605703,
-2.08931745444593,-2.03040424951123,-2.00929526812745,-2.00573424087948,
-2.00357456515292,-2.00189026147102,-1.99998099971362,-1.99668198218777,
-1.98283236802072,-1.955341990993,-1.88355481478565,-1.87477445821375,-1.85163947967053,
-1.84569554271565,-1.84222729717398,-1.83923685216028,-1.83558948254433,
-1.82864932423041,-1.7803278063186,-1.70611978857024,-1.68614963516126,
-1.68264534752024,-1.68047938643621,-1.67879829421352,-1.67687031887543,
-1.67348670425153,-1.65847573703791,-1.58065340231378,-1.53079657214752,
-1.52420187538904,-1.52026354006071,-1.51723390660095,-1.5139752371275,
-1.50882167510734,-1.49202963367777,-1.46455195147587,-1.39023152181972,
-1.36359030114698,-1.35943943139079,-1.35732051167427,-1.35564348621507,
-1.35368284235094,-1.35014999158018,-1.33280287108105,-1.25679689637712,
-1.20770503148704,-1.20112546841894,-1.19719153114086,-1.19416256873165,
-1.19090195013919,-1.18573961487041,-1.16886809959988,-1.14120854121272,
-1.06851675826252,-1.04060101605438,-1.03640612562779,-1.03427780417039,
-1.03260007306797,-1.03064634261255,-1.02714523230519,-1.01032934196678,
-0.933934032562123,-0.884649574755044,-0.878066153089346,-0.874131089913014,
-0.871101951019273,-0.867841822392571,-0.862681712024551,-0.845830447507494,
-0.818217309940156,-0.74504688778659,-0.717516456535309,-0.713334374753202,
-0.711208781245367,-0.709531257331113,-0.707575533978588,-0.704065295549147,
-0.687098775447949,-0.661728295761303),.UNSPECIFIED.);
#210=B_SPLINE_CURVE_WITH_KNOTS('',3,(#19946,#19947,#19948,#19949,#19950,
#19951,#19952,#19953,#19954,#19955,#19956,#19957,#19958,#19959,#19960,#19961,
#19962,#19963,#19964,#19965,#19966,#19967,#19968,#19969,#19970,#19971,#19972,
#19973,#19974,#19975,#19976,#19977,#19978,#19979,#19980,#19981,#19982,#19983,
#19984,#19985,#19986,#19987,#19988,#19989,#19990,#19991,#19992,#19993,#19994,
#19995,#19996,#19997,#19998,#19999,#20000,#20001,#20002,#20003,#20004,#20005,
#20006,#20007,#20008,#20009,#20010,#20011,#20012,#20013,#20014,#20015,#20016,
#20017,#20018,#20019,#20020,#20021,#20022,#20023,#20024,#20025,#20026,#20027,
#20028,#20029,#20030,#20031,#20032,#20033,#20034,#20035,#20036,#20037,#20038,
#20039,#20040,#20041,#20042,#20043,#20044,#20045,#20046,#20047,#20048,#20049,
#20050,#20051,#20052,#20053,#20054,#20055,#20056,#20057,#20058,#20059,#20060,
#20061,#20062,#20063,#20064,#20065,#20066,#20067,#20068,#20069,#20070,#20071,
#20072,#20073,#20074,#20075,#20076,#20077,#20078,#20079,#20080,#20081,#20082,
#20083,#20084,#20085,#20086,#20087,#20088,#20089,#20090,#20091,#20092,#20093,
#20094,#20095,#20096,#20097,#20098,#20099,#20100,#20101,#20102,#20103,#20104,
#20105,#20106,#20107,#20108,#20109,#20110,#20111,#20112,#20113,#20114,#20115,
#20116,#20117,#20118,#20119,#20120,#20121,#20122,#20123,#20124,#20125,#20126,
#20127,#20128,#20129,#20130,#20131,#20132,#20133,#20134,#20135,#20136,#20137,
#20138,#20139,#20140,#20141,#20142,#20143,#20144,#20145,#20146,#20147,#20148,
#20149,#20150,#20151,#20152,#20153,#20154,#20155,#20156,#20157,#20158,#20159,
#20160,#20161,#20162,#20163,#20164,#20165,#20166,#20167),.UNSPECIFIED.,
 .F.,.F.,(4,2,2,2,2,2,2,2,2,2,2,2,2,2,2,2,2,2,2,2,2,2,2,2,2,2,2,2,2,2,2,
2,2,2,2,2,2,2,2,2,2,2,2,2,2,2,2,2,2,2,2,2,2,2,2,2,2,2,2,2,2,2,2,2,2,2,2,
2,2,2,2,2,2,2,2,2,2,2,2,2,2,2,2,2,2,2,2,2,2,2,2,2,2,2,2,2,2,2,2,2,2,2,2,
2,2,2,2,2,2,2,4),(-3.39989171054498,-3.37782329442216,-3.35020252442917,
-3.3333459486215,-3.32818481540107,-3.32492414522188,-3.32189456784869,
-3.31795901667933,-3.31137488213135,-3.26208951110153,-3.18558680582082,
-3.16883886382238,-3.16534143070497,-3.16338828577502,-3.16171013045796,
-3.15958005406527,-3.15537799249585,-3.12725035584433,-3.05488510752912,
-3.02722163448309,-3.01034613369993,-3.00518271799666,-3.0019214145189,
-2.99889180664146,-2.99495700769636,-2.98837587584108,-2.9392578410892,
-2.86310012201381,-2.84587672669976,-2.84235053198704,-2.8403910470402,
-2.83871343885712,-2.83659174209633,-2.83242930386336,-2.80548067831588,
-2.73162543526178,-2.70411439915233,-2.68730520105543,-2.68214889754865,
-2.67888904360795,-2.67585868075213,-2.67191991552082,-2.66532556577614,
-2.6155567639682,-2.53787653517198,-2.52261378549417,-2.51921207582781,
-2.51727975436108,-2.51559869340779,-2.51343775810565,-2.50893868465012,
-2.46818773048134,-2.41140556771671,-2.38205791036345,-2.36445764283756,
-2.35921571566852,-2.35593675978992,-2.35291249419321,-2.34901513433722,
-2.34256294487568,-2.29901685157658,-2.23632701948247,-2.21204345611577,
-2.19928316951178,-2.196069996818,-2.19417932781648,-2.19249011501072,-2.19029638201601,
-2.18662086812254,-2.16301729331119,-2.09488224879521,-2.04459631984225,
-2.03760506999759,-2.03394617682264,-2.03124240612375,-2.02788138381756,
-2.02226888935828,-2.00077383956864,-1.92029935513111,-1.87838752279567,
-1.87387849850888,-1.87171550128931,-1.87003410970749,-1.86810282970024,
-1.86470635798594,-1.84952270222907,-1.77181033003987,-1.72203224496142,
-1.71543728631934,-1.71149806854268,-1.70846732314914,-1.70520702538135,
-1.70004995332058,-1.68323782740404,-1.65571748444761,-1.58174623965975,
-1.55483552393685,-1.55067381081448,-1.54855207881564,-1.54687423417808,
-1.54491422198477,-1.54138646819637,-1.52414252396053,-1.44802798268863,
-1.39892782666286,-1.39234630777616,-1.38841099787858,-1.38538085059294,
-1.38211882409639,-1.37695396240566,-1.37009647383181),.UNSPECIFIED.);
#211=B_SPLINE_CURVE_WITH_KNOTS('',3,(#20169,#20170,#20171,#20172,#20173,
#20174,#20175,#20176,#20177,#20178,#20179,#20180,#20181,#20182,#20183,#20184,
#20185,#20186,#20187,#20188,#20189,#20190,#20191,#20192,#20193,#20194,#20195,
#20196,#20197,#20198,#20199,#20200,#20201,#20202,#20203,#20204,#20205,#20206,
#20207,#20208,#20209,#20210,#20211,#20212,#20213,#20214,#20215,#20216,#20217,
#20218,#20219,#20220,#20221,#20222,#20223,#20224,#20225,#20226,#20227,#20228,
#20229,#20230,#20231,#20232,#20233,#20234,#20235,#20236,#20237,#20238,#20239,
#20240,#20241,#20242,#20243,#20244),.UNSPECIFIED.,.F.,.F.,(4,2,2,2,2,2,
2,2,2,2,2,2,2,2,2,2,2,2,2,2,2,2,2,2,2,2,2,2,2,2,2,2,2,2,2,2,2,4),(-0.661728295761303,
-0.610815008485105,-0.561583971244939,-0.555001604028606,-0.5510668437837,
-0.548037746741959,-0.544777474721572,-0.53961673580376,-0.52390332568263,
-0.498367783465112,-0.416315153428545,-0.394074951591542,-0.390453257662493,
-0.388275633138542,-0.386588987397853,-0.384690169563046,-0.381503994986904,
-0.368922016892563,-0.345058087830577,-0.296520050215664,-0.238719470933928,
-0.232031714938196,-0.228066128117626,-0.225031917703408,-0.221784314022387,
-0.216681961847125,-0.200746292228467,-0.156926182370389,-0.122396956235019,
-0.0975934140122743,-0.0713673360125964,-0.0672317821819891,-0.0651161327737426,
-0.0634393244099186,-0.0614761928712398,-0.0593948705733298,-0.0561558460900975,
-0.000961981174542983),.UNSPECIFIED.);
#212=B_SPLINE_CURVE_WITH_KNOTS('',3,(#20245,#20246,#20247,#20248,#20249,
#20250,#20251,#20252,#20253,#20254,#20255,#20256,#20257,#20258,#20259,#20260,
#20261,#20262,#20263,#20264,#20265,#20266,#20267,#20268,#20269,#20270,#20271,
#20272,#20273,#20274,#20275,#20276,#20277,#20278,#20279,#20280,#20281,#20282,
#20283,#20284,#20285,#20286,#20287,#20288,#20289,#20290,#20291,#20292,#20293,
#20294,#20295,#20296,#20297,#20298,#20299,#20300,#20301,#20302,#20303,#20304,
#20305,#20306,#20307,#20308,#20309,#20310,#20311,#20312,#20313,#20314,#20315,
#20316,#20317,#20318,#20319,#20320,#20321,#20322,#20323,#20324,#20325,#20326,
#20327,#20328,#20329,#20330,#20331,#20332,#20333,#20334,#20335,#20336,#20337,
#20338,#20339,#20340,#20341,#20342,#20343,#20344,#20345,#20346,#20347,#20348,
#20349,#20350,#20351,#20352,#20353,#20354,#20355,#20356,#20357,#20358,#20359,
#20360,#20361,#20362,#20363,#20364,#20365,#20366,#20367,#20368,#20369,#20370,
#20371,#20372,#20373,#20374,#20375,#20376,#20377,#20378,#20379,#20380,#20381,
#20382,#20383,#20384,#20385,#20386,#20387,#20388,#20389,#20390),
 .UNSPECIFIED.,.F.,.F.,(4,2,2,2,2,2,2,2,2,2,2,2,2,2,2,2,2,2,2,2,2,2,2,2,
2,2,2,2,2,2,2,2,2,2,2,2,2,2,2,2,2,2,2,2,2,2,2,2,2,2,2,2,2,2,2,2,2,2,2,2,
2,2,2,2,2,2,2,2,2,2,2,2,4),(-4.0611470534665,-3.97946902488515,-3.96965145523291,
-3.9654577117724,-3.96239736646629,-3.95958437074479,-3.95505180491361,
-3.94396228855254,-3.87768596605957,-3.84543925377997,-3.82003258159493,
-3.80692915525169,-3.80376407204218,-3.80183408645674,-3.80015362614578,
-3.79799162283085,-3.79348395991318,-3.75143218553444,-3.67070044832043,
-3.64966864652559,-3.64407023781302,-3.64071349823518,-3.63771050538882,
-3.63390328725673,-3.62788754992851,-3.5955536658021,-3.52072655021728,
-3.49652584640034,-3.48379637841951,-3.48058685021556,-3.47869759037803,
-3.47700914039031,-3.47481578566657,-3.47113962057223,-3.44748897124155,
-3.44120042806564,-3.37026904772027,-3.34267010541243,-3.3258239005242,
-3.3206647980075,-3.31740516913945,-3.31437639905568,-3.31044167737777,
-3.30385847378207,-3.25456398580373,-3.17814277092822,-3.16131673389292,
-3.15781519833253,-3.15586149103941,-3.15418393456454,-3.1520560460983,
-3.14786264167539,-3.11997844918352,-3.04730888222496,-3.01966642328088,
-3.00280093887991,-2.9976395186792,-2.99437925161932,-2.99135045856442,
-2.98741651617018,-2.98083639886609,-2.93171316182019,-2.85564035127376,
-2.8383319726208,-2.83480144026594,-2.83284134603925,-2.8311643319978,-2.82904485085657,
-2.82489115787273,-2.79816557270861,-2.72401104340086,-2.69653098908436,
-2.69214420168212),.UNSPECIFIED.);
#213=B_SPLINE_CURVE_WITH_KNOTS('',3,(#20396,#20397,#20398,#20399,#20400,
#20401,#20402,#20403,#20404,#20405,#20406,#20407,#20408,#20409,#20410,#20411,
#20412,#20413,#20414,#20415,#20416,#20417,#20418,#20419,#20420,#20421,#20422,
#20423,#20424,#20425,#20426,#20427,#20428,#20429,#20430,#20431,#20432,#20433,
#20434,#20435,#20436,#20437,#20438,#20439,#20440,#20441,#20442,#20443,#20444,
#20445,#20446,#20447,#20448,#20449,#20450,#20451,#20452,#20453,#20454,#20455,
#20456,#20457,#20458,#20459,#20460,#20461,#20462,#20463,#20464,#20465,#20466,
#20467,#20468,#20469,#20470,#20471,#20472,#20473,#20474,#20475,#20476,#20477,
#20478,#20479,#20480,#20481,#20482,#20483,#20484,#20485,#20486,#20487,#20488,
#20489,#20490,#20491,#20492,#20493,#20494,#20495,#20496,#20497,#20498,#20499,
#20500,#20501,#20502,#20503,#20504,#20505,#20506,#20507,#20508,#20509,#20510,
#20511,#20512,#20513,#20514,#20515,#20516,#20517,#20518,#20519,#20520,#20521,
#20522,#20523,#20524,#20525,#20526,#20527,#20528,#20529,#20530,#20531,#20532,
#20533,#20534,#20535,#20536,#20537,#20538,#20539,#20540,#20541,#20542,#20543,
#20544,#20545,#20546,#20547,#20548,#20549,#20550,#20551,#20552,#20553),
 .UNSPECIFIED.,.F.,.F.,(4,2,2,2,2,2,2,2,2,2,2,2,2,2,2,2,2,2,2,2,2,2,2,2,
2,2,2,2,2,2,2,2,2,2,2,2,2,2,2,2,2,2,2,2,2,2,2,2,2,2,2,2,2,2,2,2,2,2,2,2,
2,2,2,2,2,2,2,2,2,2,2,2,2,2,2,2,2,2,4),(-1.36944548578019,-1.36685508335615,
-1.36473347674478,-1.36305571269168,-1.3610957732222,-1.35756809666554,
-1.34032346801666,-1.26421357917519,-1.21511627636007,-1.20853507721217,
-1.20459995510823,-1.20156995044009,-1.19830807552231,-1.19314344966717,
-1.17626142839677,-1.1485805305303,-1.07617139302344,-1.04802314847339,
-1.04381972674251,-1.04168915448406,-1.04001070961269,-1.03805733229479,
-1.03455976189052,-1.01781565328565,-0.941337050177608,-0.892059912697068,
-0.885475116329598,-0.881538947322674,-0.878508781914032,-0.875247369609173,
-0.870084831183972,-0.853221774374299,-0.82558434751641,-0.752702894258793,
-0.72493888615982,-0.720747988955342,-0.718620083668117,-0.716941846042953,
-0.714986534434993,-0.711480100500522,-0.69459050339053,-0.618220259872811,
-0.568994407109077,-0.562410631263075,-0.558474758183008,-0.5554446369634,
-0.552183091361504,-0.54701995644478,-0.530475386363742,-0.503428506327888,
-0.427122710844942,-0.422931781795328,-0.401430160587616,-0.397849174516712,
-0.395683167212009,-0.393997521194305,-0.392090769841944,-0.388871213100074,
-0.37589600991404,-0.350913011538589,-0.298584493958666,-0.246080525137938,
-0.239435449672719,-0.235481605811399,-0.232448502934618,-0.229194382385887,
-0.224065533934083,-0.207902223077646,-0.168168060512799,-0.135652290613352,
-0.0791226485939434,-0.0747236304802112,-0.072582301660274,-0.0709029524686051,
-0.0689571617927164,-0.0669006777669633,-0.0637222316588258,-0.0577186424769282,
-0.000962232141326606),.UNSPECIFIED.);
#214=B_SPLINE_CURVE_WITH_KNOTS('',3,(#20554,#20555,#20556,#20557,#20558,
#20559,#20560,#20561,#20562,#20563,#20564,#20565,#20566,#20567,#20568,#20569,
#20570,#20571,#20572,#20573,#20574,#20575,#20576,#20577,#20578,#20579,#20580,
#20581,#20582,#20583,#20584,#20585,#20586,#20587,#20588,#20589,#20590,#20591,
#20592,#20593,#20594,#20595,#20596,#20597,#20598,#20599,#20600,#20601,#20602,
#20603,#20604,#20605,#20606,#20607,#20608,#20609,#20610,#20611,#20612,#20613,
#20614,#20615,#20616,#20617,#20618,#20619,#20620,#20621,#20622,#20623,#20624,
#20625,#20626,#20627,#20628,#20629,#20630,#20631),.UNSPECIFIED.,.F.,.F.,
(4,2,2,2,2,2,2,2,2,2,2,2,2,2,2,2,2,2,2,2,2,2,2,2,2,2,2,2,2,2,2,2,2,2,2,
2,2,2,4),(-4.06105430689023,-3.99656812749712,-3.98512601458802,-3.97914984493825,
-3.97401873272135,-3.97076482823473,-3.96773307376906,-3.96378262465774,
-3.95714683680808,-3.89007832436105,-3.85768781871186,-3.82063014135095,
-3.81320996672058,-3.81117504882215,-3.80924463791343,-3.8075638189508,
-3.80540133333362,-3.80089256753859,-3.7587518252921,-3.6926845608974,-3.65864448390997,
-3.65243664936152,-3.64883446441842,-3.64587376855026,-3.64237746811502,
-3.63631231893072,-3.61173737201564,-3.60453958170595,-3.52710871464621,
-3.50369007507047,-3.4912772988814,-3.48809997677297,-3.48620305720783,
-3.48451584949507,-3.48233457089039,-3.47870065865522,-3.45607474347752,
-3.44128182274636,-3.39989171054498),.UNSPECIFIED.);
#215=B_SPLINE_CURVE_WITH_KNOTS('',3,(#20632,#20633,#20634,#20635,#20636,
#20637,#20638,#20639,#20640,#20641,#20642,#20643,#20644,#20645,#20646,#20647,
#20648,#20649,#20650,#20651,#20652,#20653,#20654,#20655,#20656,#20657,#20658,
#20659,#20660,#20661,#20662,#20663,#20664,#20665,#20666,#20667,#20668,#20669,
#20670,#20671,#20672,#20673,#20674,#20675,#20676,#20677,#20678,#20679,#20680,
#20681,#20682,#20683,#20684,#20685,#20686,#20687,#20688,#20689,#20690,#20691,
#20692,#20693,#20694,#20695,#20696,#20697,#20698,#20699,#20700,#20701,#20702,
#20703,#20704,#20705,#20706,#20707,#20708,#20709,#20710,#20711,#20712,#20713,
#20714,#20715,#20716,#20717,#20718,#20719,#20720,#20721,#20722,#20723,#20724,
#20725,#20726,#20727,#20728,#20729,#20730,#20731,#20732,#20733,#20734,#20735,
#20736,#20737,#20738,#20739,#20740,#20741,#20742,#20743,#20744,#20745,#20746,
#20747,#20748,#20749,#20750,#20751,#20752,#20753,#20754,#20755,#20756,#20757,
#20758,#20759,#20760,#20761,#20762,#20763,#20764,#20765,#20766,#20767,#20768,
#20769,#20770,#20771,#20772,#20773,#20774,#20775,#20776,#20777,#20778,#20779,
#20780,#20781,#20782,#20783,#20784,#20785,#20786,#20787,#20788,#20789,#20790,
#20791,#20792,#20793,#20794,#20795,#20796,#20797,#20798,#20799,#20800,#20801,
#20802,#20803,#20804,#20805,#20806,#20807,#20808,#20809,#20810,#20811,#20812,
#20813,#20814,#20815,#20816,#20817,#20818,#20819,#20820,#20821,#20822,#20823,
#20824,#20825,#20826,#20827,#20828,#20829,#20830,#20831,#20832,#20833,#20834,
#20835,#20836,#20837,#20838,#20839,#20840,#20841,#20842,#20843,#20844,#20845,
#20846,#20847,#20848,#20849,#20850,#20851,#20852,#20853,#20854,#20855,#20856,
#20857,#20858,#20859),.UNSPECIFIED.,.F.,.F.,(4,2,2,2,2,2,2,2,2,2,2,2,2,
2,2,2,2,2,2,2,2,2,2,2,2,2,2,2,2,2,2,2,2,2,2,2,2,2,2,2,2,2,2,2,2,2,2,2,2,
2,2,2,2,2,2,2,2,2,2,2,2,2,2,2,2,2,2,2,2,2,2,2,2,2,2,2,2,2,2,2,2,2,2,2,2,
2,2,2,2,2,2,2,2,2,2,2,2,2,2,2,2,2,2,2,2,2,2,2,2,2,2,2,2,4),(-2.69214420168212,
-2.67973619593171,-2.67458237891731,-2.67132367241898,-2.66829408939555,
-2.66435593831008,-2.65776176172773,-2.60794407083172,-2.53025102046682,
-2.51503192846507,-2.51163384492198,-2.50970265456142,-2.50802199066382,
-2.50586083304291,-2.50135877979141,-2.46015665689658,-2.38130797234107,
-2.3578388945831,-2.35206644839734,-2.34867078894003,-2.34567322123776,
-2.34192642209654,-2.33610951900337,-2.30713797266868,-2.23214079973542,
-2.20535490684935,-2.19173899336989,-2.18845774434828,-2.18655233387126,
-2.1848671016102,-2.18270068842031,-2.1791171198563,-2.15754520488519,-2.14989323317005,
-2.0761138376243,-2.03997334956528,-2.03102968730414,-2.02703378172422,
-2.0239946422948,-2.02075938775664,-2.01571307773361,-1.99986899625076,
-1.97451931270814,-1.9242454105774,-1.89328683005485,-1.87007736772437,
-1.86641892233116,-1.8642305854261,-1.86254260764619,-1.86065007199541,
-1.85742661802092,-1.84453263428126,-1.81986795164492,-1.75735563355225,
-1.71421223308437,-1.7077728497534,-1.70387992384522,-1.70085716260779,
-1.69757790696673,-1.69233131702317,-1.67467623005482,-1.64519178392337,
-1.58758527717084,-1.54777307596717,-1.54328317919534,-1.54112445325438,
-1.53944409350665,-1.53751144687149,-1.53410651735475,-1.51878504810215,
-1.44122176624357,-1.39145478805498,-1.38486193147988,-1.38092416016115,
-1.37789464827414,-1.37463580237969,-1.36948130772471,-1.35268040125277,
-1.32518230094414,-1.25101802340827,-1.22426124465494,-1.22010623719456,
-1.21798644952337,-1.2163093833264,-1.21434943739582,-1.21081971592342,
-1.19352525392567,-1.11748255282312,-1.06837193429881,-1.06179207486316,
-1.05785808011058,-1.0548291434526,-1.05156862154496,-1.04640658638491,
-1.0295373699114,-1.00188292407963,-0.929141443246179,-0.901267290284923,
-0.897073809129345,-0.894945805419274,-0.893268120518162,-0.891314209286817,
-0.887812192822024,-0.870980835262293,-0.794598309860886,-0.745320093665881,
-0.738736875909263,-0.734801900745541,-0.731772809806856,-0.728512713298485,
-0.723352612227376,-0.706501006252207,-0.678886930515555,-0.662304444938604),
 .UNSPECIFIED.);
#216=B_SPLINE_CURVE_WITH_KNOTS('',3,(#20864,#20865,#20866,#20867,#20868,
#20869,#20870,#20871,#20872,#20873,#20874,#20875,#20876,#20877,#20878,#20879,
#20880,#20881,#20882,#20883,#20884,#20885,#20886,#20887,#20888,#20889,#20890,
#20891,#20892,#20893,#20894,#20895,#20896,#20897,#20898,#20899,#20900,#20901,
#20902,#20903,#20904,#20905,#20906,#20907,#20908,#20909,#20910,#20911,#20912,
#20913,#20914,#20915,#20916,#20917,#20918,#20919,#20920,#20921,#20922,#20923,
#20924,#20925,#20926,#20927,#20928,#20929,#20930,#20931,#20932,#20933,#20934,
#20935,#20936,#20937,#20938,#20939,#20940,#20941,#20942,#20943,#20944,#20945,
#20946,#20947,#20948,#20949,#20950,#20951,#20952,#20953,#20954,#20955,#20956,
#20957,#20958,#20959,#20960,#20961,#20962,#20963,#20964,#20965,#20966,#20967,
#20968,#20969,#20970,#20971,#20972,#20973,#20974,#20975,#20976,#20977,#20978,
#20979,#20980,#20981,#20982,#20983,#20984,#20985,#20986,#20987,#20988,#20989,
#20990,#20991,#20992,#20993,#20994,#20995,#20996,#20997,#20998,#20999,#21000,
#21001,#21002,#21003,#21004,#21005,#21006,#21007,#21008,#21009,#21010,#21011,
#21012,#21013,#21014,#21015,#21016,#21017,#21018,#21019,#21020,#21021,#21022,
#21023,#21024,#21025,#21026,#21027,#21028,#21029,#21030,#21031,#21032,#21033,
#21034,#21035,#21036,#21037,#21038,#21039,#21040,#21041,#21042,#21043,#21044,
#21045,#21046,#21047,#21048,#21049,#21050,#21051,#21052,#21053,#21054,#21055,
#21056,#21057,#21058,#21059,#21060,#21061,#21062,#21063,#21064,#21065,#21066,
#21067,#21068,#21069,#21070,#21071,#21072,#21073),.UNSPECIFIED.,.F.,.F.,
(4,2,2,2,2,2,2,2,2,2,2,2,2,2,2,2,2,2,2,2,2,2,2,2,2,2,2,2,2,2,2,2,2,2,2,
2,2,2,2,2,2,2,2,2,2,2,2,2,2,2,2,2,2,2,2,2,2,2,2,2,2,2,2,2,2,2,2,2,2,2,2,
2,2,2,2,2,2,2,2,2,2,2,2,2,2,2,2,2,2,2,2,2,2,2,2,2,2,2,2,2,2,2,2,2,4),(-3.39921582738553,
-3.32481449484858,-3.30797204107994,-3.30446916420648,-3.30251498590862,
-3.30083718732464,-3.29870916466968,-3.29451599472769,-3.26664925628896,
-3.19397761073236,-3.1663465501906,-3.1494858161877,-3.14432445482504,-3.14106388128885,
-3.13803455985473,-3.13409957702268,-3.12751691295561,-3.0782858165178,
-3.00189575808859,-2.98500486145439,-2.98149889632078,-2.97954397315815,
-2.9778661408787,-2.97573885432162,-2.97154948562348,-2.94380391627405,
-2.87097584465458,-2.84335764833016,-2.8265022422895,-2.82134126972633,
-2.81808065552759,-2.81505109875404,-2.81111552974511,-2.80453126707731,
-2.75523674437102,-2.67871415564775,-2.66199391026287,-2.65849819775023,
-2.65654543973425,-2.65486726016679,-2.65273669366933,-2.64853227368191,
-2.62032987930118,-2.54805679372162,-2.52038554596727,-2.50350669964811,
-2.49834294745525,-2.49508158963164,-2.49205204038094,-2.48811747241642,
-2.48153706788515,-2.43245266483799,-2.3563606378107,-2.33904762085849,
-2.33551616421612,-2.33355554550493,-2.33187806631487,-2.32975794052694,
-2.32560279115239,-2.29885712373006,-2.22473481912716,-2.19725827844759,
-2.18046421850513,-2.17530961896144,-2.1720501625438,-2.16901969944224,
-2.1650801360264,-2.15848297600417,-2.10856767226204,-2.03044723688045,
-2.01597481920901,-2.01250315737895,-2.01053455404231,-2.00885767955125,
-2.00674778779779,-2.00250568674842,-1.96247756126698,-1.89318044936584,
-1.86030054312869,-1.85425101246816,-1.85043251301819,-1.84742698875623,
-1.8440740303073,-1.83849748626483,-1.81741498603992,-1.73660164759996,
-1.6945550508575,-1.69004526258722,-1.68788217634461,-1.68620084491157,
-1.68426977978387,-1.6808740325054,-1.66569931345358,-1.5879837647268,-1.53820564997236,
-1.53161095427254,-1.52767190776974,-1.52464130245084,-1.52138116353253,
-1.5162243601143,-1.49941326497488,-1.47189476671748,-1.39792253642723,
-1.37101648029654,-1.36944548578019),.UNSPECIFIED.);
#217=B_SPLINE_CURVE_WITH_KNOTS('',3,(#21075,#21076,#21077,#21078,#21079,
#21080,#21081,#21082,#21083,#21084,#21085,#21086,#21087,#21088,#21089,#21090,
#21091,#21092,#21093,#21094,#21095,#21096,#21097,#21098,#21099,#21100,#21101,
#21102,#21103,#21104,#21105,#21106,#21107,#21108,#21109,#21110,#21111,#21112,
#21113,#21114,#21115,#21116,#21117,#21118,#21119,#21120,#21121,#21122,#21123,
#21124,#21125,#21126,#21127,#21128,#21129,#21130,#21131,#21132,#21133,#21134,
#21135,#21136,#21137,#21138,#21139,#21140,#21141,#21142,#21143,#21144,#21145,
#21146,#21147,#21148,#21149,#21150),.UNSPECIFIED.,.F.,.F.,(4,2,2,2,2,2,
2,2,2,2,2,2,2,2,2,2,2,2,2,2,2,2,2,2,2,2,2,2,2,2,2,2,2,2,2,2,2,4),(-0.662304444938604,
-0.63510021468167,-0.578477873728376,-0.574082661913293,-0.571942617297102,
-0.570264008758051,-0.568318804463193,-0.565099959077751,-0.551433987379965,
-0.524294500285268,-0.446054304749311,-0.420452860529858,-0.414309608485123,
-0.4107957026584,-0.408106194423922,-0.404633303173324,-0.398985520822482,
-0.374703149293996,-0.291094634145217,-0.255474777269919,-0.251032176228322,
-0.248882730945909,-0.247203238869721,-0.245264380807548,-0.243217478816965,
-0.235647647195005,-0.196108431693412,-0.162561834215048,-0.142574300536187,
-0.0990487023498325,-0.0925986579080474,-0.0887025324900113,-0.0856792144300964,
-0.0824012833215487,-0.0790422999552084,-0.0741458825853799,-0.0566546994879453,
-0.00096234511667658),.UNSPECIFIED.);
#218=B_SPLINE_CURVE_WITH_KNOTS('',3,(#21151,#21152,#21153,#21154,#21155,
#21156,#21157,#21158,#21159,#21160,#21161,#21162,#21163,#21164,#21165,#21166,
#21167,#21168,#21169,#21170,#21171,#21172,#21173,#21174,#21175,#21176,#21177,
#21178,#21179,#21180,#21181,#21182,#21183,#21184,#21185,#21186,#21187,#21188,
#21189,#21190,#21191,#21192,#21193,#21194,#21195,#21196,#21197,#21198,#21199,
#21200,#21201,#21202,#21203,#21204,#21205,#21206,#21207,#21208,#21209,#21210,
#21211,#21212,#21213,#21214,#21215,#21216,#21217,#21218,#21219,#21220,#21221,
#21222,#21223,#21224,#21225,#21226,#21227,#21228,#21229,#21230,#21231,#21232,
#21233,#21234,#21235,#21236,#21237,#21238,#21239,#21240,#21241,#21242,#21243,
#21244,#21245,#21246,#21247,#21248,#21249,#21250,#21251,#21252,#21253,#21254,
#21255,#21256,#21257,#21258,#21259,#21260,#21261,#21262,#21263,#21264,#21265,
#21266,#21267,#21268,#21269,#21270,#21271,#21272,#21273,#21274,#21275,#21276,
#21277,#21278,#21279,#21280,#21281,#21282,#21283,#21284,#21285,#21286,#21287,
#21288,#21289,#21290,#21291,#21292,#21293,#21294,#21295,#21296,#21297,#21298,
#21299,#21300,#21301,#21302,#21303,#21304),.UNSPECIFIED.,.F.,.F.,(4,2,2,
2,2,2,2,2,2,2,2,2,2,2,2,2,2,2,2,2,2,2,2,2,2,2,2,2,2,2,2,2,2,2,2,2,2,2,2,
2,2,2,2,2,2,2,2,2,2,2,2,2,2,2,2,2,2,2,2,2,2,2,2,2,2,2,2,2,2,2,2,2,2,2,2,
2,4),(-4.06007593280828,-3.99508670064763,-3.99042194715341,-3.98776077535643,
-3.98538711376223,-3.98367662841544,-3.98207435650221,-3.97935938264497,
-3.9720265854057,-3.91556034035554,-3.8827315202545,-3.83998657274542,-3.82975634765789,
-3.82642509712098,-3.82316636481412,-3.82013759582651,-3.81620169374451,
-3.80961390953123,-3.76006666597922,-3.70094237722576,-3.67857286962766,
-3.66653741920305,-3.66339613799091,-3.66150782191981,-3.65981929132283,
-3.6576246250592,-3.65394369652287,-3.63017141919948,-3.62397508904615,
-3.54783538865922,-3.52360536853894,-3.50833632884403,-3.50347413144518,
-3.50021467130849,-3.49718620563316,-3.49325208901566,-3.48667035960177,
-3.43742539958884,-3.36110525559634,-3.34415337328646,-3.34064443200445,
-3.3386892137869,-3.33701198197228,-3.33488658932606,-3.33070438709033,
-3.30314862482051,-3.2300802790426,-3.20247969303012,-3.18563290730004,
-3.18047383514902,-3.17721427347346,-3.17418559895685,-3.17025104847686,
-3.16366823498459,-3.11438531399867,-3.03798766474525,-3.02113336432045,
-3.01763018167405,-3.0156761491635,-3.01399868145626,-3.01187137883828,
-3.00768055820981,-2.97987210006679,-2.90711205193522,-2.87947911680082,
-2.86261792626382,-2.85745707334647,-2.85419699258987,-2.85116825392184,
-2.84723421370144,-2.84065356166726,-2.79149557310213,-2.71535395356781,
-2.69814409994251,-2.69461945246054,-2.69266067310163,-2.69180502268216),
 .UNSPECIFIED.);
#219=B_SPLINE_CURVE_WITH_KNOTS('',3,(#21310,#21311,#21312,#21313,#21314,
#21315,#21316,#21317,#21318,#21319,#21320,#21321,#21322,#21323,#21324,#21325,
#21326,#21327,#21328,#21329,#21330,#21331,#21332,#21333,#21334,#21335,#21336,
#21337,#21338,#21339,#21340,#21341,#21342,#21343,#21344,#21345,#21346,#21347,
#21348,#21349,#21350,#21351,#21352,#21353,#21354,#21355,#21356,#21357,#21358,
#21359,#21360,#21361,#21362,#21363,#21364,#21365,#21366,#21367,#21368,#21369,
#21370,#21371,#21372,#21373,#21374,#21375,#21376,#21377,#21378,#21379,#21380,
#21381,#21382,#21383,#21384,#21385,#21386,#21387,#21388,#21389,#21390,#21391,
#21392,#21393,#21394,#21395,#21396,#21397,#21398,#21399,#21400,#21401,#21402,
#21403,#21404,#21405,#21406,#21407,#21408,#21409,#21410,#21411,#21412,#21413,
#21414,#21415,#21416,#21417,#21418,#21419,#21420,#21421,#21422,#21423,#21424,
#21425,#21426,#21427,#21428,#21429,#21430,#21431,#21432,#21433,#21434,#21435,
#21436,#21437,#21438,#21439,#21440,#21441,#21442,#21443,#21444,#21445,#21446,
#21447,#21448,#21449,#21450,#21451,#21452,#21453,#21454,#21455,#21456,#21457,
#21458,#21459,#21460,#21461,#21462,#21463,#21464,#21465,#21466,#21467,#21468,
#21469,#21470,#21471,#21472,#21473,#21474,#21475,#21476,#21477,#21478,#21479,
#21480,#21481,#21482,#21483,#21484,#21485,#21486,#21487,#21488,#21489,#21490,
#21491,#21492,#21493,#21494,#21495,#21496,#21497,#21498,#21499,#21500,#21501,
#21502,#21503,#21504,#21505,#21506,#21507,#21508,#21509,#21510,#21511,#21512,
#21513),.UNSPECIFIED.,.F.,.F.,(4,2,2,2,2,2,2,2,2,2,2,2,2,2,2,2,2,2,2,2,
2,2,2,2,2,2,2,2,2,2,2,2,2,2,2,2,2,2,2,2,2,2,2,2,2,2,2,2,2,2,2,2,2,2,2,2,
2,2,2,2,2,2,2,2,2,2,2,2,2,2,2,2,2,2,2,2,2,2,2,2,2,2,2,2,2,2,2,2,2,2,2,2,
2,2,2,2,2,2,2,2,2,4),(-1.37015241264804,-1.35570167221927,-1.34911020280277,
-1.34517184391813,-1.34214104368373,-1.33887998266,-1.33372020388906,-1.31688586729512,
-1.28931555875076,-1.21574475579553,-1.18851814157379,-1.18434507533776,
-1.18222082213135,-1.18054267426951,-1.17858425479071,-1.17506423658523,
-1.15795382549888,-1.08173522975928,-1.032581929931,-1.02599891416521,-1.02206301295249,
-1.01903258795034,-1.01577043744264,-1.01060575243728,-0.99372691981051,
-0.966054700086884,-0.893500726404919,-0.865460163196997,-0.861259800617952,
-0.859129726214254,-0.857451132930531,-0.855496962431575,-0.851996434210784,
-0.835208971356298,-0.758751733720428,-0.709504648386363,-0.702907312120488,
-0.698967235220946,-0.695936156354818,-0.69267582199739,-0.687519377516122,
-0.670715408820021,-0.643214620991501,-0.569065739521207,-0.542282788116421,
-0.538125382693541,-0.536004469917919,-0.534326558392875,-0.53236564356778,
-0.528834197182952,-0.511531168312921,-0.435452029791617,-0.386395765008376,
-0.379799368310777,-0.375859550998606,-0.37282849579225,-0.372756962554819,
-0.372695205486438,-0.37264188380147,-0.372595840334254,-0.372556076881171,
-0.372521732658634,-0.372492065480112,-0.372456341309402,-0.372421787924555,
-0.372388362413708,-0.372356024898909,-0.372324737004946,-0.37229446180026,
-0.372265163735355,-0.372236808603881,-0.372209363485444,-0.372182796719788,
-0.37215707782998,-0.37213217978693,-0.372108076696769,-0.372084737184498,
-0.372062135128295,-0.372040245393113,-0.368586703197645,-0.362467433708289,
-0.354934034015112,-0.339130344809145,-0.292302260847055,-0.223613311847423,
-0.216443223500477,-0.213751925897575,-0.212153567805215,-0.210438561239818,
-0.208044291725156,-0.202254565889217,-0.175127893333119,-0.104932832839247,
-0.0858200753755365,-0.0613244148699548,-0.0552638180302682,-0.0517678051873036,
-0.0488059839202267,-0.0459509476860365,-0.0424235859125755,-0.0371219143882906,
-0.000961528038556079),.UNSPECIFIED.);
#220=B_SPLINE_CURVE_WITH_KNOTS('',3,(#21514,#21515,#21516,#21517,#21518,
#21519,#21520,#21521,#21522,#21523,#21524,#21525,#21526,#21527,#21528,#21529,
#21530,#21531,#21532,#21533,#21534,#21535,#21536,#21537,#21538,#21539,#21540,
#21541,#21542,#21543,#21544,#21545,#21546,#21547,#21548,#21549,#21550,#21551,
#21552,#21553,#21554,#21555,#21556,#21557,#21558,#21559,#21560,#21561,#21562,
#21563,#21564,#21565,#21566,#21567,#21568,#21569,#21570,#21571,#21572,#21573,
#21574,#21575,#21576,#21577,#21578,#21579,#21580,#21581,#21582,#21583,#21584,
#21585,#21586,#21587),.UNSPECIFIED.,.F.,.F.,(4,2,2,2,2,2,2,2,2,2,2,2,2,
2,2,2,2,2,2,2,2,2,2,2,2,2,2,2,2,2,2,2,2,2,2,2,4),(-4.0598307301908,-4.03672959654851,
-3.95835106002174,-3.95188085665108,-3.94937832677973,-3.94764332351265,
-3.94607023270309,-3.9435082940285,-3.93713708709772,-3.86158186525947,
-3.82533930506727,-3.8068002885785,-3.79430707685316,-3.78976557777166,
-3.78696446288447,-3.78393493284727,-3.77999677157192,-3.77340237704567,
-3.72417508750641,-3.6477441627003,-3.63092268536297,-3.62742123393807,
-3.6254674383618,-3.62378971257453,-3.62166145320441,-3.61746682253874,
-3.58954942267503,-3.5169466966478,-3.48931127062046,-3.47244892089151,
-3.46728758094606,-3.46402713981489,-3.46099802341706,-3.45706342335037,
-3.45048165609643,-3.40123518122251,-3.39921582738553),.UNSPECIFIED.);
#221=B_SPLINE_CURVE_WITH_KNOTS('',3,(#21588,#21589,#21590,#21591,#21592,
#21593,#21594,#21595,#21596,#21597,#21598,#21599,#21600,#21601,#21602,#21603,
#21604,#21605,#21606,#21607,#21608,#21609,#21610,#21611,#21612,#21613,#21614,
#21615,#21616,#21617,#21618,#21619,#21620,#21621,#21622,#21623,#21624,#21625,
#21626,#21627,#21628,#21629,#21630,#21631,#21632,#21633,#21634,#21635,#21636,
#21637,#21638,#21639,#21640,#21641,#21642,#21643,#21644,#21645,#21646,#21647,
#21648,#21649,#21650,#21651,#21652,#21653,#21654,#21655,#21656,#21657,#21658,
#21659,#21660,#21661,#21662,#21663,#21664,#21665,#21666,#21667,#21668,#21669,
#21670,#21671,#21672,#21673,#21674,#21675,#21676,#21677,#21678,#21679,#21680,
#21681,#21682,#21683,#21684,#21685,#21686,#21687,#21688,#21689,#21690,#21691,
#21692,#21693,#21694,#21695,#21696,#21697,#21698,#21699,#21700,#21701,#21702,
#21703,#21704,#21705,#21706,#21707,#21708,#21709,#21710,#21711,#21712,#21713,
#21714,#21715,#21716,#21717,#21718,#21719,#21720,#21721,#21722,#21723,#21724,
#21725,#21726,#21727,#21728,#21729,#21730,#21731,#21732,#21733,#21734,#21735,
#21736,#21737,#21738,#21739,#21740,#21741,#21742,#21743,#21744,#21745,#21746,
#21747,#21748,#21749,#21750,#21751,#21752,#21753,#21754,#21755,#21756,#21757,
#21758,#21759,#21760,#21761,#21762,#21763,#21764,#21765,#21766,#21767,#21768,
#21769,#21770,#21771,#21772,#21773,#21774,#21775,#21776,#21777,#21778,#21779,
#21780,#21781,#21782,#21783,#21784,#21785,#21786,#21787,#21788,#21789,#21790,
#21791,#21792,#21793,#21794,#21795,#21796,#21797,#21798,#21799,#21800,#21801,
#21802,#21803,#21804,#21805),.UNSPECIFIED.,.F.,.F.,(4,2,2,2,2,2,2,2,2,2,
2,2,2,2,2,2,2,2,2,2,2,2,2,2,2,2,2,2,2,2,2,2,2,2,2,2,2,2,2,2,2,2,2,2,2,2,
2,2,2,2,2,2,2,2,2,2,2,2,2,2,2,2,2,2,2,2,2,2,2,2,2,2,2,2,2,2,2,2,2,2,2,2,
2,2,2,2,2,2,2,2,2,2,2,2,2,2,2,2,2,2,2,2,2,2,2,2,2,2,4),(-2.69180502268216,
-2.69098358363705,-2.68886246929761,-2.68470097689536,-2.6577549091569,
-2.58389478623317,-2.55637814733146,-2.5395674861602,-2.53441201103297,
-2.53115299800168,-2.52812364253832,-2.52418651570319,-2.51759566115706,
-2.46793923265734,-2.39068125422341,-2.37493000085803,-2.37149626078189,
-2.36955727521549,-2.3678777726856,-2.36572845901756,-2.36128660196571,
-2.32521766519254,-2.26256970565054,-2.23393241278596,-2.21663605089012,
-2.21142748729118,-2.20815658155172,-2.20513100478276,-2.2012197036306,
-2.19471781410534,-2.14917658715137,-2.08156441301318,-2.06214658048509,
-2.05485433177623,-2.04957085857689,-2.04726416463708,-2.04556448048204,
-2.04371115668083,-2.04066395643112,-2.03086934245073,-1.95121836060041,
-1.89744691537271,-1.89078577967483,-1.88682805874426,-1.88379528173221,
-1.88054473992063,-1.87542835743921,-1.85897088566994,-1.83225328723325,
-1.75640354428838,-1.73009268910162,-1.72595389450485,-1.72383752417177,
-1.72216063304425,-1.72019796947154,-1.71665599776122,-1.69915378515835,
-1.62325628349064,-1.57422088611227,-1.56764228836061,-1.56370857108618,
-1.56067956920271,-1.55741870232406,-1.55225553513478,-1.53537736598037,
-1.50770288505918,-1.43516336059359,-1.40712092096809,-1.40292181085711,
-1.40079255368937,-1.39911470404518,-1.39716154604376,-1.39366322321443,
-1.37689424866944,-1.30046125112015,-1.25115863798108,-1.2445746865456,
-1.24063940859038,-1.23761016390584,-1.2343499800531,-1.22918990720931,
-1.21233988340498,-1.18472991746882,-1.11151823182696,-1.08401810062982,
-1.07983694701505,-1.07771151444344,-1.07603395721322,-1.07407801063294,
-1.07056691228205,-1.05358735349408,-0.977310537189237,-0.928082510657953,
-0.921500035257714,-0.91756518284616,-0.914535998778254,-0.911275617259664,
-0.906114671276844,-0.889256780249801,-0.861628813866283,-0.78859483489283,
-0.760952521356919,-0.756766570732481,-0.754640112795603,-0.752962474562208,
-0.751007270713667,-0.747499589186207,-0.730576758887035,-0.661807984799128),
 .UNSPECIFIED.);
#222=B_SPLINE_CURVE_WITH_KNOTS('',3,(#21810,#21811,#21812,#21813,#21814,
#21815,#21816,#21817,#21818,#21819,#21820,#21821,#21822,#21823,#21824,#21825,
#21826,#21827,#21828,#21829,#21830,#21831,#21832,#21833,#21834,#21835,#21836,
#21837,#21838,#21839,#21840,#21841,#21842,#21843,#21844,#21845,#21846,#21847,
#21848,#21849,#21850,#21851,#21852,#21853,#21854,#21855,#21856,#21857,#21858,
#21859,#21860,#21861,#21862,#21863,#21864,#21865,#21866,#21867,#21868,#21869,
#21870,#21871,#21872,#21873,#21874,#21875,#21876,#21877,#21878,#21879,#21880,
#21881,#21882,#21883,#21884,#21885,#21886,#21887,#21888,#21889,#21890,#21891,
#21892,#21893,#21894,#21895,#21896,#21897,#21898,#21899,#21900,#21901,#21902,
#21903,#21904,#21905,#21906,#21907,#21908,#21909,#21910,#21911,#21912,#21913,
#21914,#21915,#21916,#21917,#21918,#21919,#21920,#21921,#21922,#21923,#21924,
#21925,#21926,#21927,#21928,#21929,#21930,#21931,#21932,#21933,#21934,#21935,
#21936,#21937,#21938,#21939,#21940,#21941,#21942,#21943,#21944,#21945,#21946,
#21947,#21948,#21949,#21950,#21951,#21952,#21953,#21954,#21955,#21956,#21957,
#21958,#21959,#21960,#21961,#21962,#21963,#21964,#21965,#21966,#21967,#21968,
#21969,#21970,#21971,#21972,#21973,#21974,#21975,#21976,#21977,#21978,#21979,
#21980,#21981,#21982,#21983,#21984,#21985,#21986,#21987,#21988,#21989,#21990,
#21991,#21992,#21993,#21994,#21995,#21996,#21997,#21998,#21999,#22000,#22001,
#22002,#22003,#22004,#22005,#22006,#22007,#22008,#22009,#22010,#22011,#22012,
#22013,#22014,#22015,#22016,#22017,#22018,#22019,#22020,#22021,#22022,#22023),
 .UNSPECIFIED.,.F.,.F.,(4,2,2,2,2,2,2,2,2,2,2,2,2,2,2,2,2,2,2,2,2,2,2,2,
2,2,2,2,2,2,2,2,2,2,2,2,2,2,2,2,2,2,2,2,2,2,2,2,2,2,2,2,2,2,2,2,2,2,2,2,
2,2,2,2,2,2,2,2,2,2,2,2,2,2,2,2,2,2,2,2,2,2,2,2,2,2,2,2,2,2,2,2,2,2,2,2,
2,2,2,2,2,2,2,2,2,2,4),(-3.40023537643569,-3.33482078185619,-3.30719486950161,
-3.29033523387914,-3.28517320247625,-3.28191197376044,-3.27888188358579,
-3.27494567499668,-3.26836045983183,-3.21906860335362,-3.1425569306785,
-3.12580076494813,-3.12230240871166,-3.12034886027345,-3.11867042783018,
-3.11654008924492,-3.1123377816331,-3.08421993346944,-3.01182460862819,
-2.98415801707282,-2.96728033953895,-2.96211612285055,-2.95885428238125,
-2.95582415422582,-2.95188864913119,-2.94530626920494,-2.89617337285961,
-2.81998983409003,-2.80278126440513,-2.79925552182887,-2.79729593292003,
-2.79561801718591,-2.7934956514125,-2.78933106242006,-2.76233708521128,
-2.68852255018912,-2.66100033844717,-2.64418544131733,-2.63902794809165,
-2.63576747103202,-2.63273661807035,-2.62879734251646,-2.62220241790063,
-2.57245296636962,-2.49483755632898,-2.47947731681429,-2.47606857340942,
-2.47413450500865,-2.47245336709749,-2.47029422017985,-2.46580539845458,
-2.4262386953559,-2.36847625742542,-2.33896598030259,-2.32129602970495,
-2.31604619892625,-2.3127651407173,-2.30974086132929,-2.30584617027375,
-2.29940420549618,-2.25626330165687,-2.19386345910526,-2.16905381699869,
-2.1561088099532,-2.15288002433365,-2.1509856900146,-2.14929700013531,-2.14710888804055,
-2.14345323594964,-2.12034146941491,-2.10962599753095,-2.03152314379028,
-2.02122744771306,-1.99944375006007,-1.99361917422242,-1.99017733836269,
-1.98718316977388,-1.9834975552179,-1.97637918050148,-1.9200651726639,-1.85963851291728,
-1.83458282172232,-1.83049138590502,-1.82838461643966,-1.8267076302322,
-1.82473587112967,-1.82115458829943,-1.80297942502917,-1.72618180678269,
-1.67871268495384,-1.67216469347124,-1.66823897361453,-1.66521007514229,
-1.66194332995739,-1.65675802400204,-1.6396911344249,-1.6115862890577,-1.54671124652989,
-1.51195632735406,-1.50752256950061,-1.50537423955513,-1.50369411251794,
-1.50175277797187,-1.49831093281251,-1.48245266118319,-1.40528043645708,
-1.37015241264804),.UNSPECIFIED.);
#223=B_SPLINE_CURVE_WITH_KNOTS('',3,(#22025,#22026,#22027,#22028,#22029,
#22030,#22031,#22032,#22033,#22034,#22035,#22036,#22037,#22038,#22039,#22040,
#22041,#22042,#22043,#22044,#22045,#22046,#22047,#22048,#22049,#22050,#22051,
#22052,#22053,#22054,#22055,#22056,#22057,#22058,#22059,#22060,#22061,#22062,
#22063,#22064,#22065,#22066,#22067,#22068,#22069,#22070,#22071,#22072,#22073,
#22074,#22075,#22076,#22077,#22078,#22079,#22080,#22081,#22082,#22083,#22084,
#22085,#22086,#22087,#22088,#22089,#22090,#22091,#22092,#22093,#22094,#22095,
#22096,#22097,#22098,#22099,#22100),.UNSPECIFIED.,.F.,.F.,(4,2,2,2,2,2,
2,2,2,2,2,2,2,2,2,2,2,2,2,2,2,2,2,2,2,2,2,2,2,2,2,2,2,2,2,2,2,4),(-0.661807984799128,
-0.654257869818397,-0.605014980974329,-0.598429031543051,-0.594493162276247,
-0.591463814719946,-0.58820386700501,-0.583044906843026,-0.566205126427913,
-0.538618671574585,-0.468140561817124,-0.462130454299904,-0.437689929728706,
-0.433625192760907,-0.431524767779201,-0.429848909425109,-0.42787393520875,
-0.424275166859475,-0.405758519692253,-0.325536566182482,-0.281740120617086,
-0.275267094480029,-0.271364303988575,-0.268340089133171,-0.265538401924824,
-0.261004058170068,-0.248366526641298,-0.22953730751555,-0.193035807796621,
-0.118118298295534,-0.111729377774037,-0.10916430395282,-0.107590514978991,
-0.105855895048481,-0.103355943930342,-0.096903514059749,-0.0634855304692036,
-0.000963188783679523),.UNSPECIFIED.);
#224=B_SPLINE_CURVE_WITH_KNOTS('',3,(#22101,#22102,#22103,#22104,#22105,
#22106,#22107,#22108,#22109,#22110,#22111,#22112,#22113,#22114,#22115,#22116,
#22117,#22118,#22119,#22120,#22121,#22122,#22123,#22124,#22125,#22126,#22127,
#22128,#22129,#22130,#22131,#22132,#22133,#22134,#22135,#22136,#22137,#22138,
#22139,#22140,#22141,#22142,#22143,#22144,#22145,#22146,#22147,#22148,#22149,
#22150,#22151,#22152,#22153,#22154,#22155,#22156,#22157,#22158,#22159,#22160,
#22161,#22162,#22163,#22164,#22165,#22166,#22167,#22168,#22169,#22170,#22171,
#22172,#22173,#22174,#22175,#22176,#22177,#22178,#22179,#22180,#22181,#22182,
#22183,#22184,#22185,#22186,#22187,#22188,#22189,#22190,#22191,#22192,#22193,
#22194,#22195,#22196,#22197,#22198,#22199,#22200,#22201,#22202,#22203,#22204,
#22205,#22206,#22207,#22208,#22209,#22210,#22211,#22212,#22213,#22214,#22215,
#22216,#22217,#22218,#22219,#22220,#22221,#22222,#22223,#22224,#22225,#22226,
#22227,#22228,#22229,#22230,#22231,#22232,#22233,#22234,#22235,#22236,#22237,
#22238,#22239,#22240,#22241,#22242,#22243,#22244,#22245,#22246,#22247,#22248,
#22249,#22250,#22251,#22252,#22253,#22254,#22255,#22256,#22257,#22258,#22259,
#22260,#22261,#22262,#22263,#22264),.UNSPECIFIED.,.F.,.F.,(4,2,2,2,2,2,
2,2,2,2,2,2,2,2,2,2,2,2,2,2,2,2,2,2,2,2,2,2,2,2,2,2,2,2,2,2,2,2,2,2,2,2,
2,2,2,2,2,2,2,2,2,2,2,2,2,2,2,2,2,2,2,2,2,2,2,2,2,2,2,2,2,2,2,2,2,2,2,2,
2,2,2,4),(-4.0614287578822,-4.03248871540076,-4.01846104360662,-4.01365489798641,
-4.01033316269565,-4.00752181880818,-4.00452327004274,-4.0007622030692,
-3.99489804196461,-3.96524899606189,-3.94584283611108,-3.88111634163756,
-3.85452293802728,-3.84879489543677,-3.84641168900244,-3.84469933804932,
-3.84309929440734,-3.84039647146944,-3.8331451375629,-3.77212380131558,
-3.72144008924457,-3.70353835756497,-3.69530252279819,-3.68872717556511,
-3.68517352177786,-3.68247422333838,-3.67909297441338,-3.67338468946435,
-3.65345836652772,-3.55643899838608,-3.53774678690756,-3.53064256320669,
-3.52546566485076,-3.52317800715839,-3.52148127783768,-3.5196194663786,
-3.51653417352629,-3.50641678134479,-3.50451420221678,-3.41361908352743,
-3.38615026898234,-3.36936041640254,-3.36420716022018,-3.36094858742808,
-3.35791897603315,-3.35398057099992,-3.34738549014509,-3.29815696099868,
-3.22183041738727,-3.20486364478017,-3.2013533191308,-3.1993975661187,-3.19772002182691,
-3.19559442110385,-3.19141237522778,-3.16388011103469,-3.09076122624934,
-3.06315893043958,-3.04631045962763,-3.04115055523152,-3.03789039483268,
-3.03486111368623,-3.03092570368943,-3.02434129471597,-2.97503329712059,
-2.89858817553595,-2.8817742661767,-2.87827305475125,-2.87631921920786,
-2.87464136090194,-2.87251284295468,-2.86831745264589,-2.84038932807227,
-2.76775598971946,-2.74010440623786,-2.72323413696449,-2.71807163743497,
-2.71481077727113,-2.71178149438938,-2.70784700259689,-2.70126615755269,
-2.69232820337898),.UNSPECIFIED.);
#225=B_SPLINE_CURVE_WITH_KNOTS('',3,(#22270,#22271,#22272,#22273,#22274,
#22275,#22276,#22277,#22278),.UNSPECIFIED.,.F.,.F.,(4,1,1,1,1,1,4),(160.22122533308,
160.306526627267,161.306472639618,162.306418651969,163.306364664321,164.306310676672,
164.458927396546),.UNSPECIFIED.);
#226=B_SPLINE_CURVE_WITH_KNOTS('',3,(#22279,#22280,#22281,#22282,#22283,
#22284,#22285,#22286,#22287,#22288,#22289,#22290,#22291,#22292,#22293,#22294,
#22295,#22296,#22297,#22298,#22299,#22300,#22301,#22302,#22303,#22304,#22305,
#22306,#22307,#22308,#22309,#22310,#22311,#22312,#22313,#22314,#22315,#22316,
#22317,#22318,#22319,#22320,#22321,#22322,#22323,#22324,#22325,#22326,#22327,
#22328,#22329,#22330,#22331,#22332,#22333,#22334,#22335,#22336,#22337,#22338,
#22339,#22340,#22341,#22342,#22343,#22344,#22345,#22346,#22347,#22348,#22349,
#22350,#22351,#22352,#22353,#22354),.UNSPECIFIED.,.F.,.F.,(4,2,2,2,2,2,
2,2,2,2,2,2,2,2,2,2,2,2,2,2,2,2,2,2,2,2,2,2,2,2,2,2,2,2,2,2,2,4),(-4.0614630673581,
-4.05235423870892,-3.96283840444798,-3.93777252469754,-3.93188013811726,
-3.92845778818342,-3.92546300471007,-3.92175396700727,-3.91606035920602,
-3.88902746696132,-3.8050304357142,-3.78310043186638,-3.77517962828362,
-3.77130702260846,-3.76816909778494,-3.76629336885218,-3.76469327318415,
-3.76255009404327,-3.75814060112062,-3.7020680575884,-3.65787276096341,
-3.6302390214585,-3.6133762570027,-3.60821407922187,-3.60495294503442,-3.60192307173183,
-3.59798732806223,-3.59140329432733,-3.54215389317604,-3.4657303365375,
-3.44886309154659,-3.44535811526621,-3.44340319417903,-3.44172502335401,
-3.43959686996878,-3.43540447334862,-3.40763336833459,-3.40023537643569),
 .UNSPECIFIED.);
#227=B_SPLINE_CURVE_WITH_KNOTS('',3,(#22355,#22356,#22357,#22358,#22359,
#22360,#22361,#22362,#22363,#22364,#22365,#22366,#22367,#22368,#22369,#22370,
#22371,#22372,#22373,#22374,#22375,#22376,#22377,#22378,#22379,#22380,#22381,
#22382,#22383,#22384,#22385,#22386,#22387,#22388,#22389,#22390,#22391,#22392,
#22393,#22394,#22395,#22396,#22397,#22398,#22399,#22400,#22401,#22402,#22403,
#22404,#22405,#22406,#22407,#22408,#22409,#22410,#22411,#22412,#22413,#22414,
#22415,#22416,#22417,#22418,#22419,#22420,#22421,#22422,#22423,#22424,#22425,
#22426,#22427,#22428,#22429,#22430,#22431,#22432,#22433,#22434,#22435,#22436,
#22437,#22438,#22439,#22440,#22441,#22442,#22443,#22444,#22445,#22446,#22447,
#22448,#22449,#22450,#22451,#22452,#22453,#22454,#22455,#22456,#22457,#22458,
#22459,#22460,#22461,#22462,#22463,#22464,#22465,#22466,#22467,#22468,#22469,
#22470,#22471,#22472,#22473,#22474,#22475,#22476,#22477,#22478,#22479,#22480,
#22481,#22482,#22483,#22484,#22485,#22486,#22487,#22488,#22489,#22490,#22491,
#22492,#22493,#22494,#22495,#22496,#22497,#22498,#22499,#22500,#22501,#22502,
#22503,#22504,#22505,#22506,#22507,#22508,#22509,#22510,#22511,#22512,#22513,
#22514,#22515,#22516,#22517,#22518,#22519,#22520,#22521,#22522,#22523,#22524,
#22525,#22526,#22527,#22528,#22529,#22530,#22531,#22532,#22533,#22534,#22535,
#22536,#22537,#22538,#22539,#22540,#22541,#22542,#22543,#22544,#22545,#22546,
#22547,#22548,#22549,#22550,#22551,#22552,#22553,#22554,#22555,#22556,#22557,
#22558,#22559,#22560,#22561,#22562,#22563,#22564,#22565,#22566),
 .UNSPECIFIED.,.F.,.F.,(4,2,2,2,2,2,2,2,2,2,2,2,2,2,2,2,2,2,2,2,2,2,2,2,
2,2,2,2,2,2,2,2,2,2,2,2,2,2,2,2,2,2,2,2,2,2,2,2,2,2,2,2,2,2,2,2,2,2,2,2,
2,2,2,2,2,2,2,2,2,2,2,2,2,2,2,2,2,2,2,2,2,2,2,2,2,2,2,2,2,2,2,2,2,2,2,2,
2,2,2,2,2,2,2,2,2,4),(-2.69232820337898,-2.65215331755146,-2.57610388787892,
-2.55874252190226,-2.55520845908299,-2.55324739746129,-2.55157016471346,
-2.54945118635699,-2.5453008033091,-2.51868116942949,-2.44436574494018,
-2.41690138391812,-2.40011266218735,-2.39495896467106,-2.391699930452,-2.38866976400286,
-2.38473045818825,-2.37813347333805,-2.32868997370835,-2.25191573891669,
-2.23552390746872,-2.23204851955261,-2.23010018678417,-2.22842149070606,
-2.22628472487605,-2.22287778578281,-2.20478565495202,-2.1045602781164,
-2.07843784358157,-2.07247131749459,-2.06903277073797,-2.06603972630721,
-2.06235328025359,-2.05673239951629,-2.03080471296937,-1.97580982653872,
-1.94588728187544,-1.93779308354745,-1.9134451694628,-1.90938428253259,
-1.90728467757254,-1.90560885148976,-1.90363318936277,-1.90003129527163,
-1.88145719932781,-1.80063827631087,-1.7574399740288,-1.75099908058603,
-1.74710571190354,-1.7440828863301,-1.74080384074389,-1.73555819605331,
-1.71791208240507,-1.68844885628179,-1.63096870377777,-1.59100057425755,
-1.58650919985396,-1.58435018577139,-1.5826697993837,-1.5807373452675,-1.57733328749,
-1.56202461388756,-1.48445088468712,-1.43468019637624,-1.42808727138658,
-1.42414948173725,-1.42111996890225,-1.41786113492771,-1.41270668666146,
-1.39590617689815,-1.36840897502444,-1.29423806712174,-1.26748633929008,
-1.26333151633647,-1.2612117690953,-1.25953470699639,-1.25757473367821,
-1.25404488214976,-1.23674817735237,-1.16070716478711,-1.11159742061136,
-1.10501758302102,-1.10108359618052,-1.09805466260356,-1.0947941410465,
-1.08963210011751,-1.07276280810492,-1.04510818063073,-0.972368929468456,
-0.944493035068862,-0.940299499291466,-0.938171484898872,-0.936493800339113,
-0.934539899570493,-0.931037926828355,-0.914207256388892,-0.837824288323109,
-0.788545872915298,-0.781962655556508,-0.778027682083294,-0.774998593294991,
-0.771738499937146,-0.766578405634705,-0.749726837719345,-0.7221128406229,
-0.662156536932336),.UNSPECIFIED.);
#228=B_SPLINE_CURVE_WITH_KNOTS('',3,(#22572,#22573,#22574,#22575,#22576,
#22577,#22578,#22579,#22580,#22581,#22582,#22583,#22584,#22585,#22586,#22587,
#22588,#22589,#22590,#22591,#22592,#22593,#22594,#22595,#22596,#22597,#22598,
#22599,#22600,#22601,#22602,#22603,#22604,#22605,#22606,#22607,#22608,#22609,
#22610,#22611,#22612,#22613,#22614,#22615,#22616,#22617,#22618,#22619,#22620,
#22621,#22622,#22623,#22624,#22625,#22626,#22627,#22628,#22629,#22630,#22631,
#22632,#22633,#22634,#22635,#22636,#22637,#22638,#22639,#22640,#22641,#22642,
#22643,#22644,#22645,#22646,#22647,#22648,#22649,#22650,#22651,#22652,#22653,
#22654,#22655,#22656,#22657,#22658,#22659,#22660,#22661,#22662,#22663,#22664,
#22665,#22666,#22667,#22668,#22669,#22670,#22671,#22672,#22673,#22674,#22675,
#22676,#22677,#22678,#22679,#22680,#22681,#22682,#22683,#22684,#22685,#22686,
#22687,#22688,#22689,#22690,#22691,#22692,#22693,#22694,#22695,#22696,#22697,
#22698,#22699,#22700,#22701,#22702,#22703,#22704,#22705,#22706,#22707,#22708,
#22709,#22710,#22711,#22712,#22713,#22714,#22715,#22716,#22717,#22718,#22719),
 .UNSPECIFIED.,.F.,.F.,(4,2,2,2,2,2,2,2,2,2,2,2,2,2,2,2,2,2,2,2,2,2,2,2,
2,2,2,2,2,2,2,2,2,2,2,2,2,2,2,2,2,2,2,2,2,2,2,2,2,2,2,2,2,2,2,2,2,2,2,2,
2,2,2,2,2,2,2,2,2,2,2,2,2,4),(-1.37008796384114,-1.36509452139955,-1.33756705120965,
-1.26368343230619,-1.23671424426907,-1.23255080247012,-1.2304288356845,
-1.22875114013694,-1.22679168817352,-1.22326591239097,-1.20605080402931,
-1.12992498236679,-1.08081976705881,-1.07423874891923,-1.070303803348,-1.06727397461942,
-1.06401232857066,-1.05884814934947,-1.0419683457706,-1.01429186311723,
-0.941855362331853,-0.913734708695746,-0.909532372698914,-0.907402106931502,
-0.905723776584494,-0.903770385711698,-0.900272435613842,-0.883519770475412,
-0.807052768490655,-0.757781920452373,-0.751197573840573,-0.747261652086498,
-0.744231664359939,-0.740970430796123,-0.735808148573984,-0.718945687248358,
-0.691308980812469,-0.620870374069518,-0.614969858323678,-0.590479109974328,
-0.586411585532371,-0.584310240216116,-0.582633918546744,-0.580658681749976,
-0.577060132417265,-0.558559337013442,-0.478501477509581,-0.468039787372866,
-0.433871639893346,-0.42776519906544,-0.423929513645285,-0.420922167846103,
-0.417579260091554,-0.412047651623141,-0.391792315100057,-0.310341290712693,
-0.26802602034066,-0.263514571034847,-0.261351215984343,-0.259669921488299,
-0.257739175796078,-0.254573477874679,-0.241479782206959,-0.216107046963393,
-0.183560071733502,-0.117597596727701,-0.106504907451117,-0.101970548454938,
-0.0991562778078226,-0.0960944020792617,-0.0918983056610401,-0.087252618025963,
-0.0792406479124629,-0.000962876874443607),.UNSPECIFIED.);
#229=B_SPLINE_CURVE_WITH_KNOTS('',3,(#22720,#22721,#22722,#22723,#22724,
#22725),.UNSPECIFIED.,.F.,.F.,(4,1,1,4),(164.458927396546,165.306256689024,
166.306202701375,166.504410640259),.UNSPECIFIED.);
#230=B_SPLINE_CURVE_WITH_KNOTS('',3,(#22727,#22728,#22729,#22730,#22731,
#22732,#22733,#22734,#22735,#22736,#22737,#22738,#22739,#22740,#22741,#22742,
#22743,#22744,#22745,#22746,#22747,#22748,#22749,#22750,#22751,#22752,#22753,
#22754,#22755,#22756,#22757,#22758,#22759,#22760,#22761,#22762,#22763,#22764,
#22765,#22766,#22767,#22768,#22769,#22770,#22771,#22772,#22773,#22774,#22775,
#22776,#22777,#22778,#22779,#22780,#22781,#22782,#22783,#22784,#22785,#22786,
#22787,#22788,#22789,#22790,#22791,#22792,#22793,#22794,#22795,#22796,#22797,
#22798,#22799,#22800,#22801,#22802,#22803,#22804,#22805,#22806,#22807,#22808,
#22809,#22810,#22811,#22812,#22813,#22814),.UNSPECIFIED.,.F.,.F.,(4,2,2,
2,2,2,2,2,2,2,2,2,2,2,2,2,2,2,2,2,2,2,2,2,2,2,2,2,2,2,2,2,2,2,2,2,2,2,2,
2,2,2,2,4),(-0.662156536932336,-0.648956013746852,-0.621418192193571,-0.617234499775957,
-0.615108581233505,-0.613431055280487,-0.611475622140756,-0.607966632969675,
-0.591020215921372,-0.514722936640716,-0.465485531341795,-0.458903121030178,
-0.454968378544555,-0.451939320614257,-0.448679115744897,-0.443518536519126,
-0.426662623721119,-0.399038694208074,-0.355194168524487,-0.298655849376382,
-0.294253481146245,-0.292112018854427,-0.290433286732513,-0.290426632483179,
-0.290420084506535,-0.290413640687297,-0.290407299018121,-0.290401057478961,
-0.2903949140909,-0.288474887817562,-0.285144057785002,-0.280975459144695,
-0.272195312542459,-0.246600417983609,-0.184345430883523,-0.142200987206802,
-0.135789521101596,-0.13190488755513,-0.128883447241603,-0.125600486147694,
-0.120336747935594,-0.102516454894325,-0.0726393233951299,-0.000963379534404715),
 .UNSPECIFIED.);
#231=B_SPLINE_CURVE_WITH_KNOTS('',3,(#22815,#22816,#22817,#22818,#22819,
#22820,#22821,#22822,#22823,#22824,#22825,#22826,#22827,#22828,#22829,#22830,
#22831,#22832,#22833,#22834,#22835,#22836,#22837,#22838,#22839,#22840,#22841,
#22842,#22843,#22844,#22845,#22846,#22847,#22848,#22849,#22850,#22851,#22852,
#22853,#22854,#22855,#22856,#22857,#22858,#22859,#22860,#22861,#22862,#22863,
#22864,#22865,#22866,#22867,#22868,#22869,#22870,#22871,#22872,#22873,#22874,
#22875,#22876,#22877,#22878,#22879,#22880,#22881,#22882,#22883,#22884,#22885,
#22886,#22887,#22888,#22889,#22890,#22891,#22892,#22893,#22894,#22895,#22896,
#22897,#22898,#22899,#22900,#22901,#22902,#22903,#22904,#22905,#22906,#22907,
#22908,#22909,#22910,#22911,#22912,#22913,#22914,#22915,#22916,#22917,#22918,
#22919,#22920,#22921,#22922,#22923,#22924,#22925,#22926,#22927,#22928,#22929,
#22930,#22931,#22932,#22933,#22934,#22935,#22936,#22937,#22938,#22939,#22940,
#22941,#22942,#22943,#22944,#22945,#22946,#22947,#22948,#22949,#22950,#22951,
#22952,#22953,#22954,#22955,#22956,#22957,#22958,#22959,#22960,#22961,#22962,
#22963,#22964,#22965,#22966,#22967,#22968,#22969,#22970,#22971,#22972,#22973,
#22974,#22975,#22976,#22977,#22978,#22979,#22980,#22981,#22982),
 .UNSPECIFIED.,.F.,.F.,(4,2,2,2,2,2,2,2,2,2,2,2,2,2,2,2,2,2,2,2,2,2,2,2,
2,2,2,2,2,2,2,2,2,2,2,2,2,2,2,2,2,2,2,2,2,2,2,2,2,2,2,2,2,2,2,2,2,2,2,2,
2,2,2,2,2,2,2,2,2,2,2,2,2,2,2,2,2,2,2,2,2,2,2,4),(-4.06137411129811,-4.03546814208168,
-4.03260936723115,-4.03068543622094,-4.02910207865154,-4.02742394594966,
-4.02528765473165,-4.02188101107949,-4.00378125912536,-3.99087511127817,
-3.92336215122477,-3.89390000861074,-3.87625324670922,-3.87100804923103,
-3.86772941140725,-3.86470704756532,-3.86081439142151,-3.85437488405435,
-3.81121148531092,-3.74866773042392,-3.72400495439522,-3.71543798804153,
-3.71134229651865,-3.70803197674221,-3.70613041934244,-3.70612544828196,
-3.70612044883366,-3.70611542078261,-3.70443560804051,-3.70228077409685,
-3.69780993954386,-3.64539408540266,-3.5975998397588,-3.5699879776209,-3.55313585729943,
-3.54797591462403,-3.5447159788346,-3.5416870780946,-3.53775240607612,-3.53116976900817,
-3.48191981090553,-3.40559298472915,-3.38863278312118,-3.38512298134602,
-3.38316740373971,-3.38148993761662,-3.37936434319125,-3.3751820310455,
-3.34763695028034,-3.27453969815414,-3.24693700621568,-3.23008860856498,
-3.22492888144925,-3.2216688687451,-3.21863974945762,-3.21470458469248,
-3.20812066303947,-3.15882272722111,-3.08239739921846,-3.06556304272006,
-3.06206071391739,-3.06010669570504,-3.05842895425275,-3.05630093644398,
-3.05210759438145,-3.02423685725316,-2.95153830415818,-2.92389457450066,
-2.90702798083542,-2.90186605690893,-2.89860543385016,-2.89557628398828,
-2.89164184114217,-2.88506080525283,-2.83592398160934,-2.75982708098895,
-2.74253790851482,-2.73900821643197,-2.73704816754924,-2.73537093391692,
-2.73325084441166,-2.72909497053658,-2.70231907556713,-2.69288841829231),
 .UNSPECIFIED.);
#232=B_SPLINE_CURVE_WITH_KNOTS('',3,(#22987,#22988,#22989,#22990,#22991,
#22992,#22993,#22994,#22995,#22996,#22997,#22998,#22999,#23000,#23001,#23002,
#23003,#23004,#23005,#23006,#23007,#23008,#23009,#23010,#23011,#23012,#23013,
#23014,#23015,#23016,#23017,#23018,#23019,#23020,#23021,#23022,#23023,#23024,
#23025,#23026,#23027,#23028,#23029,#23030,#23031,#23032,#23033,#23034,#23035,
#23036,#23037,#23038,#23039,#23040,#23041,#23042,#23043,#23044,#23045,#23046,
#23047,#23048,#23049,#23050,#23051,#23052,#23053,#23054,#23055,#23056,#23057,
#23058,#23059,#23060,#23061,#23062,#23063,#23064,#23065,#23066,#23067,#23068,
#23069,#23070,#23071,#23072,#23073,#23074,#23075,#23076,#23077,#23078,#23079,
#23080,#23081,#23082,#23083,#23084,#23085,#23086,#23087,#23088,#23089,#23090,
#23091,#23092,#23093,#23094,#23095,#23096,#23097,#23098,#23099,#23100,#23101,
#23102,#23103,#23104,#23105,#23106,#23107,#23108,#23109,#23110,#23111,#23112,
#23113,#23114,#23115,#23116,#23117,#23118,#23119,#23120,#23121,#23122,#23123,
#23124,#23125,#23126,#23127,#23128,#23129,#23130,#23131,#23132,#23133,#23134,
#23135,#23136,#23137,#23138,#23139,#23140,#23141,#23142,#23143,#23144,#23145,
#23146,#23147,#23148,#23149,#23150,#23151,#23152,#23153,#23154,#23155,#23156,
#23157,#23158,#23159,#23160,#23161,#23162,#23163,#23164,#23165,#23166,#23167,
#23168,#23169,#23170,#23171,#23172,#23173,#23174,#23175,#23176,#23177,#23178,
#23179,#23180,#23181,#23182,#23183,#23184,#23185,#23186,#23187,#23188,#23189,
#23190,#23191,#23192,#23193,#23194,#23195,#23196,#23197,#23198,#23199,#23200,
#23201,#23202,#23203,#23204,#23205,#23206,#23207,#23208,#23209,#23210),
 .UNSPECIFIED.,.F.,.F.,(4,2,2,2,2,2,2,2,2,2,2,2,2,2,2,2,2,2,2,2,2,2,2,2,
2,2,2,2,2,2,2,2,2,2,2,2,2,2,2,2,2,2,2,2,2,2,2,2,2,2,2,2,2,2,2,2,2,2,2,2,
2,2,2,2,2,2,2,2,2,2,2,2,2,2,2,2,2,2,2,2,2,2,2,2,2,2,2,2,2,2,2,2,2,2,2,2,
2,2,2,2,2,2,2,2,2,2,2,2,2,2,2,4),(-3.39966608106449,-3.38261128349882,-3.35497570774651,
-3.338113451604,-3.33295200935335,-3.32969146948553,-3.32666223742753,-3.32272745345153,
-3.31614531186498,-3.26694168136053,-3.1907099101825,-3.17363514114318,
-3.17011842316367,-3.16816131401051,-3.16648402352849,-3.16436051743969,
-3.16018776103442,-3.13291633050984,-3.05949811623182,-3.03194119663903,
-3.01511328560141,-3.00995596861619,-3.00669657453334,-3.00366740214253,
-2.99973127200117,-2.99314374523304,-2.94364090247096,-2.86670894548044,
-2.85055095601095,-2.84709090394187,-2.84514617557408,-2.84346726749296,
-2.84132600076709,-2.83790404593358,-2.81957711423026,-2.80891652745426,
-2.73669207491879,-2.70901751536791,-2.69213721490099,-2.68697328756015,
-2.68371187685395,-2.68068231677239,-2.67674778689009,-2.67016755184739,
-2.62108505627865,-2.54493668804139,-2.52769090989588,-2.52416333160112,
-2.52220351047619,-2.52052595489496,-2.51840471596455,-2.51424415045443,
-2.48734372264166,-2.41343298042621,-2.38593254279303,-2.36912835008891,
-2.36397282631354,-2.3607132905156,-2.35768310268818,-2.35374439357789,
-2.34714976139369,-2.29734863682004,-2.21959576937047,-2.20443222572976,
-2.20103751302584,-2.19910683116374,-2.19742569567641,-2.19526269934773,
-2.19075250656781,-2.14851804884808,-2.06719291631178,-2.04677288712501,
-2.0412558210861,-2.03791627694886,-2.03490847978163,-2.03106742517263,
-2.02317458368319,-1.95967605606827,-1.88628544679042,-1.87975250323861,
-1.877162868236,-1.87558422288974,-1.87385357929687,-1.87137531622725,-1.86506480397488,
-1.83306105454725,-1.77047461586855,-1.75729397090777,-1.7441860953638,
-1.72414060652952,-1.71841855108414,-1.71503336288645,-1.71233325925205,
-1.70870922850884,-1.70188403501992,-1.65762275671428,-1.60008308379339,
-1.56020166884823,-1.55571017087348,-1.55355071755667,-1.55186981265787,
-1.54993653655055,-1.54653042770158,-1.53120211913237,-1.45361840498715,
-1.40388867049861,-1.39729526300685,-1.39335671251092,-1.3903263291247,
-1.38706627187768,-1.38190926344052,-1.37008796384114),.UNSPECIFIED.);
#233=B_SPLINE_CURVE_WITH_KNOTS('',3,(#23211,#23212,#23213,#23214,#23215,
#23216,#23217,#23218,#23219,#23220,#23221,#23222,#23223,#23224,#23225,#23226,
#23227,#23228,#23229,#23230,#23231,#23232,#23233,#23234,#23235,#23236,#23237,
#23238,#23239,#23240,#23241,#23242,#23243,#23244,#23245,#23246,#23247,#23248,
#23249,#23250,#23251,#23252,#23253,#23254,#23255,#23256,#23257,#23258,#23259,
#23260,#23261,#23262,#23263,#23264,#23265,#23266,#23267,#23268,#23269,#23270,
#23271,#23272,#23273,#23274,#23275,#23276,#23277,#23278,#23279,#23280,#23281,
#23282,#23283,#23284,#23285,#23286,#23287,#23288,#23289,#23290,#23291,#23292,
#23293,#23294,#23295,#23296,#23297,#23298,#23299,#23300,#23301,#23302,#23303,
#23304,#23305,#23306,#23307,#23308,#23309,#23310,#23311,#23312,#23313,#23314,
#23315,#23316,#23317,#23318,#23319,#23320,#23321,#23322,#23323,#23324,#23325,
#23326,#23327,#23328,#23329,#23330,#23331,#23332,#23333,#23334,#23335,#23336,
#23337,#23338,#23339,#23340,#23341,#23342,#23343,#23344,#23345,#23346,#23347,
#23348,#23349,#23350,#23351,#23352,#23353,#23354,#23355,#23356,#23357,#23358,
#23359,#23360,#23361,#23362,#23363,#23364,#23365,#23366,#23367,#23368,#23369,
#23370,#23371,#23372,#23373,#23374,#23375,#23376,#23377,#23378,#23379,#23380,
#23381,#23382,#23383,#23384,#23385,#23386,#23387,#23388,#23389,#23390,#23391,
#23392,#23393,#23394,#23395,#23396,#23397,#23398,#23399,#23400,#23401,#23402,
#23403,#23404,#23405,#23406,#23407,#23408,#23409,#23410,#23411,#23412,#23413,
#23414,#23415,#23416,#23417,#23418,#23419,#23420),.UNSPECIFIED.,.F.,.F.,
(4,2,2,2,2,2,2,2,2,2,2,2,2,2,2,2,2,2,2,2,2,2,2,2,2,2,2,2,2,2,2,2,2,2,2,
2,2,2,2,2,2,2,2,2,2,2,2,2,2,2,2,2,2,2,2,2,2,2,2,2,2,2,2,2,2,2,2,2,2,2,2,
2,2,2,2,2,2,2,2,2,2,2,2,2,2,2,2,2,2,2,2,2,2,2,2,2,2,2,2,2,2,2,2,2,4),(-2.69288841829231,
-2.62821882857888,-2.6007272457602,-2.58392685535843,-2.57877203897195,
-2.5755128666472,-2.57248296531735,-2.5685445636208,-2.56195032742445,-2.5121627565062,
-2.43456185993032,-2.41921818360647,-2.41581133401556,-2.41387807961672,
-2.41219749054209,-2.41003887805007,-2.40555060755085,-2.36593727651975,
-2.30537801053633,-2.27772835275544,-2.26085845100696,-2.25569566369569,
-2.25243452943043,-2.24940492818091,-2.24546993238837,-2.23888804491525,
-2.18975083361885,-2.11365587102885,-2.09634556667394,-2.09281425284967,
-2.09085367158604,-2.08917621102593,-2.08705612618127,-2.08290112561271,
-2.05616258912101,-2.03199624470501,-1.94597896357116,-1.93591544299417,
-1.93199209624569,-1.92914836552149,-1.92610767860638,-1.92203409081843,
-1.91290505419737,-1.87535572106653,-1.80071489023966,-1.77429011247854,
-1.77014648718103,-1.76802884968564,-1.76635158185573,-1.76438920303215,
-1.76084957159198,-1.74339580996198,-1.66744737487523,-1.61838183785446,
-1.6118015624543,-1.60786697224214,-1.60483737445711,-1.60157594124946,
-1.5964120377444,-1.57953290048706,-1.55185828817305,-1.47924943754684,
-1.45124694014851,-1.44704848820846,-1.44491913173856,-1.44324097358994,
-1.44128718560547,-1.43778709672479,-1.42099750256704,-1.34456105711149,
-1.29525838411997,-1.28867332750679,-1.2847373215308,-1.28170747656142,
-1.27844660714296,-1.27328536447936,-1.25643075273483,-1.22881247853191,
-1.15561506517993,-1.12808709532021,-1.12390436286328,-1.12177835145588,
-1.1201004670003,-1.11814429827942,-1.1146331345721,-1.09765973572434,-1.02136300866315,
-0.97211996680353,-0.965536191401954,-0.961600609134019,-0.958570891342557,
-0.955309963443433,-0.950148213284202,-0.933288257111523,-0.905657539389735,
-0.832580728904072,-0.804956179165809,-0.800770253437381,-0.79864358802766,
-0.796965672120665,-0.795010015864425,-0.791501209614637,-0.774566977529387,
-0.698242856613169,-0.662479512201711),.UNSPECIFIED.);
#234=B_SPLINE_CURVE_WITH_KNOTS('',3,(#23426,#23427,#23428,#23429,#23430,
#23431,#23432,#23433,#23434,#23435,#23436,#23437,#23438,#23439,#23440,#23441,
#23442,#23443,#23444,#23445,#23446,#23447,#23448,#23449,#23450,#23451,#23452,
#23453,#23454,#23455,#23456,#23457,#23458,#23459,#23460,#23461,#23462,#23463,
#23464,#23465,#23466,#23467,#23468,#23469,#23470,#23471,#23472,#23473,#23474,
#23475,#23476,#23477,#23478,#23479,#23480,#23481,#23482,#23483,#23484,#23485,
#23486,#23487,#23488,#23489,#23490,#23491,#23492,#23493,#23494,#23495,#23496,
#23497,#23498,#23499,#23500,#23501,#23502,#23503,#23504,#23505,#23506,#23507,
#23508,#23509,#23510,#23511,#23512,#23513,#23514,#23515,#23516,#23517,#23518,
#23519,#23520,#23521,#23522,#23523,#23524,#23525,#23526,#23527,#23528,#23529,
#23530,#23531,#23532,#23533,#23534,#23535,#23536,#23537,#23538,#23539,#23540,
#23541,#23542,#23543,#23544,#23545,#23546,#23547,#23548,#23549,#23550,#23551,
#23552,#23553,#23554,#23555,#23556,#23557,#23558,#23559,#23560,#23561,#23562,
#23563,#23564,#23565,#23566,#23567),.UNSPECIFIED.,.F.,.F.,(4,3,3,3,3,3,
3,3,3,3,3,3,3,3,3,3,3,3,3,3,3,3,3,3,3,3,3,3,3,3,3,3,3,3,3,3,3,3,3,3,3,3,
3,3,3,3,3,4),(179.070781254915,179.194664687591,179.305500861943,179.39859273852,
179.491558370991,179.584425373595,179.677224205602,179.769987658213,179.862740536934,
179.955507631942,180.048373536086,180.141291001732,180.234363515655,180.305446874294,
180.398541048115,180.491509359221,180.584379412833,180.677181836596,180.769949210642,
180.862706333617,180.955477989103,181.048348910899,181.141271655451,181.234349817205,
181.305392886646,181.398334052106,181.491148767177,181.583864836116,181.676513311331,
181.76912680166,181.861730280687,181.954348707172,182.047067984862,182.139839721645,
182.232769500411,182.305338898997,182.398589636842,182.491713738259,182.584738616987,
182.677693796661,182.770612606954,182.863519673557,182.956439605844,183.04945531922,
183.142521141419,183.235738105157,183.305284911348,183.307775588641),
 .UNSPECIFIED.);
#235=B_SPLINE_CURVE_WITH_KNOTS('',3,(#23568,#23569,#23570,#23571,#23572,
#23573,#23574,#23575,#23576,#23577,#23578,#23579,#23580,#23581,#23582,#23583,
#23584,#23585,#23586,#23587,#23588,#23589,#23590,#23591,#23592,#23593,#23594,
#23595,#23596,#23597,#23598,#23599,#23600,#23601,#23602,#23603,#23604,#23605,
#23606,#23607,#23608,#23609,#23610,#23611,#23612,#23613,#23614,#23615,#23616,
#23617,#23618,#23619,#23620,#23621,#23622,#23623,#23624,#23625,#23626,#23627,
#23628,#23629,#23630,#23631,#23632,#23633,#23634,#23635,#23636,#23637,#23638,
#23639,#23640,#23641,#23642,#23643,#23644,#23645,#23646,#23647,#23648,#23649),
 .UNSPECIFIED.,.F.,.F.,(4,2,2,2,2,2,2,2,2,2,2,2,2,2,2,2,2,2,2,2,2,2,2,2,
2,2,2,2,2,2,2,2,2,2,2,2,2,2,2,2,4),(-4.06064997137112,-4.00430212489643,
-3.9868513581544,-3.9820030275949,-3.97866530730521,-3.97540299905737,-3.97237911174722,
-3.96846118072314,-3.96192906392512,-3.91487982033083,-3.89956282472104,
-3.89810813990657,-3.864651258576,-3.82517255520197,-3.81778930412554,-3.81575922412801,
-3.81383283440873,-3.81215259313831,-3.80998797932649,-3.80546786376064,
-3.75977925280789,-3.69886501358032,-3.67541231637473,-3.66050213306632,
-3.65574544601386,-3.65248155291347,-3.64945235973654,-3.64552208156608,
-3.63895720591681,-3.59061317511019,-3.51471753417946,-3.4966681963661,
-3.49309358890036,-3.49111519062416,-3.48943896207023,-3.48734102711929,
-3.48406109914624,-3.46794153634667,-3.45940315232818,-3.42919062260033,
-3.39966608106449),.UNSPECIFIED.);
#236=B_SPLINE_CURVE_WITH_KNOTS('',3,(#23651,#23652,#23653,#23654,#23655,
#23656,#23657,#23658,#23659,#23660,#23661,#23662,#23663,#23664,#23665,#23666,
#23667,#23668,#23669,#23670,#23671,#23672,#23673,#23674,#23675,#23676,#23677,
#23678,#23679,#23680,#23681,#23682,#23683,#23684,#23685,#23686,#23687,#23688,
#23689,#23690,#23691,#23692,#23693,#23694,#23695,#23696,#23697,#23698,#23699,
#23700,#23701,#23702,#23703,#23704,#23705,#23706,#23707,#23708,#23709,#23710,
#23711,#23712,#23713,#23714,#23715,#23716,#23717,#23718,#23719,#23720,#23721,
#23722,#23723,#23724,#23725,#23726,#23727,#23728,#23729,#23730,#23731,#23732,
#23733,#23734,#23735,#23736,#23737,#23738,#23739,#23740,#23741,#23742,#23743,
#23744,#23745,#23746,#23747,#23748,#23749,#23750,#23751,#23752,#23753,#23754,
#23755,#23756,#23757,#23758,#23759,#23760,#23761,#23762,#23763,#23764,#23765,
#23766),.UNSPECIFIED.,.F.,.F.,(4,2,2,2,2,2,2,2,2,2,2,2,2,2,2,2,2,2,2,2,
2,2,2,2,2,2,2,2,2,2,2,2,2,2,2,2,2,2,2,2,2,2,2,2,2,2,2,2,2,2,2,2,2,2,2,2,
2,4),(-0.662479512201711,-0.649009424411012,-0.642409141833841,-0.638468707869307,
-0.635438182478318,-0.632179264095796,-0.627026819422034,-0.610251866436487,
-0.582815677117585,-0.508156618053557,-0.481743925243419,-0.477600639337013,
-0.475483028236158,-0.473805651605458,-0.471842955267847,-0.468302491705472,
-0.450839150649112,-0.374882833553105,-0.325871973122078,-0.318694037867528,
-0.314917377826305,-0.311983489431598,-0.311920428982104,-0.31186191958805,
-0.311807486730928,-0.311756719226512,-0.311709262158357,-0.311664806402384,
-0.311623081297898,-0.311583848699337,-0.311546898111623,-0.311512042695099,
-0.311479115966062,-0.311447969026018,-0.311418468253126,-0.311390493337331,
-0.311363935643299,-0.311338696775966,-0.31131468739484,-0.31129182617357,
-0.311270038880336,-0.311234493337896,-0.307662220568363,-0.303815800756465,
-0.297749141659154,-0.26285874592463,-0.212549790608409,-0.18103199971563,
-0.158401309690868,-0.154766783500816,-0.152585227276661,-0.150897943913734,
-0.149001242898515,-0.145759233350475,-0.132638674924846,-0.107321035533903,
-0.0120020791574577,-0.00125822521736063),.UNSPECIFIED.);
#237=B_SPLINE_CURVE_WITH_KNOTS('',3,(#23767,#23768,#23769,#23770,#23771,
#23772,#23773,#23774,#23775,#23776,#23777,#23778,#23779,#23780,#23781,#23782,
#23783,#23784,#23785,#23786,#23787,#23788,#23789,#23790,#23791,#23792,#23793,
#23794,#23795,#23796,#23797,#23798,#23799,#23800,#23801,#23802,#23803,#23804,
#23805,#23806,#23807,#23808,#23809,#23810,#23811,#23812,#23813,#23814,#23815,
#23816,#23817,#23818,#23819,#23820,#23821,#23822,#23823,#23824,#23825,#23826,
#23827,#23828,#23829,#23830,#23831,#23832,#23833,#23834,#23835,#23836,#23837,
#23838,#23839,#23840,#23841,#23842,#23843,#23844,#23845,#23846,#23847,#23848,
#23849,#23850,#23851,#23852,#23853,#23854,#23855,#23856,#23857,#23858,#23859,
#23860,#23861,#23862,#23863,#23864,#23865,#23866,#23867,#23868,#23869,#23870,
#23871,#23872,#23873,#23874,#23875,#23876,#23877,#23878,#23879,#23880,#23881,
#23882,#23883,#23884,#23885,#23886,#23887,#23888,#23889,#23890,#23891,#23892,
#23893,#23894,#23895,#23896,#23897,#23898,#23899,#23900,#23901,#23902,#23903,
#23904,#23905,#23906,#23907,#23908,#23909,#23910,#23911,#23912,#23913,#23914,
#23915,#23916,#23917,#23918),.UNSPECIFIED.,.F.,.F.,(4,2,2,2,2,2,2,2,2,2,
2,2,2,2,2,2,2,2,2,2,2,2,2,2,2,2,2,2,2,2,2,2,2,2,2,2,2,2,2,2,2,2,2,2,2,2,
2,2,2,2,2,2,2,2,2,2,2,2,2,2,2,2,2,2,2,2,2,2,2,2,2,2,2,2,2,4),(1.36975430456593,
1.42172213103555,1.42835907822274,1.43231026028757,1.43534261990349,1.43859721798056,
1.44372951406029,1.46032157515104,1.48733375467083,1.56345959992786,1.58911797235801,
1.59323077093026,1.59534102870295,1.5970163230271,1.59898047451482,1.60253580486721,
1.62032079655486,1.69595908431547,1.74497514520024,1.75154764787522,1.75547693459096,
1.75850205496357,1.76175826077702,1.7669129693815,1.78375284916472,1.81134514278918,
1.88470936858748,1.91205219408331,1.91622378369688,1.9183453985704,1.92002128184319,
1.9219772152077,1.92548956202872,1.9424990451031,2.01876868011758,2.06797842187324,
2.07457334368562,2.07851187574343,2.08154172293333,2.0848006946761,2.08995491720612,
2.10675154389236,2.13423850540126,2.2080107693298,2.234962355599,2.23912474317568,
2.24124647941251,2.24292384677168,2.24488255613175,2.24840757550826,2.26562940368616,
2.3417535912804,2.39083775208834,2.39800956423947,2.40178339871772,2.40470300808647,
2.40798193156949,2.41142081405101,2.41651204772883,2.47970159142052,2.55460999112475,
2.56099596046146,2.56355977958516,2.56513277122848,2.56686638517147,2.56936480342705,
2.57581282132122,2.60920785722189,2.70538587515279,2.71843531316576,2.72327801529024,
2.72614870782649,2.72903657179424,2.73196675294122,2.73523955564581,2.73829514625514),
 .UNSPECIFIED.);
#238=B_SPLINE_CURVE_WITH_KNOTS('',3,(#23922,#23923,#23924,#23925,#23926,
#23927,#23928,#23929,#23930,#23931,#23932,#23933,#23934,#23935,#23936,#23937,
#23938,#23939,#23940,#23941,#23942,#23943,#23944,#23945,#23946,#23947,#23948,
#23949,#23950,#23951,#23952,#23953,#23954,#23955,#23956,#23957,#23958,#23959,
#23960,#23961,#23962,#23963,#23964,#23965,#23966,#23967,#23968,#23969,#23970,
#23971,#23972,#23973,#23974,#23975,#23976,#23977,#23978,#23979,#23980,#23981,
#23982,#23983,#23984,#23985,#23986,#23987,#23988,#23989,#23990,#23991,#23992,
#23993,#23994),.UNSPECIFIED.,.F.,.F.,(4,3,3,3,3,3,3,3,3,3,3,3,3,3,3,3,3,
3,3,3,3,3,3,3,4),(-4.09274904019422,-3.99978404940549,-3.91106269308813,
-3.8224565701686,-3.73394206808229,-3.64217906420377,-3.55376958798201,
-3.46537482046749,-3.37697356575947,-3.28854462858425,-3.20001846627961,
-3.11143447070011,-3.02272368784104,-2.99983803705412,-2.91202313233303,
-2.82432062379338,-2.73670592850525,-2.64915228090865,-2.56163015593267,
-2.47411747838494,-2.38659218514979,-2.29898035505946,-2.21132256779175,
-2.12353003259716,-2.06151489981891),.UNSPECIFIED.);
#239=B_SPLINE_CURVE_WITH_KNOTS('',3,(#23998,#23999,#24000,#24001,#24002),
 .UNSPECIFIED.,.F.,.F.,(4,1,4),(0.,0.99994601235136,1.11004521091143),
 .UNSPECIFIED.);
#240=B_SPLINE_CURVE_WITH_KNOTS('',3,(#24004,#24005,#24006,#24007,#24008,
#24009,#24010,#24011,#24012,#24013,#24014,#24015,#24016,#24017,#24018,#24019,
#24020,#24021,#24022,#24023,#24024,#24025,#24026,#24027,#24028,#24029,#24030,
#24031,#24032,#24033,#24034,#24035,#24036,#24037,#24038,#24039,#24040,#24041,
#24042,#24043,#24044,#24045,#24046,#24047,#24048,#24049,#24050,#24051,#24052,
#24053,#24054,#24055,#24056,#24057,#24058,#24059,#24060,#24061,#24062,#24063,
#24064,#24065,#24066,#24067,#24068,#24069,#24070,#24071,#24072,#24073,#24074,
#24075,#24076,#24077,#24078,#24079,#24080,#24081,#24082,#24083,#24084,#24085,
#24086,#24087,#24088,#24089,#24090,#24091,#24092,#24093,#24094,#24095,#24096,
#24097,#24098,#24099,#24100,#24101,#24102,#24103,#24104,#24105,#24106,#24107,
#24108,#24109,#24110,#24111,#24112,#24113,#24114,#24115,#24116,#24117,#24118,
#24119,#24120,#24121,#24122,#24123,#24124,#24125,#24126,#24127,#24128,#24129,
#24130,#24131,#24132,#24133,#24134,#24135,#24136,#24137,#24138,#24139,#24140,
#24141,#24142,#24143,#24144,#24145,#24146,#24147,#24148,#24149,#24150,#24151,
#24152,#24153,#24154,#24155,#24156,#24157,#24158,#24159,#24160,#24161,#24162,
#24163,#24164,#24165,#24166,#24167,#24168,#24169,#24170,#24171,#24172,#24173,
#24174,#24175,#24176,#24177,#24178,#24179,#24180,#24181,#24182,#24183,#24184,
#24185,#24186,#24187,#24188,#24189,#24190,#24191,#24192,#24193,#24194,#24195,
#24196,#24197,#24198,#24199,#24200,#24201,#24202,#24203,#24204,#24205,#24206,
#24207,#24208,#24209,#24210,#24211,#24212,#24213,#24214,#24215,#24216,#24217,
#24218,#24219,#24220,#24221,#24222,#24223,#24224,#24225,#24226,#24227,#24228,
#24229),.UNSPECIFIED.,.F.,.F.,(4,3,3,3,3,3,3,3,3,3,3,3,3,3,3,3,3,3,3,3,
3,3,3,3,3,3,3,3,3,3,3,3,3,3,3,3,3,3,3,3,3,3,3,3,3,3,3,3,3,3,3,3,3,3,3,3,
3,3,3,3,3,3,3,3,3,3,3,3,3,3,3,3,3,3,3,4),(1.11004521091143,1.19654798308244,
1.28294343992058,1.37256201301835,1.45882332647987,1.54506113767005,1.63129831945091,
1.71755774326959,1.80391109059945,1.89032034860343,1.97685772330168,1.99989202470273,
2.08856526631284,2.17712371506071,2.26559102252296,2.35737189933935,2.44573560240637,
2.53408518581266,2.62244188184438,2.71082692264793,2.79931035885651,2.88785225711593,
2.97652216123164,2.99983803705411,3.08854237714131,3.17713472538585,3.26563868098512,
3.35740685203767,3.44581388317613,3.53420920066809,3.62261399977723,3.7110494773624,
3.79958658197351,3.88818409875563,3.97691207014386,3.99978404940548,4.08821701236545,
4.1765337235679,4.26475813713124,4.35662962770944,4.4447491111496,4.53285440935254,
4.62096701909789,4.70910843742362,4.79735018389678,4.88565122025918,4.97408335872012,
4.99973006175686,5.08830339777262,5.17676200893295,5.26512967357959,5.35694797364567,
5.44521319848833,5.53346491396212,5.62172446584756,5.710013200411,5.79840208000763,
5.88685032811372,5.97542865050467,5.99967607410823,6.08824398278253,6.17669743939677,
6.26506022746791,6.35688045984187,6.44514154014848,6.53338938989229,6.62164536044511,
6.70993080388133,6.79831684303157,6.88676250976978,6.97533865408563,6.9996220864596,
7.09845393160949,7.19699737151629,7.29511382857198,7.39323028562766),
 .UNSPECIFIED.);
#241=B_SPLINE_CURVE_WITH_KNOTS('',3,(#24231,#24232,#24233,#24234,#24235,
#24236,#24237,#24238,#24239,#24240),.UNSPECIFIED.,.F.,.F.,(4,1,1,1,1,1,
1,4),(7.39323051809102,7.99956809881098,8.99951411116236,9.99946012351374,
10.9994061358651,11.9993521482165,12.9992981605679,13.6764158252706),
 .UNSPECIFIED.);
#242=B_SPLINE_CURVE_WITH_KNOTS('',3,(#24242,#24243,#24244,#24245,#24246,
#24247,#24248,#24249,#24250,#24251,#24252,#24253,#24254,#24255,#24256,#24257,
#24258,#24259,#24260,#24261,#24262,#24263,#24264,#24265,#24266,#24267,#24268,
#24269,#24270,#24271,#24272,#24273,#24274,#24275,#24276,#24277,#24278,#24279,
#24280,#24281,#24282,#24283,#24284,#24285,#24286,#24287,#24288,#24289,#24290,
#24291,#24292,#24293,#24294,#24295,#24296,#24297,#24298,#24299,#24300,#24301,
#24302,#24303,#24304,#24305,#24306,#24307,#24308,#24309,#24310,#24311,#24312,
#24313,#24314,#24315,#24316,#24317,#24318,#24319,#24320,#24321,#24322,#24323,
#24324,#24325,#24326,#24327,#24328,#24329,#24330,#24331,#24332,#24333,#24334,
#24335,#24336,#24337,#24338,#24339,#24340,#24341,#24342,#24343,#24344,#24345,
#24346,#24347,#24348,#24349,#24350,#24351,#24352,#24353,#24354,#24355,#24356,
#24357,#24358,#24359,#24360,#24361,#24362,#24363,#24364,#24365,#24366,#24367,
#24368,#24369,#24370,#24371,#24372,#24373,#24374,#24375,#24376,#24377,#24378,
#24379,#24380,#24381,#24382,#24383,#24384,#24385,#24386,#24387,#24388,#24389,
#24390,#24391,#24392,#24393,#24394,#24395,#24396,#24397,#24398,#24399,#24400,
#24401,#24402,#24403,#24404,#24405,#24406,#24407,#24408,#24409,#24410,#24411,
#24412,#24413,#24414,#24415,#24416,#24417,#24418,#24419,#24420,#24421,#24422,
#24423,#24424,#24425,#24426,#24427,#24428,#24429,#24430,#24431,#24432,#24433,
#24434,#24435,#24436,#24437,#24438,#24439,#24440,#24441,#24442,#24443,#24444,
#24445,#24446,#24447,#24448,#24449,#24450,#24451,#24452,#24453,#24454,#24455,
#24456,#24457,#24458,#24459,#24460,#24461,#24462,#24463,#24464),
 .UNSPECIFIED.,.F.,.F.,(4,3,3,3,3,3,3,3,3,3,3,3,3,3,3,3,3,3,3,3,3,3,3,3,
3,3,3,3,3,3,3,3,3,3,3,3,3,3,3,3,3,3,3,3,3,3,3,3,3,3,3,3,3,3,3,3,3,3,3,3,
3,3,3,3,3,3,3,3,3,3,3,3,3,3,4),(13.6764160462236,13.7802779401167,13.8897610565179,
13.9992441729192,14.0877938450277,14.1762287121119,14.2645725817854,14.3563997822211,
14.4446412388262,14.5328692371514,14.6211051488017,14.7093703459499,14.7977359613827,
14.886161075732,14.9747166370169,14.9991901852706,15.0877397450242,15.1761744991284,
15.2645182553368,15.3563454981224,15.4445868407756,15.5328147251651,15.6210505230179,
15.7093156066296,15.7976811094917,15.8861061116931,15.9746615623273,15.999136197622,
16.0876856965531,16.1761203885788,16.264464081533,16.356291347588,16.4445326244357,
16.5327604421866,16.6209961726353,16.7092611881441,16.7976266222034,16.8860515551089,
16.974606936256,16.9990822099733,17.0876317737306,17.1760665314604,17.264410290913,
17.3562375323395,17.4444788772557,17.5327067635402,17.6209425629163,17.7092076476754,
17.7975731511168,17.8859981535672,17.9745536039599,17.9990282223247,18.0875777660888,
18.1760125036722,18.2643562428505,18.3561834918287,18.4444248162795,18.5326526820631,
18.6208884609244,18.7091535251768,18.7975190082276,18.8859439903297,18.9744994205947,
18.9989742346761,19.0869698722266,19.1748511299411,19.2626424314125,19.3503698897695,
19.4380636509169,19.5257456458262,19.6134377916244,19.7012172493001,19.7890401091154,
19.8770064336621,19.9596011323108),.UNSPECIFIED.);
#243=B_SPLINE_CURVE_WITH_KNOTS('',3,(#24466,#24467,#24468,#24469,#24470,
#24471,#24472,#24473,#24474,#24475,#24476,#24477,#24478,#24479,#24480,#24481,
#24482,#24483,#24484,#24485,#24486,#24487,#24488,#24489,#24490,#24491,#24492,
#24493,#24494,#24495,#24496,#24497,#24498,#24499,#24500,#24501,#24502,#24503,
#24504,#24505,#24506,#24507,#24508,#24509,#24510,#24511,#24512,#24513,#24514,
#24515,#24516,#24517,#24518,#24519,#24520,#24521,#24522,#24523,#24524,#24525,
#24526,#24527,#24528,#24529,#24530,#24531,#24532,#24533,#24534,#24535,#24536,
#24537,#24538,#24539,#24540,#24541,#24542,#24543,#24544,#24545,#24546,#24547,
#24548,#24549,#24550,#24551,#24552,#24553,#24554,#24555,#24556,#24557,#24558,
#24559,#24560,#24561,#24562,#24563,#24564,#24565,#24566,#24567,#24568,#24569,
#24570,#24571,#24572,#24573,#24574,#24575,#24576,#24577,#24578,#24579,#24580,
#24581,#24582,#24583,#24584,#24585,#24586,#24587,#24588,#24589,#24590,#24591,
#24592,#24593,#24594,#24595,#24596,#24597,#24598,#24599,#24600,#24601,#24602,
#24603,#24604,#24605,#24606,#24607,#24608,#24609,#24610,#24611,#24612,#24613,
#24614,#24615,#24616,#24617,#24618,#24619,#24620,#24621,#24622,#24623,#24624,
#24625,#24626,#24627,#24628,#24629,#24630,#24631,#24632,#24633,#24634,#24635,
#24636,#24637,#24638,#24639,#24640,#24641,#24642,#24643,#24644,#24645,#24646,
#24647,#24648,#24649,#24650,#24651,#24652,#24653,#24654,#24655,#24656,#24657,
#24658,#24659,#24660,#24661,#24662,#24663,#24664,#24665,#24666,#24667,#24668,
#24669,#24670,#24671,#24672,#24673,#24674,#24675,#24676,#24677,#24678,#24679,
#24680,#24681,#24682,#24683,#24684,#24685,#24686,#24687,#24688,#24689,#24690,
#24691,#24692,#24693,#24694),.UNSPECIFIED.,.F.,.F.,(4,3,3,3,3,3,3,3,3,3,
3,3,3,3,3,3,3,3,3,3,3,3,3,3,3,3,3,3,3,3,3,3,3,3,3,3,3,3,3,3,3,3,3,3,3,3,
3,3,3,3,3,3,3,3,3,3,3,3,3,3,3,3,3,3,3,3,3,3,3,3,3,3,3,3,3,3,4),(19.9596011324502,
19.9989202470274,20.0874697934524,20.1759045336718,20.2642482754581,20.3560755234482,
20.4443168504197,20.532544718687,20.6207804999927,20.7090455666468,20.7974110520236,
20.8858360364104,20.9743914688815,20.9988662593788,21.0874158024492,21.1758505392836,
21.2641942776585,21.3560215269175,21.4442628504338,21.5324907152358,21.6207264930694,
21.7089915562485,21.7973570381634,21.8857820190918,21.9743374481363,21.9988122717302,
22.0873618142379,22.175796550492,22.26414028827,22.3559675377465,22.4442088606275,
22.532436724781,22.6206725019536,22.7089375644599,22.7973030456876,22.8857280259196,
22.9742834542594,22.9987582840816,23.0873078278185,23.17574256532,23.2640863043619,
23.3559135533708,23.4441548775493,23.5323827430104,23.6206185214995,23.7088835853299,
23.7972490678861,23.8856740494509,23.9742294791195,23.9987042964329,24.0872538396301,
24.1756885765864,24.2640323150784,24.3558595642917,24.4441008879117,24.5323287528123,
24.6205645307393,24.7088295940064,24.7971950760008,24.8856200570039,24.9741754861153,
24.9986503087843,25.0871998519514,25.1756345888759,25.263978327334,25.3558055765592,
25.4440469001412,25.5322747650021,25.6205105428879,25.7087756061121,25.7971410880619,
25.8855660690191,25.9741214980832,25.9985963211357,26.1206913455188,26.2351355066195,
26.2427863699019),.UNSPECIFIED.);
#244=B_SPLINE_CURVE_WITH_KNOTS('',3,(#24696,#24697,#24698,#24699,#24700,
#24701,#24702,#24703,#24704,#24705),.UNSPECIFIED.,.F.,.F.,(4,1,1,1,1,1,
1,4),(26.2427864396298,26.998542333487,27.9984883458384,28.9984343581898,
29.9983803705412,30.9983263828926,31.9982723952439,32.5259717468094),
 .UNSPECIFIED.);
#245=B_SPLINE_CURVE_WITH_KNOTS('',3,(#24707,#24708,#24709,#24710,#24711,
#24712,#24713,#24714,#24715,#24716),.UNSPECIFIED.,.F.,.F.,(4,1,1,1,1,1,
1,4),(32.5259717468094,32.9982184075953,33.9981644199467,34.998110432298,
35.9980564446494,36.9980024570008,37.9979484693521,38.8091526513998),
 .UNSPECIFIED.);
#246=B_SPLINE_CURVE_WITH_KNOTS('',3,(#24718,#24719,#24720,#24721,#24722,
#24723,#24724,#24725,#24726,#24727,#24728,#24729,#24730,#24731,#24732,#24733,
#24734,#24735,#24736,#24737,#24738,#24739,#24740,#24741,#24742,#24743,#24744,
#24745,#24746,#24747,#24748,#24749,#24750,#24751,#24752,#24753,#24754,#24755,
#24756,#24757,#24758,#24759,#24760,#24761,#24762,#24763,#24764,#24765,#24766,
#24767,#24768,#24769,#24770,#24771,#24772,#24773,#24774,#24775,#24776,#24777,
#24778,#24779,#24780,#24781,#24782,#24783,#24784,#24785,#24786,#24787,#24788,
#24789,#24790,#24791,#24792,#24793,#24794,#24795,#24796,#24797,#24798,#24799,
#24800,#24801,#24802,#24803,#24804,#24805,#24806,#24807,#24808,#24809,#24810,
#24811,#24812,#24813,#24814,#24815,#24816,#24817,#24818,#24819,#24820,#24821,
#24822,#24823,#24824,#24825,#24826,#24827,#24828,#24829,#24830,#24831,#24832,
#24833,#24834,#24835,#24836,#24837,#24838,#24839,#24840,#24841,#24842,#24843,
#24844,#24845,#24846,#24847,#24848,#24849,#24850,#24851,#24852,#24853,#24854,
#24855,#24856,#24857,#24858,#24859,#24860,#24861,#24862,#24863,#24864,#24865,
#24866,#24867,#24868,#24869,#24870,#24871,#24872,#24873,#24874,#24875,#24876,
#24877,#24878,#24879,#24880,#24881,#24882,#24883,#24884,#24885,#24886,#24887,
#24888,#24889,#24890,#24891,#24892,#24893,#24894,#24895,#24896,#24897,#24898,
#24899,#24900,#24901,#24902,#24903,#24904,#24905,#24906,#24907,#24908,#24909,
#24910,#24911,#24912,#24913,#24914,#24915,#24916,#24917,#24918,#24919,#24920,
#24921,#24922,#24923,#24924,#24925,#24926,#24927,#24928,#24929,#24930,#24931,
#24932,#24933,#24934,#24935,#24936,#24937,#24938,#24939,#24940,#24941,#24942,
#24943),.UNSPECIFIED.,.F.,.F.,(4,3,3,3,3,3,3,3,3,3,3,3,3,3,3,3,3,3,3,3,
3,3,3,3,3,3,3,3,3,3,3,3,3,3,3,3,3,3,3,3,3,3,3,3,3,3,3,3,3,3,3,3,3,3,3,3,
3,3,3,3,3,3,3,3,3,3,3,3,3,3,3,3,3,3,3,4),(38.809157053989,38.9402318305317,
38.9978944817035,39.0864440249643,39.174878761984,39.2632225005392,39.3550497497287,
39.4432910734108,39.5315189383729,39.6197547163609,39.7080197796883,39.7963852617418,
39.8848102428031,39.9733656719714,39.9978404940549,40.0863900373156,40.1748247743353,
40.2631685128904,40.3549957620799,40.4432370857619,40.5314649507239,40.6197007287117,
40.7079657920391,40.7963312740924,40.8847562551537,40.9733116843219,40.9977865064063,
41.086336049667,41.1747707866867,41.2631145252418,41.3549417744313,41.4431830981132,
41.5314109630753,41.619646741063,41.7079118043903,41.7962772864437,41.8847022675049,
41.9732576966731,41.9977325187576,42.0862820620183,42.174716799038,42.2630605375931,
42.3548877867826,42.4431291104647,42.5313569754267,42.6195927534145,42.7078578167418,
42.7962232987952,42.8846482798565,42.9732037090247,42.997678531109,43.0862280743697,
43.1746628113895,43.2630065499446,43.3548337991341,43.4430751228161,43.5313029877781,
43.619538765766,43.7078038290934,43.7961693111468,43.8845942922081,43.9731497213763,
43.9976245434604,44.0861740867211,44.1746088237409,44.2629525622959,44.3547798114854,
44.4430211351675,44.5312490001295,44.6194847781173,44.7077498414445,44.7961153234978,
44.8845403045592,44.9730957337274,44.9975705558118,45.0923423611685),
 .UNSPECIFIED.);
#247=B_SPLINE_CURVE_WITH_KNOTS('',3,(#24945,#24946,#24947,#24948,#24949,
#24950,#24951,#24952,#24953,#24954),.UNSPECIFIED.,.F.,.F.,(4,1,1,1,1,1,
1,4),(45.0923512995181,45.9975165681631,46.9974625805145,47.9974085928659,
48.9973546052172,49.9973006175686,50.99724662992,51.3755200907042),
 .UNSPECIFIED.);
#248=B_SPLINE_CURVE_WITH_KNOTS('',3,(#24956,#24957,#24958,#24959,#24960,
#24961,#24962,#24963,#24964,#24965,#24966,#24967,#24968,#24969,#24970,#24971,
#24972,#24973,#24974,#24975,#24976,#24977,#24978,#24979,#24980,#24981,#24982,
#24983,#24984,#24985,#24986,#24987,#24988,#24989,#24990,#24991,#24992,#24993,
#24994,#24995,#24996,#24997,#24998,#24999,#25000,#25001,#25002,#25003,#25004,
#25005,#25006,#25007,#25008,#25009,#25010,#25011,#25012,#25013,#25014,#25015,
#25016,#25017,#25018,#25019,#25020,#25021,#25022,#25023,#25024,#25025,#25026,
#25027,#25028,#25029,#25030,#25031,#25032,#25033,#25034,#25035,#25036,#25037,
#25038,#25039,#25040,#25041,#25042,#25043,#25044,#25045,#25046,#25047,#25048,
#25049,#25050,#25051,#25052,#25053,#25054,#25055,#25056,#25057,#25058,#25059,
#25060,#25061,#25062,#25063,#25064,#25065,#25066,#25067,#25068,#25069,#25070,
#25071,#25072,#25073,#25074,#25075,#25076,#25077,#25078,#25079,#25080,#25081,
#25082,#25083,#25084,#25085,#25086,#25087,#25088,#25089,#25090,#25091,#25092,
#25093,#25094,#25095,#25096,#25097,#25098,#25099,#25100,#25101,#25102,#25103,
#25104,#25105,#25106,#25107,#25108,#25109,#25110,#25111,#25112,#25113,#25114,
#25115,#25116,#25117,#25118,#25119,#25120,#25121,#25122,#25123,#25124,#25125,
#25126,#25127,#25128,#25129,#25130,#25131,#25132,#25133,#25134,#25135,#25136,
#25137,#25138,#25139,#25140,#25141,#25142,#25143,#25144,#25145,#25146,#25147,
#25148,#25149,#25150,#25151,#25152,#25153,#25154,#25155,#25156,#25157,#25158,
#25159,#25160,#25161,#25162,#25163,#25164,#25165,#25166,#25167,#25168,#25169,
#25170,#25171,#25172,#25173,#25174,#25175,#25176,#25177,#25178,#25179,#25180,
#25181),.UNSPECIFIED.,.F.,.F.,(4,3,3,3,3,3,3,3,3,3,3,3,3,3,3,3,3,3,3,3,
3,3,3,3,3,3,3,3,3,3,3,3,3,3,3,3,3,3,3,3,3,3,3,3,3,3,3,3,3,3,3,3,3,3,3,3,
3,3,3,3,3,3,3,3,3,3,3,3,3,3,3,3,3,3,3,4),(51.3755276683481,51.4644854095652,
51.5534539425206,51.642453477088,51.731568782179,51.8207424676004,51.9100816636312,
51.9971926422714,52.0857421855321,52.1741769225517,52.2625206611069,52.3543479102964,
52.4425892339784,52.5308170989404,52.6190528769282,52.7073179402553,52.7956834223086,
52.8841084033699,52.972663832538,52.9971386546227,53.0856881978835,53.1741229349033,
53.2624666734584,53.3542939226479,53.4425352463299,53.530763111292,53.6189988892798,
53.7072639526072,53.7956294346605,53.8840544157218,53.9726098448899,53.9970846669741,
54.0856342102349,54.1740689472545,54.2624126858097,54.3542399349992,54.4424812586813,
54.5307091236433,54.618944901631,54.7072099649584,54.7955754470118,54.8840004280729,
54.9725558572412,54.9970306793255,55.0855802225862,55.1740149596059,55.2623586981611,
55.3541859473506,55.4424272710327,55.5306551359947,55.6188909139824,55.7071559773094,
55.7955214593627,55.8839464404242,55.9725018695924,55.9969766916768,56.0855262349375,
56.1739609719573,56.2623047105123,56.3541319597018,56.442373283384,56.5306011483461,
56.6188369263337,56.7071019896608,56.7954674717142,56.8838924527754,56.9724478819438,
56.9969227040282,57.0854947724333,57.1739540959007,57.26232214872,57.3506203291089,
57.4388747032672,57.5271032295614,57.6153453697455,57.6587129755277),
 .UNSPECIFIED.);
#249=B_SPLINE_CURVE_WITH_KNOTS('',3,(#25183,#25184,#25185,#25186,#25187,
#25188,#25189,#25190,#25191,#25192,#25193,#25194,#25195,#25196,#25197,#25198,
#25199,#25200,#25201,#25202,#25203,#25204,#25205,#25206,#25207,#25208,#25209,
#25210,#25211,#25212,#25213,#25214,#25215,#25216,#25217,#25218,#25219,#25220,
#25221,#25222,#25223,#25224,#25225,#25226,#25227,#25228,#25229,#25230,#25231,
#25232,#25233,#25234,#25235,#25236,#25237,#25238,#25239,#25240,#25241,#25242,
#25243,#25244,#25245,#25246,#25247,#25248,#25249,#25250,#25251,#25252,#25253,
#25254,#25255,#25256,#25257,#25258,#25259,#25260,#25261,#25262,#25263,#25264,
#25265,#25266,#25267,#25268,#25269,#25270,#25271,#25272,#25273,#25274,#25275,
#25276,#25277,#25278,#25279,#25280,#25281,#25282,#25283,#25284,#25285,#25286,
#25287,#25288,#25289,#25290,#25291,#25292,#25293,#25294,#25295,#25296,#25297,
#25298,#25299,#25300,#25301,#25302,#25303,#25304,#25305,#25306,#25307,#25308,
#25309,#25310,#25311,#25312,#25313,#25314,#25315,#25316,#25317,#25318,#25319,
#25320,#25321,#25322,#25323,#25324,#25325,#25326,#25327,#25328,#25329,#25330,
#25331,#25332,#25333,#25334,#25335,#25336,#25337,#25338,#25339,#25340,#25341,
#25342,#25343,#25344,#25345,#25346,#25347,#25348,#25349,#25350,#25351,#25352,
#25353,#25354,#25355,#25356,#25357,#25358,#25359,#25360,#25361,#25362,#25363,
#25364,#25365,#25366,#25367,#25368,#25369,#25370,#25371,#25372,#25373,#25374,
#25375,#25376,#25377,#25378,#25379,#25380,#25381,#25382,#25383,#25384,#25385,
#25386,#25387,#25388,#25389,#25390,#25391,#25392,#25393,#25394,#25395,#25396,
#25397,#25398,#25399,#25400,#25401,#25402,#25403,#25404,#25405,#25406,#25407,
#25408),.UNSPECIFIED.,.F.,.F.,(4,3,3,3,3,3,3,3,3,3,3,3,3,3,3,3,3,3,3,3,
3,3,3,3,3,3,3,3,3,3,3,3,3,3,3,3,3,3,3,3,3,3,3,3,3,3,3,3,3,3,3,3,3,3,3,3,
3,3,3,3,3,3,3,3,3,3,3,3,3,3,3,3,3,3,3,4),(57.6587129757527,57.7611008096764,
57.8640988984394,57.9677937989378,57.9968687163796,58.0854182596404,58.17385299666,
58.2621967352151,58.3540239844046,58.4422653080866,58.5304931730487,58.6187289510364,
58.7069940143638,58.7953594964171,58.8837844774784,58.9723399066465,58.996814728731,
59.0853642719917,59.1737990090114,59.2621427475665,59.3539699967559,59.442211320438,
59.5304391854,59.6186749633878,59.7069400267152,59.7953055087685,59.8837304898298,
59.972285918998,59.9967607410823,60.085310284343,60.1737450213627,60.2620887599178,
60.3539160091073,60.4421573327893,60.5303851977514,60.6186209757392,60.7068860390665,
60.7952515211198,60.8836765021811,60.9722319313493,60.9967067534337,61.0852562966945,
61.1736910337142,61.2620347722692,61.3538620214587,61.4421033451408,61.5303312101028,
61.6185669880906,61.706832051418,61.7951975334714,61.8836225145326,61.9721779437008,
61.9966527657851,62.0852023090459,62.1736370460656,62.2619807846206,62.3538080338101,
62.4420493574922,62.5302772224542,62.618513000442,62.7067780637692,62.7951435458225,
62.8835685268838,62.972123956052,62.9965987781365,63.0844206635694,63.1721283405569,
63.2597464032859,63.3473010237067,63.4348225101216,63.5223329419007,63.6098543850565,
63.6974616170165,63.7851133634083,63.8729020343142,63.9418982827073),
 .UNSPECIFIED.);
#250=B_SPLINE_CURVE_WITH_KNOTS('',3,(#25410,#25411,#25412,#25413,#25414,
#25415,#25416,#25417,#25418,#25419,#25420),.UNSPECIFIED.,.F.,.F.,(4,1,1,
1,1,1,1,1,4),(63.9418982827073,63.9965447904879,64.9964908028392,65.9964368151906,
66.996382827542,67.9963288398934,68.9962748522447,69.9962208645961,70.2250835898869),
 .UNSPECIFIED.);
#251=B_SPLINE_CURVE_WITH_KNOTS('',3,(#25422,#25423,#25424,#25425,#25426,
#25427,#25428,#25429,#25430,#25431,#25432,#25433,#25434,#25435,#25436,#25437,
#25438,#25439,#25440,#25441,#25442,#25443,#25444,#25445,#25446,#25447,#25448,
#25449,#25450,#25451,#25452,#25453,#25454,#25455,#25456,#25457,#25458,#25459,
#25460,#25461,#25462,#25463,#25464,#25465,#25466,#25467,#25468,#25469,#25470,
#25471,#25472,#25473,#25474,#25475,#25476,#25477,#25478,#25479,#25480,#25481,
#25482,#25483,#25484,#25485,#25486,#25487,#25488,#25489,#25490,#25491,#25492,
#25493,#25494,#25495,#25496,#25497,#25498,#25499,#25500,#25501,#25502,#25503,
#25504,#25505,#25506,#25507,#25508,#25509,#25510,#25511,#25512,#25513,#25514,
#25515,#25516,#25517,#25518,#25519,#25520,#25521,#25522,#25523,#25524,#25525,
#25526,#25527,#25528,#25529,#25530,#25531,#25532,#25533,#25534,#25535,#25536,
#25537,#25538,#25539,#25540,#25541,#25542,#25543,#25544,#25545,#25546,#25547,
#25548,#25549,#25550,#25551,#25552,#25553,#25554,#25555,#25556,#25557,#25558,
#25559,#25560,#25561,#25562,#25563,#25564,#25565,#25566,#25567,#25568,#25569,
#25570,#25571,#25572,#25573,#25574,#25575,#25576,#25577,#25578,#25579,#25580,
#25581,#25582,#25583,#25584,#25585,#25586,#25587,#25588,#25589,#25590,#25591,
#25592,#25593,#25594,#25595,#25596,#25597,#25598,#25599,#25600,#25601,#25602,
#25603,#25604,#25605,#25606,#25607,#25608,#25609,#25610,#25611,#25612,#25613,
#25614,#25615,#25616,#25617,#25618,#25619,#25620,#25621,#25622,#25623,#25624,
#25625,#25626,#25627,#25628,#25629,#25630,#25631,#25632,#25633,#25634,#25635,
#25636,#25637,#25638,#25639,#25640,#25641,#25642,#25643,#25644,#25645,#25646,
#25647),.UNSPECIFIED.,.F.,.F.,(4,3,3,3,3,3,3,3,3,3,3,3,3,3,3,3,3,3,3,3,
3,3,3,3,3,3,3,3,3,3,3,3,3,3,3,3,3,3,3,3,3,3,3,3,3,3,3,3,3,3,3,3,3,3,3,3,
3,3,3,3,3,3,3,3,3,3,3,3,3,3,3,3,3,3,3,4),(70.2250835898869,70.31227753055,
70.3994065089422,70.4865013955672,70.5735846005634,70.6606785201825,70.7478600908778,
70.8350863988569,70.9224543524563,70.9961668769474,71.0847164202081,71.1731511572278,
71.2614948957828,71.3533221449723,71.4415634686544,71.5297913336164,71.6180271116043,
71.7062921749316,71.794657656985,71.8830826380461,71.9716380672144,71.9961128892988,
72.0846624325596,72.1730971695793,72.2614409081343,72.3532681573238,72.441509481006,
72.529737345968,72.6179731239558,72.7062381872829,72.7946036693362,72.8830286503972,
72.9715840795655,72.9960589016502,73.0846084449109,73.1730431819306,73.2613869204854,
73.3532141696749,73.4414554933569,73.5296833583189,73.6179191363067,73.7061841996341,
73.7945496816876,73.8829746627492,73.9715300919174,73.9960049140016,74.0845544572622,
74.1729891942819,74.2613329328369,74.3531601820264,74.4414015057085,74.5296293706705,
74.617865148658,74.7061302119854,74.7944956940387,74.8829206751001,74.9714761042681,
74.9959509263529,75.0845004696136,75.1729352066333,75.2612789451884,75.3531061943779,
75.44134751806,75.5295753830218,75.6178111610097,75.7060762243367,75.7944417063901,
75.8828666874513,75.9714221166195,75.9958969387043,76.0885121594138,76.1809656964412,
76.2732153511774,76.3653433520313,76.4573224600646,76.5082688970665),
 .UNSPECIFIED.);
#252=B_SPLINE_CURVE_WITH_KNOTS('',3,(#25649,#25650,#25651,#25652,#25653,
#25654,#25655,#25656,#25657,#25658,#25659,#25660,#25661,#25662,#25663,#25664,
#25665,#25666,#25667,#25668,#25669,#25670,#25671,#25672,#25673,#25674,#25675,
#25676,#25677,#25678,#25679,#25680,#25681,#25682,#25683,#25684,#25685,#25686,
#25687,#25688,#25689,#25690,#25691,#25692,#25693,#25694,#25695,#25696,#25697,
#25698,#25699,#25700,#25701,#25702,#25703,#25704,#25705,#25706,#25707,#25708,
#25709,#25710,#25711,#25712,#25713,#25714,#25715,#25716,#25717,#25718,#25719,
#25720,#25721,#25722,#25723,#25724,#25725,#25726,#25727,#25728,#25729,#25730,
#25731,#25732,#25733,#25734,#25735,#25736,#25737,#25738,#25739,#25740,#25741,
#25742,#25743,#25744,#25745,#25746,#25747,#25748,#25749,#25750,#25751,#25752,
#25753,#25754,#25755,#25756,#25757,#25758,#25759,#25760,#25761,#25762,#25763,
#25764,#25765,#25766,#25767,#25768,#25769,#25770,#25771,#25772,#25773,#25774,
#25775,#25776,#25777,#25778,#25779,#25780,#25781,#25782,#25783,#25784,#25785,
#25786,#25787,#25788,#25789,#25790,#25791,#25792,#25793,#25794,#25795,#25796,
#25797,#25798,#25799,#25800,#25801,#25802,#25803,#25804,#25805,#25806,#25807,
#25808,#25809,#25810,#25811,#25812,#25813,#25814,#25815,#25816,#25817,#25818,
#25819,#25820,#25821,#25822,#25823,#25824,#25825,#25826,#25827,#25828,#25829,
#25830,#25831,#25832,#25833,#25834,#25835,#25836,#25837,#25838,#25839,#25840,
#25841,#25842,#25843,#25844,#25845,#25846,#25847,#25848,#25849,#25850,#25851,
#25852,#25853,#25854,#25855,#25856,#25857,#25858,#25859,#25860,#25861,#25862,
#25863,#25864,#25865,#25866,#25867,#25868,#25869,#25870,#25871,#25872,#25873,
#25874),.UNSPECIFIED.,.F.,.F.,(4,3,3,3,3,3,3,3,3,3,3,3,3,3,3,3,3,3,3,3,
3,3,3,3,3,3,3,3,3,3,3,3,3,3,3,3,3,3,3,3,3,3,3,3,3,3,3,3,3,3,3,3,3,3,3,3,
3,3,3,3,3,3,3,3,3,3,3,3,3,3,3,3,3,3,3,4),(76.5082688972016,76.6011857099923,
76.6942510627784,76.7875594403697,76.8810035839464,76.9746605070459,76.9958429510557,
77.0843924943164,77.1728272313361,77.2611709698913,77.3529982190808,77.4412395427628,
77.5294674077249,77.6177031857127,77.70596824904,77.7943337310934,77.8827587121547,
77.9713141413228,77.9957889634071,78.0843385066678,78.1727732436875,78.2611169822426,
78.3529442314321,78.4411855551141,78.5294134200761,78.6176491980639,78.7059142613912,
78.7942797434445,78.8827047245058,78.9712601536739,78.9957349757584,79.0842845190191,
79.1727192560388,79.2610629945939,79.3528902437834,79.4411315674654,79.5293594324275,
79.6175952104153,79.7058602737426,79.794225755796,79.8826507368573,79.9712061660255,
79.9956809881098,80.0842305313706,80.1726652683903,80.2610090069454,80.3528362561349,
80.4410775798169,80.529305444779,80.6175412227668,80.7058062860941,80.7941717681475,
80.8825967492088,80.971152178377,80.9956270004612,81.0841765437219,81.1726112807416,
81.2609550192967,81.3527822684862,81.4410235921682,81.5292514571302,81.6174872351179,
81.7057522984453,81.7941177804986,81.8825427615599,81.9710981907281,81.9955730128125,
82.0828584263191,82.1714328985413,82.2585004412254,82.3455122336891,82.4324907952618,
82.5222316474705,82.6092419427961,82.7003480734463,82.7914542040965),
 .UNSPECIFIED.);
#253=B_SPLINE_CURVE_WITH_KNOTS('',3,(#25876,#25877,#25878,#25879,#25880,
#25881,#25882,#25883,#25884,#25885,#25886,#25887,#25888,#25889,#25890,#25891,
#25892,#25893,#25894,#25895,#25896,#25897,#25898,#25899,#25900,#25901,#25902,
#25903,#25904,#25905,#25906,#25907,#25908,#25909,#25910,#25911,#25912,#25913,
#25914,#25915,#25916,#25917,#25918,#25919,#25920,#25921,#25922,#25923,#25924,
#25925,#25926,#25927,#25928,#25929,#25930,#25931,#25932,#25933,#25934,#25935,
#25936,#25937,#25938,#25939,#25940,#25941,#25942,#25943,#25944,#25945,#25946,
#25947,#25948,#25949,#25950,#25951,#25952,#25953,#25954,#25955,#25956,#25957,
#25958,#25959,#25960,#25961,#25962,#25963,#25964,#25965,#25966,#25967,#25968,
#25969,#25970,#25971,#25972,#25973,#25974,#25975,#25976,#25977,#25978,#25979,
#25980,#25981,#25982,#25983,#25984,#25985,#25986,#25987,#25988,#25989,#25990,
#25991,#25992,#25993,#25994,#25995,#25996,#25997,#25998,#25999,#26000,#26001,
#26002,#26003,#26004,#26005,#26006,#26007,#26008,#26009,#26010,#26011,#26012,
#26013,#26014,#26015,#26016,#26017,#26018,#26019,#26020,#26021,#26022,#26023,
#26024,#26025,#26026,#26027,#26028,#26029,#26030,#26031,#26032,#26033,#26034,
#26035,#26036,#26037,#26038,#26039,#26040,#26041,#26042,#26043,#26044,#26045,
#26046,#26047,#26048,#26049,#26050,#26051,#26052,#26053,#26054,#26055,#26056,
#26057,#26058,#26059,#26060,#26061,#26062,#26063,#26064,#26065,#26066,#26067,
#26068,#26069,#26070,#26071,#26072,#26073,#26074,#26075,#26076,#26077,#26078,
#26079,#26080,#26081,#26082,#26083,#26084,#26085,#26086,#26087,#26088,#26089,
#26090,#26091,#26092,#26093,#26094,#26095,#26096,#26097,#26098,#26099,#26100,
#26101),.UNSPECIFIED.,.F.,.F.,(4,3,3,3,3,3,3,3,3,3,3,3,3,3,3,3,3,3,3,3,
3,3,3,3,3,3,3,3,3,3,3,3,3,3,3,3,3,3,3,3,3,3,3,3,3,3,3,3,3,3,3,3,3,3,3,3,
3,3,3,3,3,3,3,3,3,3,3,3,3,3,3,3,3,3,3,4),(82.7914542042461,82.9173221738109,
82.9955190251639,83.0840685684247,83.1725033054443,83.2608470439993,83.3526742931888,
83.4409156168709,83.529143481833,83.6173792598209,83.7056443231483,83.7940098052017,
83.882434786263,83.9709902154312,83.9954650375153,84.084014580776,84.1724493177957,
84.2607930563507,84.3526203055402,84.4408616292222,84.5290894941842,84.617325272172,
84.7055903354994,84.7939558175527,84.8823807986139,84.9709362277821,84.9954110498666,
85.0839605931273,85.172395330147,85.2607390687021,85.3525663178916,85.4408076415736,
85.5290355065357,85.6172712845235,85.7055363478508,85.7939018299042,85.8823268109655,
85.9708822401336,85.995357062218,86.0839066054788,86.1723413424985,86.2606850810536,
86.352512330243,86.4407536539251,86.5289815188871,86.617217296875,86.7054823602023,
86.7938478422556,86.8822728233169,86.9708282524851,86.9953030745694,87.0838526178302,
87.1722873548499,87.260631093405,87.3524583425945,87.4406996662765,87.5289275312386,
87.6171633092263,87.7054283725537,87.793793854607,87.8822188356683,87.9707742648366,
87.9952490869208,88.0837986301816,88.1722333672013,88.2605771057564,88.3524043549458,
88.4406456786279,88.5288735435899,88.6171093215776,88.7053743849048,88.7937398669581,
88.8821648480194,88.9707202771877,88.9951950992722,89.0746395114257),
 .UNSPECIFIED.);
#254=B_SPLINE_CURVE_WITH_KNOTS('',3,(#26103,#26104,#26105,#26106,#26107,
#26108,#26109,#26110,#26111,#26112),.UNSPECIFIED.,.F.,.F.,(4,1,1,1,1,1,
1,4),(89.0746480063059,89.9951411116235,90.9950871239749,91.9950331363263,
92.9949791486776,93.994925161029,94.9948711733804,95.3578171110057),
 .UNSPECIFIED.);
#255=B_SPLINE_CURVE_WITH_KNOTS('',3,(#26114,#26115,#26116,#26117,#26118,
#26119,#26120,#26121,#26122,#26123,#26124,#26125,#26126,#26127,#26128,#26129,
#26130,#26131,#26132,#26133,#26134,#26135,#26136,#26137,#26138,#26139,#26140,
#26141,#26142,#26143,#26144,#26145,#26146,#26147,#26148,#26149,#26150,#26151,
#26152,#26153,#26154,#26155,#26156,#26157,#26158,#26159,#26160,#26161,#26162,
#26163,#26164,#26165,#26166,#26167,#26168,#26169,#26170,#26171,#26172,#26173,
#26174,#26175,#26176,#26177,#26178,#26179,#26180,#26181,#26182,#26183,#26184,
#26185,#26186,#26187,#26188,#26189,#26190,#26191,#26192,#26193,#26194,#26195,
#26196,#26197,#26198,#26199,#26200,#26201,#26202,#26203,#26204,#26205,#26206,
#26207,#26208,#26209,#26210,#26211,#26212,#26213,#26214,#26215,#26216,#26217,
#26218,#26219,#26220,#26221,#26222,#26223,#26224,#26225,#26226,#26227,#26228,
#26229,#26230,#26231,#26232,#26233,#26234,#26235,#26236,#26237,#26238,#26239,
#26240,#26241,#26242,#26243,#26244,#26245,#26246,#26247,#26248,#26249,#26250,
#26251,#26252,#26253,#26254,#26255,#26256,#26257,#26258,#26259,#26260,#26261,
#26262,#26263,#26264,#26265,#26266,#26267,#26268,#26269,#26270,#26271,#26272,
#26273,#26274,#26275,#26276,#26277,#26278,#26279,#26280,#26281,#26282,#26283,
#26284,#26285,#26286,#26287,#26288,#26289,#26290,#26291,#26292,#26293,#26294,
#26295,#26296,#26297,#26298,#26299,#26300,#26301,#26302,#26303,#26304,#26305,
#26306,#26307,#26308,#26309,#26310,#26311,#26312,#26313,#26314,#26315,#26316,
#26317,#26318,#26319,#26320,#26321,#26322,#26323,#26324,#26325,#26326,#26327,
#26328,#26329,#26330,#26331,#26332,#26333,#26334,#26335,#26336,#26337,#26338,
#26339,#26340,#26341,#26342),.UNSPECIFIED.,.F.,.F.,(4,3,3,3,3,3,3,3,3,3,
3,3,3,3,3,3,3,3,3,3,3,3,3,3,3,3,3,3,3,3,3,3,3,3,3,3,3,3,3,3,3,3,3,3,3,3,
3,3,3,3,3,3,3,3,3,3,3,3,3,3,3,3,3,3,3,3,3,3,3,3,3,3,3,3,3,3,4),(95.3578248186053,
95.4464898257287,95.5351563461466,95.6238450600736,95.7165880914881,95.80543883478,
95.8943605288811,95.9834198358781,95.9948171857317,96.0833667289924,96.1718014660123,
96.2601452045674,96.3519724537569,96.4402137774389,96.528441642401,96.6166774203887,
96.7049424837157,96.793307965769,96.8817329468303,96.9702883759985,96.9947631980831,
97.0833127413439,97.1717474783636,97.2600912169187,97.3519184661082,97.4401597897902,
97.5283876547524,97.6166234327403,97.7048884960678,97.7932539781212,97.8816789591828,
97.970234388351,97.9947092104345,98.0832587536953,98.1716934907152,98.2600372292703,
98.3518644784597,98.4401058021418,98.5283336671038,98.6165694450914,98.7048345084186,
98.793199990472,98.8816249715333,98.9701804007016,98.9946552227859,99.0832047660465,
99.1716395030662,99.2599832416215,99.3518104908109,99.4400518144929,99.5282796794549,
99.6165154574425,99.7047805207696,99.793146002823,99.8815709838841,99.9701264130522,
99.9946012351372,100.083150778398,100.171585515418,100.259929253973,100.351756503162,
100.439997826844,100.528225691807,100.616461469795,100.704726533122,100.793092015175,
100.881516996236,100.970072425405,100.994547247489,101.083392821799,101.172123155493,
101.260759394379,101.349322607109,101.437835030598,101.526318499633,101.614805634129,
101.641010125785),.UNSPECIFIED.);
#256=B_SPLINE_CURVE_WITH_KNOTS('',3,(#26344,#26345,#26346,#26347,#26348,
#26349,#26350,#26351,#26352,#26353,#26354,#26355,#26356,#26357,#26358,#26359,
#26360,#26361,#26362,#26363,#26364,#26365,#26366,#26367,#26368,#26369,#26370,
#26371,#26372,#26373,#26374,#26375,#26376,#26377,#26378,#26379,#26380,#26381,
#26382,#26383,#26384,#26385,#26386,#26387,#26388,#26389,#26390,#26391,#26392,
#26393,#26394,#26395,#26396,#26397,#26398,#26399,#26400,#26401,#26402,#26403,
#26404,#26405,#26406,#26407,#26408,#26409,#26410,#26411,#26412,#26413,#26414,
#26415,#26416,#26417,#26418,#26419,#26420,#26421,#26422,#26423,#26424,#26425,
#26426,#26427,#26428,#26429,#26430,#26431,#26432,#26433,#26434,#26435,#26436,
#26437,#26438,#26439,#26440,#26441,#26442,#26443,#26444,#26445,#26446,#26447,
#26448,#26449,#26450,#26451,#26452,#26453,#26454,#26455,#26456,#26457,#26458,
#26459,#26460,#26461,#26462,#26463,#26464,#26465,#26466,#26467,#26468,#26469,
#26470,#26471,#26472,#26473,#26474,#26475,#26476,#26477,#26478,#26479,#26480,
#26481,#26482,#26483,#26484,#26485,#26486,#26487,#26488,#26489,#26490,#26491,
#26492,#26493,#26494,#26495,#26496,#26497,#26498,#26499,#26500,#26501,#26502,
#26503,#26504,#26505,#26506,#26507,#26508,#26509,#26510,#26511,#26512,#26513,
#26514,#26515,#26516,#26517,#26518,#26519,#26520,#26521,#26522,#26523,#26524,
#26525,#26526,#26527,#26528,#26529,#26530,#26531,#26532,#26533,#26534,#26535,
#26536,#26537,#26538,#26539,#26540,#26541,#26542,#26543,#26544,#26545,#26546,
#26547,#26548,#26549,#26550,#26551,#26552,#26553,#26554,#26555,#26556,#26557,
#26558,#26559,#26560,#26561,#26562,#26563,#26564,#26565,#26566,#26567,#26568,
#26569),.UNSPECIFIED.,.F.,.F.,(4,3,3,3,3,3,3,3,3,3,3,3,3,3,3,3,3,3,3,3,
3,3,3,3,3,3,3,3,3,3,3,3,3,3,3,3,3,3,3,3,3,3,3,3,3,3,3,3,3,3,3,3,3,3,3,3,
3,3,3,3,3,3,3,3,3,3,3,3,3,3,3,3,3,3,3,4),(101.641010126018,101.742054504281,
101.843610345288,101.945794784302,101.99449325984,102.083042803101,102.17147754012,
102.259821278675,102.351648527865,102.439889851546,102.528117716508,102.616353494496,
102.704618557823,102.792984039877,102.881409020938,102.969964450106,102.994439272191,
103.082988815452,103.171423552472,103.259767291027,103.351594540217,103.439835863899,
103.528063728861,103.616299506849,103.704564570177,103.79293005223,103.881355033292,
103.96991046246,103.994385284543,104.082934827804,104.171369564823,104.259713303379,
104.351540552568,104.43978187625,104.528009741212,104.6162455192,104.704510582527,
104.792876064581,104.881301045642,104.96985647481,104.994331296894,105.082880840154,
105.171315577174,105.259659315729,105.351486564918,105.4397278886,105.527955753562,
105.616191531549,105.704456594876,105.79282207693,105.881247057991,105.969802487158,
105.994277309245,106.082826852506,106.171261589526,106.259605328081,106.351432577271,
106.439673900953,106.527901765915,106.616137543904,106.704402607231,106.792768089285,
106.881193070346,106.969748499515,106.994223321597,107.081894309482,107.169451242158,
107.256918854214,107.344323253543,107.43169496891,107.519056200791,107.606429136683,
107.693885954662,107.781388212332,107.869020538835,107.924195432964),
 .UNSPECIFIED.);
#257=B_SPLINE_CURVE_WITH_KNOTS('',3,(#26571,#26572,#26573,#26574,#26575,
#26576,#26577,#26578,#26579,#26580,#26581),.UNSPECIFIED.,.F.,.F.,(4,1,1,
1,1,1,1,1,4),(107.924195432964,107.994169333948,108.9941153463,109.994061358651,
110.994007371002,111.993953383354,112.993899395705,113.993845408056,114.207380740144),
 .UNSPECIFIED.);
#258=B_SPLINE_CURVE_WITH_KNOTS('',3,(#26583,#26584,#26585,#26586,#26587,
#26588,#26589,#26590,#26591,#26592),.UNSPECIFIED.,.F.,.F.,(4,1,1,1,1,1,
1,4),(114.207380740144,114.993791420408,115.993737432759,116.993683445111,
117.993629457462,118.993575469813,119.993521482165,120.490566047324),
 .UNSPECIFIED.);
#259=B_SPLINE_CURVE_WITH_KNOTS('',3,(#26594,#26595,#26596,#26597,#26598,
#26599,#26600,#26601,#26602,#26603),.UNSPECIFIED.,.F.,.F.,(4,1,1,1,1,1,
1,4),(120.490566047324,120.993467494516,121.993413506867,122.993359519219,
123.99330553157,124.993251543922,125.993197556273,126.773751354503),
 .UNSPECIFIED.);
#260=B_SPLINE_CURVE_WITH_KNOTS('',3,(#26605,#26606,#26607,#26608,#26609,
#26610,#26611,#26612,#26613,#26614,#26615),.UNSPECIFIED.,.F.,.F.,(4,1,1,
1,1,1,1,1,4),(126.773751354503,126.993143568624,127.993089580976,128.993035593327,
129.992981605678,130.99292761803,131.992873630381,132.992819642733,133.056936661683),
 .UNSPECIFIED.);
#261=B_SPLINE_CURVE_WITH_KNOTS('',3,(#26617,#26618,#26619,#26620,#26621,
#26622,#26623,#26624,#26625,#26626,#26627,#26628,#26629,#26630,#26631,#26632,
#26633,#26634,#26635,#26636,#26637,#26638,#26639,#26640,#26641,#26642,#26643,
#26644,#26645,#26646,#26647,#26648,#26649,#26650,#26651,#26652,#26653,#26654,
#26655,#26656,#26657,#26658,#26659,#26660,#26661,#26662,#26663,#26664,#26665,
#26666,#26667,#26668,#26669,#26670,#26671,#26672,#26673,#26674,#26675,#26676,
#26677,#26678,#26679,#26680,#26681,#26682,#26683,#26684,#26685,#26686,#26687,
#26688,#26689,#26690,#26691,#26692,#26693,#26694,#26695,#26696,#26697,#26698,
#26699,#26700,#26701,#26702,#26703,#26704,#26705,#26706,#26707,#26708,#26709,
#26710,#26711,#26712,#26713,#26714,#26715,#26716,#26717,#26718,#26719,#26720,
#26721,#26722,#26723,#26724,#26725,#26726,#26727,#26728,#26729,#26730,#26731,
#26732,#26733,#26734,#26735,#26736,#26737,#26738,#26739,#26740,#26741,#26742,
#26743,#26744,#26745,#26746,#26747,#26748,#26749,#26750,#26751,#26752,#26753,
#26754,#26755,#26756,#26757,#26758,#26759,#26760,#26761,#26762,#26763,#26764,
#26765,#26766,#26767,#26768,#26769,#26770,#26771,#26772,#26773,#26774,#26775,
#26776,#26777,#26778,#26779,#26780,#26781,#26782,#26783,#26784,#26785,#26786,
#26787,#26788,#26789,#26790,#26791,#26792,#26793,#26794,#26795,#26796,#26797,
#26798,#26799,#26800,#26801,#26802,#26803,#26804,#26805,#26806,#26807,#26808,
#26809,#26810,#26811,#26812,#26813,#26814,#26815,#26816,#26817,#26818,#26819,
#26820,#26821,#26822,#26823,#26824,#26825,#26826,#26827,#26828,#26829,#26830,
#26831,#26832,#26833,#26834,#26835,#26836,#26837,#26838,#26839,#26840,#26841,
#26842),.UNSPECIFIED.,.F.,.F.,(4,3,3,3,3,3,3,3,3,3,3,3,3,3,3,3,3,3,3,3,
3,3,3,3,3,3,3,3,3,3,3,3,3,3,3,3,3,3,3,3,3,3,3,3,3,3,3,3,3,3,3,3,3,3,3,3,
3,3,3,3,3,3,3,3,3,3,3,3,3,3,3,3,3,3,3,4),(133.056936661683,133.144638878716,
133.232231781202,133.319740031263,133.407192196977,133.494615948175,133.58203343827,
133.669466811322,133.756991613018,133.844565328127,133.932277736142,133.992765655084,
134.081315198345,134.169749935364,134.258093673919,134.349920923109,134.438162246791,
134.526390111752,134.61462588974,134.702890953068,134.791256435121,134.879681416182,
134.96823684535,134.992711667435,135.081261210696,135.169695947716,135.258039686271,
135.34986693546,135.438108259143,135.526336124105,135.614571902093,135.70283696542,
135.791202447473,135.879627428534,135.968182857703,135.992657679787,136.081207223048,
136.169641960068,136.257985698623,136.349812947812,136.438054271494,136.526282136456,
136.614517914444,136.702782977771,136.791148459825,136.879573440886,136.968128870055,
136.992603692138,137.081153235398,137.169587972418,137.257931710973,137.349758960162,
137.438000283844,137.526228148806,137.614463926793,137.702728990121,137.791094472174,
137.879519453235,137.968074882403,137.992549704489,138.08109924775,138.16953398477,
138.257877723325,138.349704972515,138.437946296197,138.526174161159,138.614409939148,
138.702675002476,138.791040484529,138.879465465591,138.968020894759,138.992495716841,
139.095160517603,139.197384563926,139.29881023738,139.340121968631),
 .UNSPECIFIED.);
#262=B_SPLINE_CURVE_WITH_KNOTS('',3,(#26844,#26845,#26846,#26847,#26848,
#26849,#26850,#26851,#26852,#26853,#26854,#26855,#26856,#26857,#26858,#26859,
#26860,#26861,#26862,#26863,#26864,#26865,#26866,#26867,#26868,#26869,#26870,
#26871,#26872,#26873,#26874,#26875,#26876,#26877,#26878,#26879,#26880,#26881,
#26882,#26883,#26884,#26885,#26886,#26887,#26888,#26889,#26890,#26891,#26892,
#26893,#26894,#26895,#26896,#26897,#26898,#26899,#26900,#26901,#26902,#26903,
#26904,#26905,#26906,#26907,#26908,#26909,#26910,#26911,#26912,#26913,#26914,
#26915,#26916,#26917,#26918,#26919,#26920,#26921,#26922,#26923,#26924,#26925,
#26926,#26927,#26928,#26929,#26930,#26931,#26932,#26933,#26934,#26935,#26936,
#26937,#26938,#26939,#26940,#26941,#26942,#26943,#26944,#26945,#26946,#26947,
#26948,#26949,#26950,#26951,#26952,#26953,#26954,#26955,#26956,#26957,#26958,
#26959,#26960,#26961,#26962,#26963,#26964,#26965,#26966,#26967,#26968,#26969,
#26970,#26971,#26972,#26973,#26974,#26975,#26976,#26977,#26978,#26979,#26980,
#26981,#26982,#26983,#26984,#26985,#26986,#26987,#26988,#26989,#26990,#26991,
#26992,#26993,#26994,#26995,#26996,#26997,#26998,#26999,#27000,#27001,#27002,
#27003,#27004,#27005,#27006,#27007,#27008,#27009,#27010,#27011,#27012,#27013,
#27014,#27015,#27016,#27017,#27018,#27019,#27020,#27021,#27022,#27023,#27024,
#27025,#27026,#27027,#27028,#27029,#27030,#27031,#27032,#27033,#27034,#27035,
#27036,#27037,#27038,#27039,#27040,#27041,#27042,#27043,#27044,#27045,#27046,
#27047,#27048,#27049,#27050,#27051,#27052,#27053,#27054,#27055,#27056,#27057,
#27058,#27059,#27060,#27061,#27062,#27063,#27064,#27065,#27066,#27067,#27068,
#27069),.UNSPECIFIED.,.F.,.F.,(4,3,3,3,3,3,3,3,3,3,3,3,3,3,3,3,3,3,3,3,
3,3,3,3,3,3,3,3,3,3,3,3,3,3,3,3,3,3,3,3,3,3,3,3,3,3,3,3,3,3,3,3,3,3,3,3,
3,3,3,3,3,3,3,3,3,3,3,3,3,3,3,3,3,3,3,4),(139.340121968862,139.428521800617,
139.516914594785,139.605321416591,139.693763336218,139.782315552249,139.870931673301,
139.95968890979,139.992441729192,140.080991272453,140.169426009473,140.257769748028,
140.349596997217,140.4378383209,140.526066185862,140.61430196385,140.702567027178,
140.790932509231,140.879357490293,140.967912919461,140.992387741544,141.080937284805,
141.169372021824,141.257715760379,141.349543009569,141.437784333251,141.526012198212,
141.6142479762,141.702513039528,141.790878521581,141.879303502642,141.96785893181,
141.992333753895,142.080883297156,142.169318034175,142.257661772731,142.34948902192,
142.437730345602,142.525958210564,142.614193988552,142.702459051879,142.790824533932,
142.879249514994,142.967804944162,142.992279766246,143.080829309507,143.169264046527,
143.257607785082,143.349435034271,143.437676357953,143.525904222915,143.614140000903,
143.70240506423,143.790770546284,143.879195527345,143.967750956513,143.992225778598,
144.080775321858,144.169210058877,144.257553797432,144.349381046622,144.437622370303,
144.525850235265,144.614086013251,144.702351076578,144.79071655863,144.879141539691,
144.967696968859,144.992171790949,145.081319122906,145.170348342848,145.259280195558,
145.350286965679,145.439082830911,145.531195053476,145.623307276042),
 .UNSPECIFIED.);
#263=B_SPLINE_CURVE_WITH_KNOTS('',3,(#27071,#27072,#27073,#27074,#27075,
#27076,#27077,#27078,#27079,#27080),.UNSPECIFIED.,.F.,.F.,(4,1,1,1,1,1,
1,4),(145.623314962503,145.9921178033,146.992063815652,147.992009828003,
148.991955840354,149.991901852706,150.991847865057,151.906483871255),
 .UNSPECIFIED.);
#264=B_SPLINE_CURVE_WITH_KNOTS('',3,(#27082,#27083,#27084,#27085,#27086,
#27087,#27088,#27089,#27090,#27091,#27092,#27093,#27094,#27095,#27096,#27097,
#27098,#27099,#27100,#27101,#27102,#27103,#27104,#27105,#27106,#27107,#27108,
#27109,#27110,#27111,#27112,#27113,#27114,#27115,#27116,#27117,#27118,#27119,
#27120,#27121,#27122,#27123,#27124,#27125,#27126,#27127,#27128,#27129,#27130,
#27131,#27132,#27133,#27134,#27135,#27136,#27137,#27138,#27139,#27140,#27141,
#27142,#27143,#27144,#27145,#27146,#27147,#27148,#27149,#27150,#27151,#27152,
#27153,#27154,#27155,#27156,#27157,#27158,#27159,#27160,#27161,#27162,#27163,
#27164,#27165,#27166,#27167,#27168,#27169,#27170,#27171,#27172,#27173,#27174,
#27175,#27176,#27177,#27178,#27179,#27180,#27181,#27182,#27183,#27184,#27185,
#27186,#27187,#27188,#27189,#27190,#27191,#27192,#27193,#27194,#27195,#27196,
#27197,#27198,#27199,#27200,#27201,#27202,#27203,#27204,#27205,#27206,#27207,
#27208,#27209,#27210,#27211,#27212,#27213,#27214,#27215,#27216,#27217,#27218,
#27219,#27220,#27221,#27222,#27223,#27224,#27225,#27226,#27227,#27228,#27229,
#27230,#27231,#27232,#27233,#27234,#27235,#27236,#27237,#27238,#27239,#27240,
#27241,#27242,#27243,#27244,#27245,#27246,#27247,#27248,#27249,#27250,#27251,
#27252,#27253,#27254,#27255,#27256,#27257,#27258,#27259,#27260,#27261,#27262,
#27263,#27264,#27265,#27266,#27267,#27268,#27269,#27270,#27271,#27272,#27273,
#27274,#27275,#27276,#27277,#27278,#27279,#27280,#27281,#27282,#27283,#27284,
#27285,#27286,#27287,#27288,#27289,#27290,#27291,#27292,#27293,#27294,#27295,
#27296,#27297,#27298,#27299,#27300,#27301,#27302,#27303,#27304,#27305,#27306,
#27307),.UNSPECIFIED.,.F.,.F.,(4,3,3,3,3,3,3,3,3,3,3,3,3,3,3,3,3,3,3,3,
3,3,3,3,3,3,3,3,3,3,3,3,3,3,3,3,3,3,3,3,3,3,3,3,3,3,3,3,3,3,3,3,3,3,3,3,
3,3,3,3,3,3,3,3,3,3,3,3,3,3,3,3,3,3,3,4),(151.906492583222,151.991793877409,
152.080343420566,152.168778157483,152.257121895935,152.348949145163,152.437190468744,
152.525418333606,152.613654111494,152.701919174722,152.790284656678,152.878709637644,
152.967265066718,152.99173988976,153.080289432964,153.168724169926,153.257067908422,
153.348895157633,153.437136481254,153.525364346154,153.61360012408,153.701865187344,
153.790230669334,153.878655650331,153.967211079435,153.991685902111,154.08023544587,
154.16867018339,154.257013922446,154.348841171448,154.43708249563,154.52531036109,
154.613546139575,154.701811203397,154.790176685939,154.878601667486,154.967157097132,
154.991631914463,155.080181456899,155.168616193095,155.256959930829,155.348787180327,
155.437028503198,155.525256367354,155.613492144542,155.701757207076,155.79012268835,
155.878547668639,155.967103097051,155.991577926814,156.080127469951,156.168562206839,
156.256905945255,156.348733194494,156.43697451802,156.525202382819,156.613438160639,
156.701703223792,156.790068705663,156.878493686538,156.967049115515,156.991523939165,
157.080073485715,157.168508226035,157.256851967898,157.34867921585,157.436920542839,
157.525148411102,157.613384192381,157.701649258987,157.790014744282,157.87843972857,
157.966995160914,157.991469951517,158.119206215025,158.189677890401),
 .UNSPECIFIED.);
#265=B_SPLINE_CURVE_WITH_KNOTS('',3,(#27309,#27310,#27311,#27312,#27313,
#27314,#27315,#27316,#27317,#27318),.UNSPECIFIED.,.F.,.F.,(4,1,1,1,1,1,
1,4),(158.189681389038,158.991415963868,159.99136197622,160.991307988571,
161.991254000922,162.991200013274,163.991146025625,164.472861769939),
 .UNSPECIFIED.);
#266=B_SPLINE_CURVE_WITH_KNOTS('',3,(#27320,#27321,#27322,#27323,#27324,
#27325,#27326,#27327,#27328,#27329,#27330,#27331,#27332,#27333,#27334,#27335,
#27336,#27337,#27338,#27339,#27340,#27341,#27342,#27343,#27344,#27345,#27346,
#27347,#27348,#27349,#27350,#27351,#27352,#27353,#27354,#27355,#27356,#27357,
#27358,#27359,#27360,#27361,#27362,#27363,#27364,#27365,#27366,#27367,#27368,
#27369,#27370,#27371,#27372,#27373,#27374,#27375,#27376,#27377,#27378,#27379,
#27380,#27381,#27382,#27383,#27384,#27385,#27386,#27387,#27388,#27389,#27390,
#27391,#27392,#27393,#27394,#27395,#27396,#27397,#27398,#27399,#27400,#27401,
#27402,#27403,#27404,#27405,#27406,#27407,#27408,#27409,#27410,#27411,#27412,
#27413,#27414,#27415,#27416,#27417,#27418,#27419,#27420,#27421,#27422,#27423,
#27424,#27425,#27426,#27427,#27428,#27429,#27430,#27431,#27432,#27433,#27434,
#27435,#27436,#27437,#27438,#27439,#27440,#27441,#27442,#27443,#27444,#27445,
#27446,#27447,#27448,#27449,#27450,#27451,#27452,#27453,#27454,#27455,#27456,
#27457,#27458,#27459,#27460,#27461,#27462,#27463,#27464,#27465,#27466,#27467,
#27468,#27469,#27470,#27471,#27472,#27473,#27474,#27475,#27476,#27477,#27478,
#27479,#27480,#27481,#27482,#27483,#27484,#27485,#27486,#27487,#27488,#27489,
#27490,#27491,#27492,#27493,#27494,#27495,#27496,#27497,#27498,#27499,#27500,
#27501,#27502,#27503,#27504,#27505,#27506,#27507,#27508,#27509,#27510,#27511,
#27512,#27513,#27514,#27515,#27516,#27517,#27518,#27519,#27520,#27521,#27522,
#27523,#27524,#27525,#27526,#27527,#27528,#27529,#27530,#27531,#27532,#27533,
#27534,#27535,#27536,#27537,#27538,#27539,#27540,#27541,#27542,#27543,#27544,
#27545),.UNSPECIFIED.,.F.,.F.,(4,3,3,3,3,3,3,3,3,3,3,3,3,3,3,3,3,3,3,3,
3,3,3,3,3,3,3,3,3,3,3,3,3,3,3,3,3,3,3,3,3,3,3,3,3,3,3,3,3,3,3,3,3,3,3,3,
3,3,3,3,3,3,3,3,3,3,3,3,3,3,3,3,3,3,3,4),(164.472863197581,164.564620554491,
164.656481689159,164.748542726059,164.840710752793,164.933083630566,164.991092037976,
165.079641825262,165.168076804179,165.256420782257,165.348247940766,165.436489496637,
165.524717590711,165.612953594507,165.701218880108,165.78958457811,165.87800977171,
165.966565406784,165.991038050328,166.079588379573,166.168023907756,166.256368441678,
166.348195394303,166.436437518814,166.524666185258,166.612902764528,166.701168628086,
166.789534904754,166.877960678146,166.966516890119,166.990984062679,167.079531079788,
167.167963287752,167.256304497273,167.348132694493,167.436371504789,167.524596866325,
167.612830153446,167.701092741073,167.789455782318,167.877878339832,167.966431389575,
167.990930075031,168.079481963654,168.167919033012,168.256265088403,168.348091463276,
168.436335051259,168.524565157465,168.612803151383,168.701070403051,168.789438021748,
168.877865112049,168.966422594011,168.990876087382,169.079430061653,169.167869267384,
169.256217506719,169.348043080846,169.436288956627,169.524521384817,169.612761732272,
169.701031366421,169.789401398027,169.877830921893,169.966390848492,169.990822099733,
170.078237539823,170.165512518093,170.252707282048,170.339844321629,170.426946068895,
170.514063004851,170.601185227643,170.688382092216,170.75604850476),
 .UNSPECIFIED.);
#267=B_SPLINE_CURVE_WITH_KNOTS('',3,(#27547,#27548,#27549,#27550,#27551,
#27552,#27553,#27554,#27555,#27556,#27557,#27558,#27559,#27560,#27561,#27562,
#27563,#27564,#27565,#27566,#27567,#27568,#27569,#27570,#27571,#27572,#27573,
#27574,#27575,#27576,#27577,#27578,#27579,#27580,#27581,#27582,#27583,#27584,
#27585,#27586,#27587,#27588,#27589,#27590,#27591,#27592,#27593,#27594,#27595,
#27596,#27597,#27598,#27599,#27600,#27601,#27602,#27603,#27604,#27605,#27606,
#27607,#27608,#27609,#27610,#27611,#27612,#27613,#27614,#27615,#27616,#27617,
#27618,#27619,#27620,#27621,#27622,#27623,#27624,#27625,#27626,#27627,#27628,
#27629,#27630,#27631,#27632,#27633,#27634,#27635,#27636,#27637,#27638,#27639,
#27640,#27641,#27642,#27643,#27644,#27645,#27646,#27647,#27648,#27649,#27650,
#27651,#27652,#27653,#27654,#27655,#27656,#27657,#27658,#27659,#27660,#27661,
#27662,#27663,#27664,#27665,#27666,#27667,#27668,#27669,#27670,#27671,#27672,
#27673,#27674,#27675,#27676,#27677,#27678,#27679,#27680,#27681,#27682,#27683,
#27684,#27685,#27686,#27687,#27688,#27689,#27690,#27691,#27692,#27693,#27694,
#27695,#27696,#27697,#27698,#27699,#27700,#27701,#27702,#27703,#27704,#27705,
#27706,#27707,#27708,#27709,#27710,#27711,#27712,#27713,#27714,#27715,#27716,
#27717,#27718,#27719,#27720,#27721,#27722,#27723,#27724,#27725,#27726,#27727,
#27728,#27729,#27730),.UNSPECIFIED.,.F.,.F.,(4,3,3,3,3,3,3,3,3,3,3,3,3,
3,3,3,3,3,3,3,3,3,3,3,3,3,3,3,3,3,3,3,3,3,3,3,3,3,3,3,3,3,3,3,3,3,3,3,3,
3,3,3,3,3,3,3,3,3,3,3,3,4),(170.756048504935,170.873914600802,170.990768112085,
171.079338276875,171.16779355935,171.256157744839,171.347977292289,171.436238693458,
171.524486466626,171.612741963255,171.701026535212,171.789411117863,171.87785498588,
171.966428842985,171.990714124436,172.079286474888,172.167744288444,172.256111342656,
172.347929941922,172.436195026618,172.524446775571,172.612706534521,172.700995649825,
172.789385165724,172.877834199635,172.966413521211,172.990660136787,173.079086910887,
173.167398611765,173.255619188468,173.347492558552,173.435611157336,173.523716659296,
173.611830560963,173.699974359953,173.788220091732,173.876526050693,173.964964454657,
173.990606149139,174.079327458897,174.167933535642,174.256447991984,174.348211013172,
174.436620444989,174.525015168666,174.613416380147,174.701845274749,174.790371395654,
174.878955350467,174.967666093791,174.99055216149,175.078366871321,175.16606918391,
175.25368368237,175.34123713241,175.428759059388,175.51627153865,175.603796633468,
175.691408265889,175.779065855606,175.866858195123,175.92887515605),
 .UNSPECIFIED.);
#268=B_SPLINE_CURVE_WITH_KNOTS('',3,(#27734,#27735,#27736,#27737,#27738,
#27739,#27740,#27741),.UNSPECIFIED.,.F.,.F.,(4,1,1,1,1,4),(-177.990390198544,
-176.990444186193,-175.990498173842,-174.99055216149,-173.990606149139,
-173.73875440895),.UNSPECIFIED.);
#269=B_SPLINE_CURVE_WITH_KNOTS('',3,(#27743,#27744,#27745,#27746,#27747,
#27748,#27749,#27750,#27751,#27752,#27753,#27754,#27755,#27756,#27757,#27758,
#27759,#27760,#27761,#27762,#27763,#27764,#27765,#27766,#27767,#27768,#27769,
#27770,#27771,#27772,#27773,#27774,#27775,#27776,#27777,#27778,#27779,#27780,
#27781,#27782,#27783,#27784,#27785,#27786,#27787,#27788,#27789,#27790,#27791,
#27792,#27793,#27794,#27795,#27796,#27797,#27798,#27799,#27800,#27801,#27802,
#27803,#27804,#27805,#27806,#27807,#27808,#27809,#27810,#27811,#27812,#27813,
#27814,#27815,#27816,#27817,#27818,#27819,#27820,#27821,#27822,#27823,#27824,
#27825,#27826,#27827,#27828,#27829,#27830,#27831,#27832,#27833,#27834,#27835,
#27836,#27837,#27838,#27839,#27840,#27841,#27842,#27843,#27844,#27845,#27846,
#27847,#27848,#27849,#27850,#27851,#27852,#27853,#27854,#27855,#27856,#27857,
#27858,#27859,#27860,#27861,#27862,#27863,#27864,#27865,#27866,#27867,#27868,
#27869,#27870,#27871,#27872,#27873,#27874,#27875,#27876,#27877,#27878,#27879,
#27880,#27881,#27882,#27883,#27884,#27885,#27886,#27887,#27888,#27889,#27890,
#27891,#27892,#27893,#27894,#27895,#27896,#27897,#27898,#27899,#27900,#27901,
#27902,#27903,#27904,#27905,#27906,#27907,#27908,#27909,#27910,#27911,#27912,
#27913,#27914,#27915,#27916,#27917,#27918,#27919,#27920,#27921,#27922,#27923,
#27924,#27925,#27926,#27927,#27928,#27929,#27930,#27931,#27932,#27933,#27934,
#27935,#27936,#27937,#27938,#27939,#27940,#27941,#27942,#27943,#27944,#27945,
#27946,#27947,#27948,#27949,#27950,#27951,#27952,#27953,#27954,#27955,#27956,
#27957,#27958,#27959,#27960,#27961,#27962,#27963,#27964,#27965,#27966,#27967,
#27968),.UNSPECIFIED.,.F.,.F.,(4,3,3,3,3,3,3,3,3,3,3,3,3,3,3,3,3,3,3,3,
3,3,3,3,3,3,3,3,3,3,3,3,3,3,3,3,3,3,3,3,3,3,3,3,3,3,3,3,3,3,3,3,3,3,3,3,
3,3,3,3,3,3,3,3,3,3,3,3,3,3,3,3,3,3,3,4),(-173.738752334043,-173.651535863068,
-173.564373232163,-173.477237355581,-173.39010587623,-173.302956444482,
-173.215714308532,-173.128421050025,-173.040991470072,-172.990660136787,
-172.902086758176,-172.813628104058,-172.725260396143,-172.63344211218,
-172.545176843568,-172.456925084215,-172.368665488387,-172.280376709863,
-172.191987786504,-172.103539494695,-172.01496112903,-171.990714124436,
-171.90214620507,-171.81369273751,-171.725329938254,-171.633509709983,-171.545248617959,
-171.45700075632,-171.368744773707,-171.280459318054,-171.192073266518,
-171.103627587279,-171.015051430389,-170.990768112085,-170.902235390015,
-170.813817694881,-170.725491197375,-170.63365756017,-170.545433867796,
-170.457223748581,-170.369005812376,-170.280758668513,-170.192411131339,
-170.10400413231,-170.01546660041,-169.990822099733,-169.902268068231,-169.8138288144,
-169.72548053607,-169.633654979984,-169.545409088144,-169.457176652377,
-169.368936305834,-169.280666681103,-169.192296671475,-169.103867176925,
-169.015307290188,-168.990876087382,-168.902324496367,-168.813887667493,
-168.725541795705,-168.633715330621,-168.545471783305,-168.457241665011,
-168.369003606262,-168.280736236998,-168.192368423046,-168.103941092068,
-168.015383304581,-167.99093007503,-167.899167922216,-167.807554835821,
-167.716121750623,-167.624794219276,-167.533586961915,-167.455567026863),
 .UNSPECIFIED.);
#270=B_SPLINE_CURVE_WITH_KNOTS('',3,(#27970,#27971,#27972,#27973,#27974,
#27975,#27976,#27977,#27978,#27979,#27980,#27981,#27982,#27983,#27984,#27985,
#27986,#27987,#27988,#27989,#27990,#27991,#27992,#27993,#27994,#27995,#27996,
#27997,#27998,#27999,#28000,#28001,#28002,#28003,#28004,#28005,#28006,#28007,
#28008,#28009,#28010,#28011,#28012,#28013,#28014,#28015,#28016,#28017,#28018,
#28019,#28020,#28021,#28022,#28023,#28024,#28025,#28026,#28027,#28028,#28029,
#28030,#28031,#28032,#28033,#28034,#28035,#28036,#28037,#28038,#28039,#28040,
#28041,#28042,#28043,#28044,#28045,#28046,#28047,#28048,#28049,#28050,#28051,
#28052,#28053,#28054,#28055,#28056,#28057,#28058,#28059,#28060,#28061,#28062,
#28063,#28064,#28065,#28066,#28067,#28068,#28069,#28070,#28071,#28072,#28073,
#28074,#28075,#28076,#28077,#28078,#28079,#28080,#28081,#28082,#28083,#28084,
#28085,#28086,#28087,#28088,#28089,#28090,#28091,#28092,#28093,#28094,#28095,
#28096,#28097,#28098,#28099,#28100,#28101,#28102,#28103,#28104,#28105,#28106,
#28107,#28108,#28109,#28110,#28111,#28112,#28113,#28114,#28115,#28116,#28117,
#28118,#28119,#28120,#28121,#28122,#28123,#28124,#28125,#28126,#28127,#28128,
#28129,#28130,#28131,#28132,#28133,#28134,#28135,#28136,#28137,#28138,#28139,
#28140,#28141,#28142,#28143,#28144,#28145,#28146,#28147,#28148,#28149,#28150,
#28151,#28152,#28153,#28154,#28155,#28156,#28157,#28158,#28159,#28160,#28161,
#28162,#28163,#28164,#28165,#28166,#28167,#28168,#28169,#28170,#28171,#28172,
#28173,#28174,#28175,#28176,#28177,#28178,#28179,#28180,#28181,#28182,#28183,
#28184,#28185,#28186,#28187,#28188,#28189,#28190,#28191,#28192,#28193,#28194,
#28195),.UNSPECIFIED.,.F.,.F.,(4,3,3,3,3,3,3,3,3,3,3,3,3,3,3,3,3,3,3,3,
3,3,3,3,3,3,3,3,3,3,3,3,3,3,3,3,3,3,3,3,3,3,3,3,3,3,3,3,3,3,3,3,3,3,3,3,
3,3,3,3,3,3,3,3,3,3,3,3,3,3,3,3,3,3,3,4),(-167.455567026675,-167.36166117942,
-167.26743965224,-167.173059830492,-167.078395851896,-166.990984062679,
-166.902433737907,-166.813998212985,-166.72565368112,-166.633826727271,
-166.545584601802,-166.457355933291,-166.369119350847,-166.280853483008,
-166.19248720044,-166.1040614202,-166.015505200038,-165.991038050328,-165.902488301604,
-165.814053353852,-165.725709399573,-165.633882229373,-165.54564067879,
-165.457412583173,-165.369176571003,-165.280911270194,-165.192545546928,
-165.104120322181,-165.015564647562,-164.991092037976,-164.902542823081,
-164.814108419134,-164.725765017936,-164.633937643897,-164.545696666176,
-164.457469149771,-164.369233722574,-164.280969011912,-164.19260388354,
-164.104179257191,-164.015624181504,-163.991146025625,-163.902596353175,
-163.814161485746,-163.725817615724,-163.633990415418,-163.545748958459,
-163.457520959779,-163.369285047773,-163.281019850269,-163.19265423448,
-163.104229119776,-163.015673558138,-162.991200013274,-162.902650453511,
-162.814215699397,-162.725871943178,-162.634044700396,-162.545803357729,
-162.457575473325,-162.369339675457,-162.281074591829,-162.192709088949,
-162.10428408673,-162.015728636077,-161.991254000922,-161.904020167719,
-161.812565361731,-161.72554948886,-161.638587796198,-161.55165773383,-161.464736785871,
-161.377767495936,-161.290769922006,-161.203680569857,-161.172381719815),
 .UNSPECIFIED.);
#271=B_SPLINE_CURVE_WITH_KNOTS('',3,(#28197,#28198,#28199,#28200,#28201,
#28202,#28203,#28204,#28205,#28206,#28207,#28208,#28209,#28210,#28211,#28212,
#28213,#28214,#28215,#28216,#28217,#28218,#28219,#28220,#28221,#28222,#28223,
#28224,#28225,#28226,#28227,#28228,#28229,#28230,#28231,#28232,#28233,#28234,
#28235,#28236,#28237,#28238,#28239,#28240,#28241,#28242,#28243,#28244,#28245,
#28246,#28247,#28248,#28249,#28250,#28251,#28252,#28253,#28254,#28255,#28256,
#28257,#28258,#28259,#28260,#28261,#28262,#28263,#28264,#28265,#28266,#28267,
#28268,#28269,#28270,#28271,#28272,#28273,#28274,#28275,#28276,#28277,#28278,
#28279,#28280,#28281,#28282,#28283,#28284,#28285,#28286,#28287,#28288,#28289,
#28290,#28291,#28292,#28293,#28294,#28295,#28296,#28297,#28298,#28299,#28300,
#28301,#28302,#28303,#28304,#28305,#28306,#28307,#28308,#28309,#28310,#28311,
#28312,#28313,#28314,#28315,#28316,#28317,#28318,#28319,#28320,#28321,#28322,
#28323,#28324,#28325,#28326,#28327,#28328,#28329,#28330,#28331,#28332,#28333,
#28334,#28335,#28336,#28337,#28338,#28339,#28340,#28341,#28342,#28343,#28344,
#28345,#28346,#28347,#28348,#28349,#28350,#28351,#28352,#28353,#28354,#28355,
#28356,#28357,#28358,#28359,#28360,#28361,#28362,#28363,#28364,#28365,#28366,
#28367,#28368,#28369,#28370,#28371,#28372,#28373,#28374,#28375,#28376,#28377,
#28378,#28379,#28380,#28381,#28382,#28383,#28384,#28385,#28386,#28387,#28388,
#28389,#28390,#28391,#28392,#28393,#28394,#28395,#28396,#28397,#28398,#28399,
#28400,#28401,#28402,#28403,#28404,#28405,#28406,#28407,#28408,#28409,#28410,
#28411,#28412,#28413,#28414,#28415,#28416,#28417,#28418,#28419,#28420,#28421,
#28422),.UNSPECIFIED.,.F.,.F.,(4,3,3,3,3,3,3,3,3,3,3,3,3,3,3,3,3,3,3,3,
3,3,3,3,3,3,3,3,3,3,3,3,3,3,3,3,3,3,3,3,3,3,3,3,3,3,3,3,3,3,3,3,3,3,3,3,
3,3,3,3,3,3,3,3,3,3,3,3,3,3,3,3,3,3,3,4),(-161.172381719684,-161.038271783866,
-160.991307988571,-160.902758424752,-160.81432366696,-160.725979907444,
-160.634152666041,-160.545911321061,-160.457683434712,-160.369447635271,
-160.281182550447,-160.192817046941,-160.104392044426,-160.015836593969,
-159.99136197622,-159.902812432459,-159.814377694878,-159.726033955703,
-159.634206706723,-159.545965382275,-159.457737516494,-159.369501737634,
-159.281236673384,-159.192871190335,-159.104446208235,-159.015890777971,
-158.991415963868,-158.902866426481,-158.814431695428,-158.726087962924,
-158.634260711498,-158.546019394041,-158.457791535358,-158.369555763696,
-158.281290706736,-158.192925231079,-158.104500256439,-158.015944833679,
-157.991469951517,-157.902920405082,-157.814485664852,-157.726141923055,
-157.634314675069,-157.546073348086,-157.457845479808,-157.369609698492,
-157.281344631827,-157.192979146439,-157.104554162041,-157.015998729559,
-156.991523939165,-156.902974396096,-156.814539659262,-156.726195920889,
-156.634368671629,-156.546127348114,-156.457899483313,-156.369663705481,
-156.281398642303,-156.193033160389,-156.104608179461,-156.016052750418,
-155.991577926814,-155.903028384309,-155.814593648058,-155.726249910282,
-155.634422660805,-155.546181337927,-155.457953473776,-155.369717696606,
-155.281452634103,-155.193087152878,-155.104662172649,-155.016106744312,
-154.991631914463,-154.889196412504),.UNSPECIFIED.);
#272=B_SPLINE_CURVE_WITH_KNOTS('',3,(#28424,#28425,#28426,#28427,#28428,
#28429,#28430,#28431,#28432,#28433),.UNSPECIFIED.,.F.,.F.,(4,1,1,1,1,1,
1,4),(-154.889187401721,-153.991685902111,-152.99173988976,-151.991793877409,
-150.991847865057,-149.991901852706,-148.991955840354,-148.606018529037),
 .UNSPECIFIED.);
#273=B_SPLINE_CURVE_WITH_KNOTS('',3,(#28435,#28436,#28437,#28438,#28439,
#28440,#28441,#28442,#28443,#28444,#28445,#28446,#28447,#28448,#28449,#28450,
#28451,#28452,#28453,#28454,#28455,#28456,#28457,#28458,#28459,#28460,#28461,
#28462,#28463,#28464,#28465,#28466,#28467,#28468,#28469,#28470,#28471,#28472,
#28473,#28474,#28475,#28476,#28477,#28478,#28479,#28480,#28481,#28482,#28483,
#28484,#28485,#28486,#28487,#28488,#28489,#28490,#28491,#28492,#28493,#28494,
#28495,#28496,#28497,#28498,#28499,#28500,#28501,#28502,#28503,#28504,#28505,
#28506,#28507,#28508,#28509,#28510,#28511,#28512,#28513,#28514,#28515,#28516,
#28517,#28518,#28519,#28520,#28521,#28522,#28523,#28524,#28525,#28526,#28527,
#28528,#28529,#28530,#28531,#28532,#28533,#28534,#28535,#28536,#28537,#28538,
#28539,#28540,#28541,#28542,#28543,#28544,#28545,#28546,#28547,#28548,#28549,
#28550,#28551,#28552,#28553,#28554,#28555,#28556,#28557,#28558,#28559,#28560,
#28561,#28562,#28563,#28564,#28565,#28566,#28567,#28568,#28569,#28570,#28571,
#28572,#28573,#28574,#28575,#28576,#28577,#28578,#28579,#28580,#28581,#28582,
#28583,#28584,#28585,#28586,#28587,#28588,#28589,#28590,#28591,#28592,#28593,
#28594,#28595,#28596,#28597,#28598,#28599,#28600,#28601,#28602,#28603,#28604,
#28605,#28606,#28607,#28608,#28609,#28610,#28611,#28612,#28613,#28614,#28615,
#28616,#28617,#28618,#28619,#28620,#28621,#28622,#28623,#28624,#28625,#28626,
#28627,#28628,#28629,#28630,#28631,#28632,#28633,#28634,#28635,#28636,#28637,
#28638,#28639,#28640,#28641,#28642,#28643,#28644,#28645,#28646,#28647,#28648,
#28649,#28650,#28651,#28652,#28653,#28654,#28655,#28656,#28657,#28658,#28659,
#28660),.UNSPECIFIED.,.F.,.F.,(4,3,3,3,3,3,3,3,3,3,3,3,3,3,3,3,3,3,3,3,
3,3,3,3,3,3,3,3,3,3,3,3,3,3,3,3,3,3,3,3,3,3,3,3,3,3,3,3,3,3,3,3,3,3,3,3,
3,3,3,3,3,3,3,3,3,3,3,3,3,3,3,3,3,3,3,4),(-148.606011105325,-148.516896311246,
-148.427765779446,-148.338599573289,-148.249313397802,-148.159965224952,
-148.070452324036,-147.992009828003,-147.903460284745,-147.815025547728,
-147.726681809176,-147.634854559986,-147.546613236307,-147.458385371348,
-147.370149593363,-147.281884530039,-147.193519047988,-147.10509406693,
-147.016538637765,-146.992063815652,-146.903514272392,-146.815079535374,
-146.72673579682,-146.63490854763,-146.546667223949,-146.458439358988,-146.370203581002,
-146.281938517676,-146.193573035624,-146.105148054564,-146.016592625397,
-145.9921178033,-145.903568260038,-145.815133523017,-145.72678978446,-145.634962535271,
-145.546721211588,-145.458493346624,-145.370257568635,-145.281992505305,
-145.19362702325,-145.105202042187,-145.016646613017,-144.992171790949,
-144.903622247689,-144.81518751067,-144.726843772116,-144.635016522926,
-144.546775199245,-144.458547334283,-144.370311556296,-144.28204649297,
-144.193681010918,-144.105256029857,-144.016700600689,-143.992225778598,
-143.903676235337,-143.815241498317,-143.726897759762,-143.635070510573,
-143.54682918689,-143.458601321928,-143.37036554394,-143.282100480614,-143.193734998561,
-143.105310017499,-143.016754588331,-142.992279766246,-142.903834207347,
-142.815500271385,-142.727256342741,-142.639080881638,-142.55094590012,
-142.462835403558,-142.374706207577,-142.322825798145),.UNSPECIFIED.);
#274=B_SPLINE_CURVE_WITH_KNOTS('',3,(#28662,#28663,#28664,#28665,#28666,
#28667,#28668,#28669,#28670,#28671),.UNSPECIFIED.,.F.,.F.,(4,1,1,1,1,1,
1,4),(-142.322818623298,-141.992333753895,-140.992387741543,-139.992441729192,
-138.992495716841,-137.992549704489,-136.992603692138,-136.039640490966),
 .UNSPECIFIED.);
#275=B_SPLINE_CURVE_WITH_KNOTS('',3,(#28673,#28674,#28675,#28676,#28677,
#28678,#28679,#28680,#28681,#28682,#28683),.UNSPECIFIED.,.F.,.F.,(4,1,1,
1,1,1,1,1,4),(-136.039640490966,-135.992657679787,-134.992711667435,-133.992765655084,
-132.992819642732,-131.992873630381,-130.99292761803,-129.992981605678,
-129.756455515395),.UNSPECIFIED.);
#276=B_SPLINE_CURVE_WITH_KNOTS('',3,(#28685,#28686,#28687,#28688,#28689,
#28690,#28691,#28692,#28693,#28694,#28695,#28696,#28697,#28698,#28699,#28700,
#28701,#28702,#28703,#28704,#28705,#28706,#28707,#28708,#28709,#28710,#28711,
#28712,#28713,#28714,#28715,#28716,#28717,#28718,#28719,#28720,#28721,#28722,
#28723,#28724,#28725,#28726,#28727,#28728,#28729,#28730,#28731,#28732,#28733,
#28734,#28735,#28736,#28737,#28738,#28739,#28740,#28741,#28742,#28743,#28744,
#28745,#28746,#28747,#28748,#28749,#28750,#28751,#28752,#28753,#28754,#28755,
#28756,#28757,#28758,#28759,#28760,#28761,#28762,#28763,#28764,#28765,#28766,
#28767,#28768,#28769,#28770,#28771,#28772,#28773,#28774,#28775,#28776,#28777,
#28778,#28779,#28780,#28781,#28782,#28783,#28784,#28785,#28786,#28787,#28788,
#28789,#28790,#28791,#28792,#28793,#28794,#28795,#28796,#28797,#28798,#28799,
#28800,#28801,#28802,#28803,#28804,#28805,#28806,#28807,#28808,#28809,#28810,
#28811,#28812,#28813,#28814,#28815,#28816,#28817,#28818,#28819,#28820,#28821,
#28822,#28823,#28824,#28825,#28826,#28827,#28828,#28829,#28830,#28831,#28832,
#28833,#28834,#28835,#28836,#28837,#28838,#28839,#28840,#28841,#28842,#28843,
#28844,#28845,#28846,#28847,#28848,#28849,#28850,#28851,#28852,#28853,#28854,
#28855,#28856,#28857,#28858,#28859,#28860,#28861,#28862,#28863,#28864,#28865,
#28866,#28867,#28868,#28869,#28870,#28871,#28872,#28873,#28874,#28875,#28876,
#28877,#28878,#28879,#28880,#28881,#28882,#28883,#28884,#28885,#28886,#28887,
#28888,#28889,#28890,#28891,#28892,#28893,#28894,#28895,#28896,#28897,#28898,
#28899,#28900,#28901,#28902,#28903,#28904,#28905,#28906,#28907,#28908,#28909,
#28910),.UNSPECIFIED.,.F.,.F.,(4,3,3,3,3,3,3,3,3,3,3,3,3,3,3,3,3,3,3,3,
3,3,3,3,3,3,3,3,3,3,3,3,3,3,3,3,3,3,3,3,3,3,3,3,3,3,3,3,3,3,3,3,3,3,3,3,
3,3,3,3,3,3,3,3,3,3,3,3,3,3,3,3,3,3,3,4),(-129.756455183786,-129.669225879151,
-129.582057726946,-129.494921170303,-129.407793834464,-129.320653356375,
-129.233423612432,-129.146147015044,-129.058730806341,-128.993035593327,
-128.904486050066,-128.816051313047,-128.727707574492,-128.635880325302,
-128.54763900162,-128.459411136659,-128.371175358671,-128.282910295343,
-128.19454481329,-128.106119832229,-128.017564403061,-127.993089580976,
-127.904540037715,-127.816105300695,-127.72776156214,-127.635934312951,
-127.547692989268,-127.459465124306,-127.371229346318,-127.28296428299,
-127.194598800937,-127.106173819875,-127.017618390707,-126.993143568624,
-126.904594025363,-126.816159288344,-126.727815549789,-126.635988300599,
-126.547746976917,-126.459519111955,-126.371283333967,-126.28301827064,
-126.194652788587,-126.106227807525,-126.017672378357,-125.993197556273,
-125.904648013013,-125.816213275993,-125.727869537438,-125.636042288249,
-125.547800964567,-125.459573099605,-125.371337321617,-125.28307225829,
-125.194706776237,-125.106281795176,-125.017726366008,-124.993251543922,
-124.904702000661,-124.816267263641,-124.727923525086,-124.636096275897,
-124.547854952214,-124.459627087252,-124.371391309264,-124.283126245937,
-124.194760763884,-124.106335782822,-124.017780353654,-123.99330553157,
-123.900984823973,-123.808821255979,-123.71685311386,-123.625000764951,
-123.533287515117,-123.473269876606),.UNSPECIFIED.);
#277=B_SPLINE_CURVE_WITH_KNOTS('',3,(#28912,#28913,#28914,#28915,#28916,
#28917,#28918,#28919,#28920,#28921),.UNSPECIFIED.,.F.,.F.,(4,1,1,1,1,1,
1,4),(-123.473268309875,-122.993359519219,-121.993413506867,-120.993467494516,
-119.993521482165,-118.993575469813,-117.993629457462,-117.19008824286),
 .UNSPECIFIED.);
#278=B_SPLINE_CURVE_WITH_KNOTS('',3,(#28923,#28924,#28925,#28926,#28927,
#28928,#28929,#28930,#28931,#28932,#28933,#28934,#28935,#28936,#28937,#28938,
#28939,#28940,#28941,#28942,#28943,#28944,#28945,#28946,#28947,#28948,#28949,
#28950,#28951,#28952,#28953,#28954,#28955,#28956,#28957,#28958,#28959,#28960,
#28961,#28962,#28963,#28964,#28965,#28966,#28967,#28968,#28969,#28970,#28971,
#28972,#28973,#28974,#28975,#28976,#28977,#28978,#28979,#28980,#28981,#28982,
#28983,#28984,#28985,#28986,#28987,#28988,#28989,#28990,#28991,#28992,#28993,
#28994,#28995,#28996,#28997,#28998,#28999,#29000,#29001,#29002,#29003,#29004,
#29005,#29006,#29007,#29008,#29009,#29010,#29011,#29012,#29013,#29014,#29015,
#29016,#29017,#29018,#29019,#29020,#29021,#29022,#29023,#29024,#29025,#29026,
#29027,#29028,#29029,#29030,#29031,#29032,#29033,#29034,#29035,#29036,#29037,
#29038,#29039,#29040,#29041,#29042,#29043,#29044,#29045,#29046,#29047,#29048,
#29049,#29050,#29051,#29052,#29053,#29054,#29055,#29056,#29057,#29058,#29059,
#29060,#29061,#29062,#29063,#29064,#29065,#29066,#29067,#29068,#29069,#29070,
#29071,#29072,#29073,#29074,#29075,#29076,#29077,#29078,#29079,#29080,#29081,
#29082,#29083,#29084,#29085,#29086,#29087,#29088,#29089,#29090,#29091,#29092,
#29093,#29094,#29095,#29096,#29097,#29098,#29099,#29100,#29101,#29102,#29103,
#29104,#29105,#29106,#29107,#29108,#29109,#29110,#29111,#29112,#29113,#29114,
#29115,#29116,#29117,#29118,#29119,#29120,#29121,#29122,#29123,#29124,#29125,
#29126,#29127,#29128,#29129,#29130,#29131,#29132,#29133,#29134,#29135,#29136,
#29137,#29138,#29139,#29140,#29141,#29142,#29143,#29144,#29145,#29146,#29147,
#29148),.UNSPECIFIED.,.F.,.F.,(4,3,3,3,3,3,3,3,3,3,3,3,3,3,3,3,3,3,3,3,
3,3,3,3,3,3,3,3,3,3,3,3,3,3,3,3,3,3,3,3,3,3,3,3,3,3,3,3,3,3,3,3,3,3,3,3,
3,3,3,3,3,3,3,3,3,3,3,3,3,3,3,3,3,3,3,4),(-117.190084569427,-117.061743136065,
-116.993683445111,-116.905133901849,-116.816699164829,-116.728355426273,
-116.636528177084,-116.548286853401,-116.460058988438,-116.371823210449,
-116.283558147121,-116.195192665067,-116.106767684005,-116.018212254836,
-115.993737432759,-115.905187889498,-115.816753152479,-115.728409413924,
-115.636582164735,-115.548340841053,-115.460112976091,-115.371877198104,
-115.283612134777,-115.195246652723,-115.106821671662,-115.018266242494,
-114.993791420408,-114.905241877147,-114.816807140127,-114.728463401572,
-114.636636152383,-114.548394828701,-114.460166963739,-114.371931185751,
-114.283666122424,-114.19530064037,-114.106875659309,-114.018320230141,
-113.993845408056,-113.905295864795,-113.816861127775,-113.72851738922,
-113.636690140031,-113.548448816348,-113.460220951386,-113.371985173398,
-113.283720110071,-113.195354628017,-113.106929646956,-113.018374217788,
-112.993899395705,-112.905349852445,-112.816915115425,-112.72857137687,
-112.636744127681,-112.548502803999,-112.460274939037,-112.37203916105,
-112.283774097722,-112.195408615669,-112.106983634608,-112.018428205441,
-111.993953383354,-111.905403840093,-111.816969103073,-111.728625364518,
-111.636798115329,-111.548556791647,-111.460328926684,-111.372093148696,
-111.283828085369,-111.195462603316,-111.107037622254,-111.018482193086,
-110.994007371002,-110.906899262247),.UNSPECIFIED.);
#279=B_SPLINE_CURVE_WITH_KNOTS('',3,(#29150,#29151,#29152,#29153,#29154,
#29155,#29156,#29157,#29158,#29159),.UNSPECIFIED.,.F.,.F.,(4,1,1,1,1,1,
1,4),(-110.906890495548,-109.994061358651,-108.9941153463,-107.994169333948,
-106.994223321597,-105.994277309245,-104.994331296894,-104.623721628154),
 .UNSPECIFIED.);
#280=B_SPLINE_CURVE_WITH_KNOTS('',3,(#29161,#29162,#29163,#29164,#29165,
#29166,#29167,#29168,#29169,#29170,#29171,#29172,#29173,#29174,#29175,#29176,
#29177,#29178,#29179,#29180,#29181,#29182,#29183,#29184,#29185,#29186,#29187,
#29188,#29189,#29190,#29191,#29192,#29193,#29194,#29195,#29196,#29197,#29198,
#29199,#29200,#29201,#29202,#29203,#29204,#29205,#29206,#29207,#29208,#29209,
#29210,#29211,#29212,#29213,#29214,#29215,#29216,#29217,#29218,#29219,#29220,
#29221,#29222,#29223,#29224,#29225,#29226,#29227,#29228,#29229,#29230,#29231,
#29232,#29233,#29234,#29235,#29236,#29237,#29238,#29239,#29240,#29241,#29242,
#29243,#29244,#29245,#29246,#29247,#29248,#29249,#29250,#29251,#29252,#29253,
#29254,#29255,#29256,#29257,#29258,#29259,#29260,#29261,#29262,#29263,#29264,
#29265,#29266,#29267,#29268,#29269,#29270,#29271,#29272,#29273,#29274,#29275,
#29276,#29277,#29278,#29279,#29280,#29281,#29282,#29283,#29284,#29285,#29286,
#29287,#29288,#29289,#29290,#29291,#29292,#29293,#29294,#29295,#29296,#29297,
#29298,#29299,#29300,#29301,#29302,#29303,#29304,#29305,#29306,#29307,#29308,
#29309,#29310,#29311,#29312,#29313,#29314,#29315,#29316,#29317,#29318,#29319,
#29320,#29321,#29322,#29323,#29324,#29325,#29326,#29327,#29328,#29329,#29330,
#29331,#29332,#29333,#29334,#29335,#29336,#29337,#29338,#29339,#29340,#29341,
#29342,#29343,#29344,#29345,#29346,#29347,#29348,#29349,#29350,#29351,#29352,
#29353,#29354,#29355,#29356,#29357,#29358,#29359,#29360,#29361,#29362,#29363,
#29364,#29365,#29366,#29367,#29368,#29369,#29370,#29371,#29372,#29373,#29374,
#29375,#29376,#29377,#29378,#29379,#29380,#29381,#29382,#29383,#29384,#29385,
#29386),.UNSPECIFIED.,.F.,.F.,(4,3,3,3,3,3,3,3,3,3,3,3,3,3,3,3,3,3,3,3,
3,3,3,3,3,3,3,3,3,3,3,3,3,3,3,3,3,3,3,3,3,3,3,3,3,3,3,3,3,3,3,3,3,3,3,3,
3,3,3,3,3,3,3,3,3,3,3,3,3,3,3,3,3,3,3,4),(-104.623713955068,-104.534906093999,
-104.446092177846,-104.357251749749,-104.266535133448,-104.177526827267,
-104.085956055905,-103.994385284543,-103.905835741282,-103.817401004262,
-103.729057265707,-103.637230016517,-103.548988692835,-103.460760827873,
-103.372525049885,-103.284259986557,-103.195894504504,-103.107469523442,
-103.018914094274,-102.994439272191,-102.90588972893,-102.817454991911,
-102.729111253356,-102.637284004166,-102.549042680484,-102.460814815522,
-102.372579037534,-102.284313974207,-102.195948492154,-102.107523511093,
-102.018968081925,-101.99449325984,-101.905943716579,-101.81750897956,-101.729165241005,
-101.637337991815,-101.549096668134,-101.460868803172,-101.372633025184,
-101.284367961857,-101.196002479804,-101.107577498743,-101.019022069575,
-100.994547247489,-100.905997704228,-100.817562967208,-100.729219228653,
-100.637391979464,-100.549150655781,-100.460922790819,-100.372687012831,
-100.284421949504,-100.19605646745,-100.107631486389,-100.019076057221,
-99.9946012351372,-99.9060516918764,-99.8176169548564,-99.7292732163011,
-99.6374459671117,-99.5492046434295,-99.4609767784672,-99.3727410004794,
-99.2844759371525,-99.1961104550991,-99.107685474038,-99.0191300448696,
-98.9946552227858,-98.905949860575,-98.8173584473077,-98.7288596647749,
-98.6404322712687,-98.5520521175381,-98.4636992979816,-98.3753378753946,
-98.3405286478881),.UNSPECIFIED.);
#281=B_SPLINE_CURVE_WITH_KNOTS('',3,(#29388,#29389,#29390,#29391,#29392,
#29393,#29394,#29395,#29396,#29397,#29398,#29399,#29400,#29401,#29402,#29403,
#29404,#29405,#29406,#29407,#29408,#29409,#29410,#29411,#29412,#29413,#29414,
#29415,#29416,#29417,#29418,#29419,#29420,#29421,#29422,#29423,#29424,#29425,
#29426,#29427,#29428,#29429,#29430,#29431,#29432,#29433,#29434,#29435,#29436,
#29437,#29438,#29439,#29440,#29441,#29442,#29443,#29444,#29445,#29446,#29447,
#29448,#29449,#29450,#29451,#29452,#29453,#29454,#29455,#29456,#29457,#29458,
#29459,#29460,#29461,#29462,#29463,#29464,#29465,#29466,#29467,#29468,#29469,
#29470,#29471,#29472,#29473,#29474,#29475,#29476,#29477,#29478,#29479,#29480,
#29481,#29482,#29483,#29484,#29485,#29486,#29487,#29488,#29489,#29490,#29491,
#29492,#29493,#29494,#29495,#29496,#29497,#29498,#29499,#29500,#29501,#29502,
#29503,#29504,#29505,#29506,#29507,#29508,#29509,#29510,#29511,#29512,#29513,
#29514,#29515,#29516,#29517,#29518,#29519,#29520,#29521,#29522,#29523,#29524,
#29525,#29526,#29527,#29528,#29529,#29530,#29531,#29532,#29533,#29534,#29535,
#29536,#29537,#29538,#29539,#29540,#29541,#29542,#29543,#29544,#29545,#29546,
#29547,#29548,#29549,#29550,#29551,#29552,#29553,#29554,#29555,#29556,#29557,
#29558,#29559,#29560,#29561,#29562,#29563,#29564,#29565,#29566,#29567,#29568,
#29569,#29570,#29571,#29572,#29573,#29574,#29575,#29576,#29577,#29578,#29579,
#29580,#29581,#29582,#29583,#29584,#29585,#29586,#29587,#29588,#29589,#29590,
#29591,#29592,#29593,#29594,#29595,#29596,#29597,#29598,#29599,#29600,#29601,
#29602,#29603,#29604,#29605,#29606,#29607,#29608,#29609,#29610,#29611,#29612,
#29613),.UNSPECIFIED.,.F.,.F.,(4,3,3,3,3,3,3,3,3,3,3,3,3,3,3,3,3,3,3,3,
3,3,3,3,3,3,3,3,3,3,3,3,3,3,3,3,3,3,3,3,3,3,3,3,3,3,3,3,3,3,3,3,3,3,3,3,
3,3,3,3,3,3,3,3,3,3,3,3,3,3,3,3,3,3,3,4),(-98.3405286476581,-98.2388278601938,
-98.1365688139642,-98.0336484171347,-97.9947092104345,-97.9061596671738,
-97.8177249301541,-97.7293811915989,-97.6375539424094,-97.5493126187274,
-97.4610847537654,-97.3728489757775,-97.2845839124504,-97.1962184303971,
-97.1077934493357,-97.0192380201675,-96.9947631980831,-96.9062136548223,
-96.8177789178026,-96.7294351792475,-96.637607930058,-96.549366606376,-96.4611387414139,
-96.3729029634261,-96.2846379000986,-96.1962724180453,-96.107847436984,
-96.0192920078157,-95.9948171857317,-95.906267642471,-95.8178329054513,
-95.7294891668962,-95.6376619177068,-95.5494205940248,-95.4611927290627,
-95.372956951075,-95.2846918877477,-95.1963264056944,-95.1079014246331,
-95.0193459954649,-94.9948711733804,-94.9063216301196,-94.8178868930999,
-94.7295431545448,-94.6377159053554,-94.5494745816733,-94.4612467167113,
-94.3730109387235,-94.2847458753962,-94.1963803933429,-94.1079554122816,
-94.0193999831134,-93.994925161029,-93.9063756177682,-93.8179408807485,
-93.7295971421934,-93.6377698930039,-93.5495285693218,-93.4613007043598,
-93.3730649263719,-93.2847998630446,-93.1964343809913,-93.10800939993,-93.0194539707618,
-92.9949791486776,-92.9072355423437,-92.8196060648545,-92.732066048324,
-92.6445893384008,-92.5571455235984,-92.4697124608468,-92.3822680202302,
-92.2947386999218,-92.207164380361,-92.1194565324101,-92.0573433407085),
 .UNSPECIFIED.);
#282=B_SPLINE_CURVE_WITH_KNOTS('',3,(#29615,#29616,#29617,#29618,#29619,
#29620,#29621,#29622,#29623,#29624,#29625),.UNSPECIFIED.,.F.,.F.,(4,1,1,
1,1,1,1,1,4),(-92.0573433407085,-91.9950331363262,-90.9950871239749,-89.9951411116235,
-88.9951950992721,-87.9952490869208,-86.9953030745694,-85.995357062218,
-85.7741580335289),.UNSPECIFIED.);
#283=B_SPLINE_CURVE_WITH_KNOTS('',3,(#29627,#29628,#29629,#29630,#29631,
#29632,#29633,#29634,#29635,#29636,#29637,#29638,#29639,#29640,#29641,#29642,
#29643,#29644,#29645,#29646,#29647,#29648,#29649,#29650,#29651,#29652,#29653,
#29654,#29655,#29656,#29657,#29658,#29659,#29660,#29661,#29662,#29663,#29664,
#29665,#29666,#29667,#29668,#29669,#29670,#29671,#29672,#29673,#29674,#29675,
#29676,#29677,#29678,#29679,#29680,#29681,#29682,#29683,#29684,#29685,#29686,
#29687,#29688,#29689,#29690,#29691,#29692,#29693,#29694,#29695,#29696,#29697,
#29698,#29699,#29700,#29701,#29702,#29703,#29704,#29705,#29706,#29707,#29708,
#29709,#29710,#29711,#29712,#29713,#29714,#29715,#29716,#29717,#29718,#29719,
#29720,#29721,#29722,#29723,#29724,#29725,#29726,#29727,#29728,#29729,#29730,
#29731,#29732,#29733,#29734,#29735,#29736,#29737,#29738,#29739,#29740,#29741,
#29742,#29743,#29744,#29745,#29746,#29747,#29748,#29749,#29750,#29751,#29752,
#29753,#29754,#29755,#29756,#29757,#29758,#29759,#29760,#29761,#29762,#29763,
#29764,#29765,#29766,#29767,#29768,#29769,#29770,#29771,#29772,#29773,#29774,
#29775,#29776,#29777,#29778,#29779,#29780,#29781,#29782,#29783,#29784,#29785,
#29786,#29787,#29788,#29789,#29790,#29791,#29792,#29793,#29794,#29795,#29796,
#29797,#29798,#29799,#29800,#29801,#29802,#29803,#29804,#29805,#29806,#29807,
#29808,#29809,#29810,#29811,#29812,#29813,#29814,#29815,#29816,#29817,#29818,
#29819,#29820,#29821,#29822,#29823,#29824,#29825,#29826,#29827,#29828,#29829,
#29830,#29831,#29832,#29833,#29834,#29835,#29836,#29837,#29838,#29839,#29840,
#29841,#29842,#29843,#29844,#29845,#29846,#29847,#29848,#29849,#29850,#29851,
#29852),.UNSPECIFIED.,.F.,.F.,(4,3,3,3,3,3,3,3,3,3,3,3,3,3,3,3,3,3,3,3,
3,3,3,3,3,3,3,3,3,3,3,3,3,3,3,3,3,3,3,3,3,3,3,3,3,3,3,3,3,3,3,3,3,3,3,3,
3,3,3,3,3,3,3,3,3,3,3,3,3,3,3,3,3,3,3,4),(-85.7741580335289,-85.6869940390936,
-85.5998987318649,-85.5128399462755,-85.4257952412113,-85.3387421916226,
-85.2516030644243,-85.1644212737914,-85.0770957414917,-84.9954110498666,
-84.9068615066059,-84.8184267695863,-84.7300830310311,-84.6382557818416,
-84.5500144581596,-84.4617865931975,-84.3735508152097,-84.2852857518826,
-84.1969202698293,-84.1084952887679,-84.0199398595997,-83.9954650375153,
-83.9069154942545,-83.8184807572348,-83.7301370186797,-83.6383097694902,
-83.5500684458081,-83.4618405808461,-83.3736048028584,-83.2853397395314,
-83.196974257478,-83.1085492764167,-83.0199938472485,-82.9955190251639,
-82.9069694819031,-82.8185347448832,-82.7301910063281,-82.6383637571386,
-82.5501224334565,-82.4618945684944,-82.3736587905064,-82.2853937271789,
-82.1970282451255,-82.1086032640641,-82.0200478348961,-81.9955730128125,
-81.9070234695518,-81.8185887325322,-81.730244993977,-81.6384177447876,
-81.5501764211055,-81.4619485561435,-81.3737127781559,-81.2854477148285,
-81.1970822327752,-81.1086572517138,-81.0201018225456,-80.9956270004612,
-80.9070774572005,-80.8186427201807,-80.7302989816257,-80.6384717324362,
-80.5502304087541,-80.462002543792,-80.3737667658043,-80.2855017024774,
-80.197136220424,-80.1087112393627,-80.0201558101946,-79.9956809881098,
-79.9027596067704,-79.8100048180451,-79.717462914801,-79.6250490832349,
-79.5327942325015,-79.4909727263493),.UNSPECIFIED.);
#284=B_SPLINE_CURVE_WITH_KNOTS('',3,(#29854,#29855,#29856,#29857,#29858,
#29859,#29860,#29861,#29862,#29863,#29864,#29865,#29866,#29867,#29868,#29869,
#29870,#29871,#29872,#29873,#29874,#29875,#29876,#29877,#29878,#29879,#29880,
#29881,#29882,#29883,#29884,#29885,#29886,#29887,#29888,#29889,#29890,#29891,
#29892,#29893,#29894,#29895,#29896,#29897,#29898,#29899,#29900,#29901,#29902,
#29903,#29904,#29905,#29906,#29907,#29908,#29909,#29910,#29911,#29912,#29913,
#29914,#29915,#29916,#29917,#29918,#29919,#29920,#29921,#29922,#29923,#29924,
#29925,#29926,#29927,#29928,#29929,#29930,#29931,#29932,#29933,#29934,#29935,
#29936,#29937,#29938,#29939,#29940,#29941,#29942,#29943,#29944,#29945,#29946,
#29947,#29948,#29949,#29950,#29951,#29952,#29953,#29954,#29955,#29956,#29957,
#29958,#29959,#29960,#29961,#29962,#29963,#29964,#29965,#29966,#29967,#29968,
#29969,#29970,#29971,#29972,#29973,#29974,#29975,#29976,#29977,#29978,#29979,
#29980,#29981,#29982,#29983,#29984,#29985,#29986,#29987,#29988,#29989,#29990,
#29991,#29992,#29993,#29994,#29995,#29996,#29997,#29998,#29999,#30000,#30001,
#30002,#30003,#30004,#30005,#30006,#30007,#30008,#30009,#30010,#30011,#30012,
#30013,#30014,#30015,#30016,#30017,#30018,#30019,#30020,#30021,#30022,#30023,
#30024,#30025,#30026,#30027,#30028,#30029,#30030,#30031,#30032,#30033,#30034,
#30035,#30036,#30037,#30038,#30039,#30040,#30041,#30042,#30043,#30044,#30045,
#30046,#30047,#30048,#30049,#30050,#30051,#30052,#30053,#30054,#30055,#30056,
#30057,#30058,#30059,#30060,#30061,#30062,#30063,#30064,#30065,#30066,#30067,
#30068,#30069,#30070,#30071,#30072,#30073,#30074,#30075,#30076,#30077,#30078,
#30079),.UNSPECIFIED.,.F.,.F.,(4,3,3,3,3,3,3,3,3,3,3,3,3,3,3,3,3,3,3,3,
3,3,3,3,3,3,3,3,3,3,3,3,3,3,3,3,3,3,3,3,3,3,3,3,3,3,3,3,3,3,3,3,3,3,3,3,
3,3,3,3,3,3,3,3,3,3,3,3,3,3,3,3,3,3,3,4),(-79.4909727261433,-79.3983623352896,
-79.3056157212193,-79.2126378190239,-79.1195318864591,-79.0262153902688,
-78.9957349757584,-78.9071854324977,-78.8187506954779,-78.7304069569228,
-78.6385797077333,-78.5503383840513,-78.4621105190892,-78.3738747411014,
-78.285609677774,-78.1972441957207,-78.1088192146593,-78.0202637854911,
-77.995788963407,-77.9072394201463,-77.8188046831266,-77.7304609445716,
-77.6386336953821,-77.5503923717001,-77.462164506738,-77.3739287287503,
-77.285663665423,-77.1972981833697,-77.1088732023084,-77.0203177731402,
-76.9958429510557,-76.907293407795,-76.8188586707753,-76.7305149322202,
-76.6386876830307,-76.5504463593487,-76.4622184943866,-76.3739827163988,
-76.2857176530715,-76.1973521710181,-76.1089271899568,-76.0203717607886,
-75.9958969387043,-75.9073473954435,-75.8189126584238,-75.7305689198687,
-75.6387416706792,-75.5505003469971,-75.4622724820351,-75.3740367040473,
-75.28577164072,-75.1974061586667,-75.1089811776053,-75.0204257484371,-74.9959509263529,
-74.9074013830922,-74.8189666460725,-74.7306229075175,-74.638795658328,
-74.550554334646,-74.462326469684,-74.3740906916963,-74.285825628369,-74.1974601463157,
-74.1090351652543,-74.0204797360861,-73.9960049140016,-73.9086913845972,
-73.8210783889188,-73.7339828174008,-73.6469435929607,-73.5599382140351,
-73.4719005153187,-73.3848666078328,-73.2963270135013,-73.2077874191697),
 .UNSPECIFIED.);
#285=B_SPLINE_CURVE_WITH_KNOTS('',3,(#30081,#30082,#30083,#30084,#30085,
#30086,#30087,#30088,#30089,#30090,#30091),.UNSPECIFIED.,.F.,.F.,(4,1,1,
1,1,1,1,1,4),(-73.2077874191697,-72.9960589016502,-71.9961128892988,-70.9961668769474,
-69.9962208645961,-68.9962748522447,-67.9963288398933,-66.9963828275419,
-66.9246021119901),.UNSPECIFIED.);
#286=B_SPLINE_CURVE_WITH_KNOTS('',3,(#30093,#30094,#30095,#30096,#30097,
#30098,#30099,#30100,#30101,#30102,#30103,#30104,#30105,#30106,#30107,#30108,
#30109,#30110,#30111,#30112,#30113,#30114,#30115,#30116,#30117,#30118,#30119,
#30120,#30121,#30122,#30123,#30124,#30125,#30126,#30127,#30128,#30129,#30130,
#30131,#30132,#30133,#30134,#30135,#30136,#30137,#30138,#30139,#30140,#30141,
#30142,#30143,#30144,#30145,#30146,#30147,#30148,#30149,#30150,#30151,#30152,
#30153,#30154,#30155,#30156,#30157,#30158,#30159,#30160,#30161,#30162,#30163,
#30164,#30165,#30166,#30167,#30168,#30169,#30170,#30171,#30172,#30173,#30174,
#30175,#30176,#30177,#30178,#30179,#30180,#30181,#30182,#30183,#30184,#30185,
#30186,#30187,#30188,#30189,#30190,#30191,#30192,#30193,#30194,#30195,#30196,
#30197,#30198,#30199,#30200,#30201,#30202,#30203,#30204,#30205,#30206,#30207,
#30208,#30209,#30210,#30211,#30212,#30213,#30214,#30215,#30216,#30217,#30218,
#30219,#30220,#30221,#30222,#30223,#30224,#30225,#30226,#30227,#30228,#30229,
#30230,#30231,#30232,#30233,#30234,#30235,#30236,#30237,#30238,#30239,#30240,
#30241,#30242,#30243,#30244,#30245,#30246,#30247,#30248,#30249,#30250,#30251,
#30252,#30253,#30254,#30255,#30256,#30257,#30258,#30259,#30260,#30261,#30262,
#30263,#30264,#30265,#30266,#30267,#30268,#30269,#30270,#30271,#30272,#30273,
#30274,#30275,#30276,#30277,#30278,#30279,#30280,#30281,#30282,#30283,#30284,
#30285,#30286,#30287,#30288,#30289,#30290,#30291,#30292,#30293,#30294,#30295,
#30296,#30297,#30298,#30299,#30300,#30301,#30302,#30303,#30304,#30305,#30306,
#30307,#30308,#30309,#30310,#30311,#30312,#30313,#30314,#30315,#30316,#30317,
#30318),.UNSPECIFIED.,.F.,.F.,(4,3,3,3,3,3,3,3,3,3,3,3,3,3,3,3,3,3,3,3,
3,3,3,3,3,3,3,3,3,3,3,3,3,3,3,3,3,3,3,3,3,3,3,3,3,3,3,3,3,3,3,3,3,3,3,3,
3,3,3,3,3,3,3,3,3,3,3,3,3,3,3,3,3,3,3,4),(-66.9246021119901,-66.8369765253447,
-66.7494590597405,-66.6620249933431,-66.5746452757939,-66.4872927329728,
-66.3999451562261,-66.312580345127,-66.225123600006,-66.1376166205138,-66.0499731462281,
-65.9964368151906,-65.9078872719299,-65.8194525349102,-65.731108796355,
-65.6392815471655,-65.5510402234834,-65.4628123585214,-65.3745765805337,
-65.2863115172062,-65.1979460351529,-65.1095210540915,-65.0209656249233,
-64.9964908028392,-64.9079412595785,-64.8195065225587,-64.7311627840035,
-64.6393355348141,-64.5510942111319,-64.4628663461699,-64.3746305681822,
-64.2863655048552,-64.1980000228018,-64.1095750417404,-64.0210196125721,
-63.9965447904878,-63.907995247227,-63.8195605102072,-63.7312167716523,
-63.6393895224628,-63.5511481987807,-63.4629203338186,-63.3746845558308,
-63.2864194925035,-63.1980540104502,-63.1096290293892,-63.021073600221,
-62.9965987781364,-62.9080492348756,-62.819614497856,-62.7312707593011,
-62.6394435101116,-62.5512021864295,-62.4629743214675,-62.3747385434799,
-62.2864734801525,-62.1981079980991,-62.1096830170379,-62.0211275878698,
-61.9966527657851,-61.9081032225242,-61.8196684855045,-61.731324746949,
-61.6394974977596,-61.5512561740775,-61.4630283091153,-61.3747925311274,
-61.2865274678006,-61.1981619857472,-61.1097370046858,-61.0211815755178,
-60.9967067534337,-60.8947512781198,-60.7932032283243,-60.6923996642118,
-60.6414170517604),.UNSPECIFIED.);
#287=B_SPLINE_CURVE_WITH_KNOTS('',3,(#30320,#30321,#30322,#30323,#30324,
#30325,#30326,#30327,#30328,#30329),.UNSPECIFIED.,.F.,.F.,(4,1,1,1,1,1,
1,4),(-60.6414168048105,-59.9967607410823,-58.996814728731,-57.9968687163796,
-56.9969227040282,-55.9969766916768,-54.9970306793255,-54.3582314976309),
 .UNSPECIFIED.);
#288=B_SPLINE_CURVE_WITH_KNOTS('',3,(#30331,#30332,#30333,#30334,#30335,
#30336,#30337,#30338,#30339,#30340),.UNSPECIFIED.,.F.,.F.,(4,1,1,1,1,1,
1,4),(-54.3582314976309,-53.9970846669741,-52.9971386546227,-51.9971926422714,
-50.99724662992,-49.9973006175686,-48.9973546052172,-48.0750546059844),
 .UNSPECIFIED.);
#289=B_SPLINE_CURVE_WITH_KNOTS('',3,(#30342,#30343,#30344,#30345,#30346,
#30347,#30348,#30349,#30350,#30351,#30352,#30353,#30354,#30355,#30356,#30357,
#30358,#30359,#30360,#30361,#30362,#30363,#30364,#30365,#30366,#30367,#30368,
#30369,#30370,#30371,#30372,#30373,#30374,#30375,#30376,#30377,#30378,#30379,
#30380,#30381,#30382,#30383,#30384,#30385,#30386,#30387,#30388,#30389,#30390,
#30391,#30392,#30393,#30394,#30395,#30396,#30397,#30398,#30399,#30400,#30401,
#30402,#30403,#30404,#30405,#30406,#30407,#30408,#30409,#30410,#30411,#30412,
#30413,#30414,#30415,#30416,#30417,#30418,#30419,#30420,#30421,#30422,#30423,
#30424,#30425,#30426,#30427,#30428,#30429,#30430,#30431,#30432,#30433,#30434,
#30435,#30436,#30437,#30438,#30439,#30440,#30441,#30442,#30443,#30444,#30445,
#30446,#30447,#30448,#30449,#30450,#30451,#30452,#30453,#30454,#30455,#30456,
#30457,#30458,#30459,#30460,#30461,#30462,#30463,#30464,#30465,#30466,#30467,
#30468,#30469,#30470,#30471,#30472,#30473,#30474,#30475,#30476,#30477,#30478,
#30479,#30480,#30481,#30482,#30483,#30484,#30485,#30486,#30487,#30488,#30489,
#30490,#30491,#30492,#30493,#30494,#30495,#30496,#30497,#30498,#30499,#30500,
#30501,#30502,#30503,#30504,#30505,#30506,#30507,#30508,#30509,#30510,#30511,
#30512,#30513,#30514,#30515,#30516,#30517,#30518,#30519,#30520,#30521,#30522,
#30523,#30524,#30525,#30526,#30527,#30528,#30529,#30530,#30531,#30532,#30533,
#30534,#30535,#30536,#30537,#30538,#30539,#30540,#30541,#30542,#30543,#30544,
#30545,#30546,#30547,#30548,#30549,#30550,#30551,#30552,#30553,#30554,#30555,
#30556,#30557,#30558,#30559,#30560,#30561,#30562,#30563,#30564,#30565,#30566,
#30567),.UNSPECIFIED.,.F.,.F.,(4,3,3,3,3,3,3,3,3,3,3,3,3,3,3,3,3,3,3,3,
3,3,3,3,3,3,3,3,3,3,3,3,3,3,3,3,3,3,3,3,3,3,3,3,3,3,3,3,3,3,3,3,3,3,3,3,
3,3,3,3,3,3,3,3,3,3,3,3,3,3,3,3,3,3,3,4),(-48.0750461904513,-47.9974085928659,
-47.9088590496049,-47.820424312585,-47.7320805740297,-47.6402533248403,
-47.552012001158,-47.4637841361958,-47.3755483582077,-47.2872832948801,
-47.1989178128266,-47.1104928317649,-47.0219374025965,-46.9974625805145,
-46.9089130372538,-46.8204783002341,-46.732134561679,-46.6403073124895,
-46.5520659888075,-46.4638381238455,-46.3756023458578,-46.2873372825305,
-46.1989718004772,-46.1105468194159,-46.0219913902478,-45.9975165681631,
-45.9089670249024,-45.8205322878828,-45.7321885493277,-45.6403613001382,
-45.5521199764563,-45.4638921114943,-45.3756563335065,-45.2873912701792,
-45.1990257881259,-45.1106008070647,-45.0220453778966,-44.9975705558118,
-44.909021012551,-44.8205862755313,-44.7322425369762,-44.6404152877867,
-44.5521739641047,-44.4639460991426,-44.3757103211548,-44.2874452578275,
-44.1990797757741,-44.1106547947128,-44.0220993655446,-43.9976245434604,
-43.9090750001997,-43.82064026318,-43.7322965246249,-43.6404692754354,-43.5522279517533,
-43.4640000867913,-43.3757643088036,-43.2874992454762,-43.1991337634229,
-43.1107087823616,-43.0221533531934,-42.997678531109,-42.9091289878483,
-42.8206942508286,-42.7323505122735,-42.6405232630841,-42.552281939402,
-42.46405407444,-42.3758182964522,-42.287553233125,-42.1991877510717,-42.1107627700105,
-42.0222073408422,-41.9977325187576,-41.8724138615788,-41.7918608832717),
 .UNSPECIFIED.);
#290=B_SPLINE_CURVE_WITH_KNOTS('',3,(#30569,#30570,#30571,#30572,#30573,
#30574,#30575,#30576,#30577,#30578,#30579,#30580,#30581,#30582,#30583,#30584,
#30585,#30586,#30587,#30588,#30589,#30590,#30591,#30592,#30593,#30594,#30595,
#30596,#30597,#30598,#30599,#30600,#30601,#30602,#30603,#30604,#30605,#30606,
#30607,#30608,#30609,#30610,#30611,#30612,#30613,#30614,#30615,#30616,#30617,
#30618,#30619,#30620,#30621,#30622,#30623,#30624,#30625,#30626,#30627,#30628,
#30629,#30630,#30631,#30632,#30633,#30634,#30635,#30636,#30637,#30638,#30639,
#30640,#30641,#30642,#30643,#30644,#30645,#30646,#30647,#30648,#30649,#30650,
#30651,#30652,#30653,#30654,#30655,#30656,#30657,#30658,#30659,#30660,#30661,
#30662,#30663,#30664,#30665,#30666,#30667,#30668,#30669,#30670,#30671,#30672,
#30673,#30674,#30675,#30676,#30677,#30678,#30679,#30680,#30681,#30682,#30683,
#30684,#30685,#30686,#30687,#30688,#30689,#30690,#30691,#30692,#30693,#30694,
#30695,#30696,#30697,#30698,#30699,#30700,#30701,#30702,#30703,#30704,#30705,
#30706,#30707,#30708,#30709,#30710,#30711,#30712,#30713,#30714,#30715,#30716,
#30717,#30718,#30719,#30720,#30721,#30722,#30723,#30724,#30725,#30726,#30727,
#30728,#30729,#30730,#30731,#30732,#30733,#30734,#30735,#30736,#30737,#30738,
#30739,#30740,#30741,#30742,#30743,#30744,#30745,#30746,#30747,#30748,#30749,
#30750,#30751,#30752,#30753,#30754,#30755,#30756,#30757,#30758,#30759,#30760,
#30761,#30762,#30763,#30764,#30765,#30766,#30767,#30768,#30769,#30770,#30771,
#30772,#30773,#30774,#30775,#30776,#30777,#30778,#30779,#30780,#30781,#30782,
#30783,#30784,#30785,#30786,#30787,#30788,#30789,#30790,#30791,#30792,#30793,
#30794),.UNSPECIFIED.,.F.,.F.,(4,3,3,3,3,3,3,3,3,3,3,3,3,3,3,3,3,3,3,3,
3,3,3,3,3,3,3,3,3,3,3,3,3,3,3,3,3,3,3,3,3,3,3,3,3,3,3,3,3,3,3,3,3,3,3,3,
3,3,3,3,3,3,3,3,3,3,3,3,3,3,3,3,3,3,3,4),(-41.7918608831318,-41.7047406880879,
-41.6163714153777,-41.5293687538345,-41.442384448814,-41.3553960300837,
-41.2659936491644,-41.1788817051822,-41.0883341057943,-40.9977865064063,
-40.9092369631456,-40.8208022261259,-40.732458487571,-40.6406312383815,
-40.5523899146994,-40.4641620497374,-40.3759262717495,-40.2876612084222,
-40.1992957263689,-40.1108707453076,-40.0223153161394,-39.9978404940549,
-39.9092909507942,-39.8208562137744,-39.7325124752191,-39.6406852260297,
-39.5524439023476,-39.4642160373855,-39.3759802593978,-39.2877151960708,
-39.1993497140176,-39.1109247329563,-39.0223693037881,-38.9978944817035,
-38.9093449384427,-38.8209102014229,-38.7325664628676,-38.6407392136782,
-38.5524978899962,-38.4642700250342,-38.3760342470463,-38.2877691837193,
-38.1994037016659,-38.1109787206049,-38.0224232914369,-37.9979484693521,
-37.9093989260914,-37.8209641890717,-37.7326204505165,-37.6407932013271,
-37.552551877645,-37.4643240126829,-37.3760882346953,-37.2878231713679,
-37.1994576893146,-37.1110327082532,-37.022477279085,-36.9980024570008,
-36.9094529137401,-36.8210181767205,-36.7326744381654,-36.6408471889759,
-36.5526058652939,-36.464378000332,-36.3761422223444,-36.2878771590168,
-36.1995116769635,-36.1110866959022,-36.0225312667339,-35.9980564446494,
-35.9044859724487,-35.8110931478129,-35.717933086428,-35.6249158515222,
-35.5320788066918,-35.5086755763231),.UNSPECIFIED.);
#291=B_SPLINE_CURVE_WITH_KNOTS('',3,(#30796,#30797,#30798,#30799,#30800,
#30801,#30802,#30803,#30804,#30805,#30806,#30807,#30808,#30809,#30810,#30811,
#30812,#30813,#30814,#30815,#30816,#30817,#30818,#30819,#30820,#30821,#30822,
#30823,#30824,#30825,#30826,#30827,#30828,#30829,#30830,#30831,#30832,#30833,
#30834,#30835,#30836,#30837,#30838,#30839,#30840,#30841,#30842,#30843,#30844,
#30845,#30846,#30847,#30848,#30849,#30850,#30851,#30852,#30853,#30854,#30855,
#30856,#30857,#30858,#30859,#30860,#30861,#30862,#30863,#30864,#30865,#30866,
#30867,#30868,#30869,#30870,#30871,#30872,#30873,#30874,#30875,#30876,#30877,
#30878,#30879,#30880,#30881,#30882,#30883,#30884,#30885,#30886,#30887,#30888,
#30889,#30890,#30891,#30892,#30893,#30894,#30895,#30896,#30897,#30898,#30899,
#30900,#30901,#30902,#30903,#30904,#30905,#30906,#30907,#30908,#30909,#30910,
#30911,#30912,#30913,#30914,#30915,#30916,#30917,#30918,#30919,#30920,#30921,
#30922,#30923,#30924,#30925,#30926,#30927,#30928,#30929,#30930,#30931,#30932,
#30933,#30934,#30935,#30936,#30937,#30938,#30939,#30940,#30941,#30942,#30943,
#30944,#30945,#30946,#30947,#30948,#30949,#30950,#30951,#30952,#30953,#30954,
#30955,#30956,#30957,#30958,#30959,#30960,#30961,#30962,#30963,#30964,#30965,
#30966,#30967,#30968,#30969,#30970,#30971,#30972,#30973,#30974,#30975,#30976,
#30977,#30978,#30979,#30980,#30981,#30982,#30983,#30984,#30985,#30986,#30987,
#30988,#30989,#30990,#30991,#30992,#30993,#30994,#30995,#30996,#30997,#30998,
#30999,#31000,#31001,#31002,#31003,#31004,#31005,#31006,#31007,#31008,#31009,
#31010,#31011,#31012,#31013,#31014,#31015,#31016,#31017,#31018,#31019,#31020,
#31021),.UNSPECIFIED.,.F.,.F.,(4,3,3,3,3,3,3,3,3,3,3,3,3,3,3,3,3,3,3,3,
3,3,3,3,3,3,3,3,3,3,3,3,3,3,3,3,3,3,3,3,3,3,3,3,3,3,3,3,3,3,3,3,3,3,3,3,
3,3,3,3,3,3,3,3,3,3,3,3,3,3,3,3,3,3,3,4),(-35.5086755760921,-35.4166443511499,
-35.3244992203645,-35.2321443196328,-35.1396757545066,-35.0470006032941,
-34.998110432298,-34.9095608890373,-34.8211261520178,-34.7327824134629,
-34.6409551642734,-34.5527138405915,-34.4644859756297,-34.3762501976422,
-34.2879851343154,-34.1996196522622,-34.111194671201,-34.022639242033,-33.9981644199467,
-33.9096148766864,-33.8211801396674,-33.7328364011129,-33.6410091519232,
-33.5527678282416,-33.4645399632801,-33.3763041852927,-33.2880391219658,
-33.199673639913,-33.1112486588522,-33.0226932296844,-32.9982184075953,
-32.909668864333,-32.8212341273119,-32.7328903887551,-32.6410631395662,
-32.5528218158826,-32.4645939509191,-32.3763581729298,-32.2880931096009,
-32.1997276275461,-32.1113026464833,-32.0227472173137,-31.9982723952439,
-31.9097228519846,-31.8212881149664,-31.7329443764129,-31.6411171272228,
-31.5528758035421,-31.4646479385814,-31.3764121605949,-31.2881470972685,
-31.1997816152164,-31.1113566341565,-31.0228012049898,-30.9983263828925,
-30.9097768396345,-30.8213421026175,-30.7329983640648,-30.6411711148743,
-30.552929791195,-30.4647019262356,-30.3764661482503,-30.2882010849253,
-30.1998356028746,-30.1114106218163,-30.0228551926506,-29.9983803705412,
-29.9109940179612,-29.8237474432069,-29.7365806384812,-29.6494710931914,
-29.5623963544676,-29.4753042131104,-29.3882064147977,-29.3010292666083,
-29.2254902689126),.UNSPECIFIED.);
#292=B_SPLINE_CURVE_WITH_KNOTS('',3,(#31023,#31024,#31025,#31026,#31027,
#31028,#31029,#31030,#31031,#31032,#31033),.UNSPECIFIED.,.F.,.F.,(4,1,1,
1,1,1,1,1,4),(-29.2254902689126,-28.9984343581898,-27.9984883458384,-26.9985423334871,
-25.9985963211357,-24.9986503087843,-23.9987042964329,-22.9987582840816,
-22.942304961733),.UNSPECIFIED.);
#293=B_SPLINE_CURVE_WITH_KNOTS('',3,(#31035,#31036,#31037,#31038,#31039,
#31040,#31041,#31042,#31043,#31044,#31045,#31046,#31047,#31048,#31049,#31050,
#31051,#31052,#31053,#31054,#31055,#31056,#31057,#31058,#31059,#31060,#31061,
#31062,#31063,#31064,#31065,#31066,#31067,#31068,#31069,#31070,#31071,#31072,
#31073,#31074,#31075,#31076,#31077,#31078,#31079,#31080,#31081,#31082,#31083,
#31084,#31085,#31086,#31087,#31088,#31089,#31090,#31091,#31092,#31093,#31094,
#31095,#31096,#31097,#31098,#31099,#31100,#31101,#31102,#31103,#31104,#31105,
#31106,#31107,#31108,#31109,#31110,#31111,#31112,#31113,#31114,#31115,#31116,
#31117,#31118,#31119,#31120,#31121,#31122,#31123,#31124,#31125,#31126,#31127,
#31128,#31129,#31130,#31131,#31132,#31133,#31134,#31135,#31136,#31137,#31138,
#31139,#31140,#31141,#31142,#31143,#31144,#31145,#31146,#31147,#31148,#31149,
#31150,#31151,#31152,#31153,#31154,#31155,#31156,#31157,#31158,#31159,#31160,
#31161,#31162,#31163,#31164,#31165,#31166,#31167,#31168,#31169,#31170,#31171,
#31172,#31173,#31174,#31175,#31176,#31177,#31178,#31179,#31180,#31181,#31182,
#31183,#31184,#31185,#31186,#31187,#31188,#31189,#31190,#31191,#31192,#31193,
#31194,#31195,#31196,#31197,#31198,#31199,#31200,#31201,#31202,#31203,#31204,
#31205,#31206,#31207,#31208,#31209,#31210,#31211,#31212,#31213,#31214,#31215,
#31216,#31217,#31218,#31219,#31220,#31221,#31222,#31223,#31224,#31225,#31226,
#31227,#31228,#31229,#31230,#31231,#31232,#31233,#31234,#31235,#31236,#31237,
#31238,#31239,#31240,#31241,#31242,#31243,#31244,#31245,#31246,#31247,#31248,
#31249,#31250,#31251,#31252,#31253,#31254,#31255,#31256,#31257,#31258,#31259,
#31260),.UNSPECIFIED.,.F.,.F.,(4,3,3,3,3,3,3,3,3,3,3,3,3,3,3,3,3,3,3,3,
3,3,3,3,3,3,3,3,3,3,3,3,3,3,3,3,3,3,3,3,3,3,3,3,3,3,3,3,3,3,3,3,3,3,3,3,
3,3,3,3,3,3,3,3,3,3,3,3,3,3,3,3,3,3,3,4),(-22.942304961733,-22.8545209046868,
-22.766847257432,-22.6792594249928,-22.5917293086245,-22.5042287777375,
-22.4167357403712,-22.3292281149642,-22.2416295280414,-22.1539833092983,
-22.0661961744187,-21.9988122717302,-21.9102627285941,-21.8218279917067,
-21.7334842532916,-21.6416570040525,-21.5534156805278,-21.4651878157292,
-21.3769520379107,-21.2886869747587,-21.2003214928881,-21.1118965120143,
-21.0233410830385,-20.9988662593788,-20.9103167128181,-20.8218819724869,
-20.7335382306125,-20.6417109826644,-20.5534696556644,-20.4652417873905,
-20.3770060061005,-20.2887409394836,-20.2003754541768,-20.1119504698788,
-20.0233950375239,-19.9989202470274,-19.9103707101465,-19.8219359795026,
-19.733592247312,-19.6417649957325,-19.5535236783475,-19.4652958196472,
-19.3770600478799,-19.2887949907244,-19.2004295147407,-19.1120045396972,
-19.0234491164242,-18.9989742346761,-18.9104246903274,-18.8219899522712,
-18.7336462127319,-18.641818963931,-18.5535776393991,-18.465349773638,-18.3771139949023,
-18.2888489308791,-18.2004834482097,-18.1120584665778,-18.02350303691,-17.9990282223247,
-17.9104786578628,-17.8220438995504,-17.7337001396359,-17.6418728984281,
-17.5536315533559,-17.4654036670284,-17.377167867722,-17.2889027831457,
-17.2005372800539,-17.1121122780503,-17.0235568282441,-16.9990822099733,
-16.8956727885515,-16.7927418059338,-16.6906685903549,-16.6591196547798),
 .UNSPECIFIED.);
#294=B_SPLINE_CURVE_WITH_KNOTS('',3,(#31262,#31263,#31264,#31265,#31266,
#31267,#31268,#31269,#31270,#31271,#31272,#31273,#31274,#31275,#31276,#31277,
#31278,#31279,#31280,#31281,#31282,#31283,#31284,#31285,#31286,#31287,#31288,
#31289,#31290,#31291,#31292,#31293,#31294,#31295,#31296,#31297,#31298,#31299,
#31300,#31301,#31302,#31303,#31304,#31305,#31306,#31307,#31308,#31309,#31310,
#31311,#31312,#31313,#31314,#31315,#31316,#31317,#31318,#31319,#31320,#31321,
#31322,#31323,#31324,#31325,#31326,#31327,#31328,#31329,#31330,#31331,#31332,
#31333,#31334,#31335,#31336,#31337,#31338,#31339,#31340,#31341,#31342,#31343,
#31344,#31345,#31346,#31347,#31348,#31349,#31350,#31351,#31352,#31353,#31354,
#31355,#31356,#31357,#31358,#31359,#31360,#31361,#31362,#31363,#31364,#31365,
#31366,#31367,#31368,#31369,#31370,#31371,#31372,#31373,#31374,#31375,#31376,
#31377,#31378,#31379,#31380,#31381,#31382,#31383,#31384,#31385,#31386,#31387,
#31388,#31389,#31390,#31391,#31392,#31393,#31394,#31395,#31396,#31397,#31398,
#31399,#31400,#31401,#31402,#31403,#31404,#31405,#31406,#31407,#31408,#31409,
#31410,#31411,#31412,#31413,#31414,#31415,#31416,#31417,#31418,#31419,#31420,
#31421,#31422,#31423,#31424,#31425,#31426,#31427,#31428,#31429,#31430,#31431,
#31432,#31433,#31434,#31435,#31436,#31437,#31438,#31439,#31440,#31441,#31442,
#31443,#31444,#31445,#31446,#31447,#31448,#31449,#31450,#31451,#31452,#31453,
#31454,#31455,#31456,#31457,#31458,#31459,#31460,#31461,#31462,#31463,#31464,
#31465,#31466,#31467,#31468,#31469,#31470,#31471,#31472,#31473,#31474,#31475,
#31476,#31477,#31478,#31479,#31480,#31481,#31482,#31483,#31484,#31485,#31486,
#31487),.UNSPECIFIED.,.F.,.F.,(4,3,3,3,3,3,3,3,3,3,3,3,3,3,3,3,3,3,3,3,
3,3,3,3,3,3,3,3,3,3,3,3,3,3,3,3,3,3,3,3,3,3,3,3,3,3,3,3,3,3,3,3,3,3,3,3,
3,3,3,3,3,3,3,3,3,3,3,3,3,3,3,3,3,3,3,4),(-16.6591196545534,-16.5708424404528,
-16.4825762959745,-16.3942999901969,-16.3059922899729,-16.2175771928198,
-16.12910117663,-16.0404827781768,-15.999136197622,-15.9105866329858,-15.8221518749269,
-15.7338081156886,-15.6419808743863,-15.5537395310261,-15.4655116467871,
-15.3772758499421,-15.2890107681959,-15.200645268462,-15.112220270127,-15.0236648244138,
-14.9991901852706,-14.9106405100812,-14.8222056404348,-14.7338617687161,
-14.6420345692415,-14.553793111893,-14.4655651133053,-14.3773292018738,
-14.2890640054263,-14.2006983914055,-14.1122732788836,-14.0237177200223,
-13.9992441729192,-13.910694981617,-13.8222605967651,-13.7339172101825,
-13.6420898289807,-13.5538488546178,-13.4656213374149,-13.3773859052664,
-13.2891211854972,-13.2007560418992,-13.1123313967461,-13.0237762971454,
-12.9992981605678,-12.9107483730229,-12.8223133938516,-12.7339694155237,
-12.6421422571103,-12.5539007010024,-12.4656726066969,-12.3774366026758,
-12.2891713168544,-12.2008056186421,-12.1123804248366,-12.023824789566,
-11.9993521482165,-11.9108018171415,-11.8223662871184,-11.7340217513491,
-11.6421947994136,-11.5539526730479,-11.4657240047502,-11.3774874236279,
-11.2892215582218,-11.2008552797222,-11.1124295045045,-11.0238732907307,
-10.9994061358651,-10.9100993890415,-10.8209123500255,-10.7318245035481,
-10.6428246466122,-10.5538777775384,-10.4649060624561,-10.3759343473738),
 .UNSPECIFIED.);
#295=B_SPLINE_CURVE_WITH_KNOTS('',3,(#31488,#31489,#31490,#31491,#31492,
#31493,#31494,#31495,#31496,#31497),.UNSPECIFIED.,.F.,.F.,(4,1,1,1,1,1,
1,4),(-10.3759267393627,-9.99946012351372,-8.99951411116235,-7.99956809881098,
-6.99962208645961,-5.99967607410823,-4.99973006175686,-4.0927579581402),
 .UNSPECIFIED.);
#296=B_SPLINE_CURVE_WITH_KNOTS('',3,(#31500,#31501,#31502,#31503,#31504,
#31505,#31506,#31507,#31508,#31509,#31510,#31511,#31512,#31513,#31514,#31515,
#31516,#31517,#31518,#31519,#31520,#31521,#31522,#31523,#31524,#31525,#31526,
#31527,#31528,#31529,#31530,#31531,#31532,#31533,#31534,#31535,#31536,#31537,
#31538,#31539,#31540,#31541,#31542,#31543,#31544,#31545,#31546,#31547,#31548,
#31549,#31550,#31551,#31552,#31553,#31554,#31555,#31556,#31557,#31558,#31559,
#31560,#31561,#31562,#31563,#31564,#31565,#31566,#31567,#31568,#31569,#31570,
#31571,#31572,#31573,#31574,#31575,#31576,#31577,#31578,#31579,#31580,#31581,
#31582,#31583,#31584,#31585,#31586,#31587,#31588,#31589,#31590,#31591,#31592,
#31593,#31594,#31595,#31596,#31597,#31598,#31599,#31600,#31601,#31602,#31603,
#31604,#31605,#31606,#31607,#31608,#31609,#31610,#31611,#31612,#31613,#31614,
#31615,#31616,#31617,#31618,#31619,#31620,#31621,#31622,#31623,#31624,#31625,
#31626,#31627,#31628,#31629,#31630,#31631,#31632,#31633,#31634,#31635,#31636,
#31637,#31638,#31639,#31640,#31641,#31642,#31643),.UNSPECIFIED.,.F.,.F.,
(4,2,2,2,2,2,2,2,2,2,2,2,2,2,2,2,2,2,2,2,2,2,2,2,2,2,2,2,2,2,2,2,2,2,2,
2,2,2,2,2,2,2,2,2,2,2,2,2,2,2,2,2,2,2,2,2,2,2,2,2,2,2,2,2,2,2,2,2,2,2,2,
4),(0.00584549622467335,0.093405921375881,0.130454269801855,0.139587899175375,
0.143701679159035,0.14678824815488,0.149686852724838,0.153705523253871,
0.164128408972305,0.241981531619902,0.268158297474372,0.296705073611049,
0.300784772366485,0.302502481570271,0.304210123261048,0.306047999034772,
0.309016606254543,0.318500512927684,0.399678224516204,0.447309111008664,
0.457678111996666,0.461978384339338,0.465070615966961,0.467881648682991,
0.47234354095253,0.482917709960205,0.564585567652315,0.60372389239076,0.620985267235939,
0.624516669834605,0.626478597891468,0.628151253543898,0.630258357458671,
0.634388810107199,0.660936540551689,0.736613518874363,0.763293960149108,
0.779708437347709,0.784796539914734,0.788025127073784,0.791034488430205,
0.794957245692005,0.801548971967704,0.852690893089723,0.928853038104393,
0.944722661187104,0.948144328498009,0.950070510781237,0.951745318861767,
0.953888164862695,0.958296575900975,1.01437647864604,1.05723809872353,1.08588504932026,
1.10319606995781,1.10841393049374,1.11169193141533,1.11472499158421,1.11864735127438,
1.12517099269234,1.17139366649591,1.23724911591007,1.25690874508622,1.26426889979486,
1.26959469417094,1.2719145215793,1.27362093904285,1.27547544412718,1.27852147831721,
1.2882877783795,1.36961643020412,1.36975430456593),.UNSPECIFIED.);
#297=B_SPLINE_CURVE_WITH_KNOTS('',3,(#31647,#31648,#31649,#31650,#31651,
#31652,#31653,#31654,#31655,#31656,#31657,#31658,#31659,#31660,#31661,#31662,
#31663,#31664,#31665,#31666,#31667,#31668,#31669,#31670,#31671,#31672,#31673,
#31674,#31675,#31676,#31677),.UNSPECIFIED.,.F.,.F.,(4,3,3,3,3,3,3,3,3,3,
4),(185.353966561968,185.448794091205,185.543475335336,185.638681286969,
185.733128562177,185.827512446235,185.921855079479,186.01767204671,186.112024247931,
186.208573598167,186.305122948402),.UNSPECIFIED.);
#298=B_SPLINE_CURVE_WITH_KNOTS('',3,(#31678,#31679,#31680,#31681,#31682,
#31683,#31684,#31685,#31686,#31687,#31688,#31689,#31690,#31691,#31692,#31693,
#31694,#31695,#31696,#31697,#31698,#31699,#31700,#31701,#31702,#31703,#31704,
#31705,#31706,#31707,#31708,#31709,#31710,#31711,#31712,#31713,#31714,#31715,
#31716,#31717,#31718,#31719,#31720,#31721,#31722,#31723,#31724,#31725,#31726,
#31727,#31728,#31729,#31730,#31731,#31732,#31733,#31734,#31735,#31736,#31737,
#31738,#31739,#31740,#31741,#31742,#31743,#31744,#31745,#31746,#31747),
 .UNSPECIFIED.,.F.,.F.,(4,3,3,3,3,3,3,3,3,3,3,3,3,3,3,3,3,3,3,3,3,3,3,4),
(183.307775588641,183.400962019436,183.494025064816,183.58699217182,183.679894571268,
183.772763733289,183.865624323015,183.95850099185,184.051477988904,184.1445079511,
184.237692355435,184.3052309237,184.397302867067,184.489248064613,184.581095274411,
184.672879103481,184.764630581829,184.856375514756,184.948139696577,185.04001655256,
185.131950850016,185.224060472127,185.305176936051,185.353966561798),
 .UNSPECIFIED.);
#299=B_SPLINE_CURVE_WITH_KNOTS('',3,(#32472,#32473,#32474,#32475,#32476,
#32477,#32478,#32479,#32480,#32481,#32482,#32483,#32484,#32485,#32486,#32487,
#32488,#32489,#32490,#32491,#32492,#32493,#32494,#32495,#32496,#32497,#32498,
#32499,#32500,#32501,#32502,#32503,#32504,#32505,#32506,#32507,#32508,#32509,
#32510,#32511,#32512,#32513,#32514,#32515,#32516,#32517,#32518,#32519,#32520,
#32521,#32522,#32523,#32524,#32525,#32526,#32527,#32528,#32529,#32530,#32531,
#32532,#32533,#32534,#32535,#32536,#32537,#32538,#32539,#32540,#32541,#32542,
#32543,#32544,#32545,#32546,#32547,#32548,#32549,#32550,#32551,#32552,#32553,
#32554,#32555,#32556,#32557,#32558,#32559,#32560,#32561,#32562,#32563,#32564,
#32565),.UNSPECIFIED.,.F.,.F.,(4,3,3,3,3,3,3,3,3,3,3,3,3,3,3,3,3,3,3,3,
3,3,3,3,3,3,3,3,3,3,3,4),(0.,0.0241761716010457,0.0604875164315824,0.0972511013618045,
0.133975157825424,0.147571430754056,0.153998040615924,0.189892464907858,
0.225711369702852,0.260761601706721,0.288115324129052,0.295702130337378,
0.30066260492773,0.335153736964546,0.36871896999146,0.40139690760849,0.422834472706132,
0.435070491669721,0.43982788192227,0.473488311702583,0.507453202697751,
0.541171507612653,0.566357468494487,0.571944200141793,0.604905779750409,
0.637688130984217,0.651026858257536,0.658444655992648,0.664614706512331,
0.696427343348877,0.727373814705075,0.744397949170765),.UNSPECIFIED.);
#300=B_SPLINE_CURVE_WITH_KNOTS('',3,(#32566,#32567,#32568,#32569,#32570,
#32571,#32572,#32573,#32574,#32575,#32576,#32577,#32578,#32579,#32580,#32581,
#32582,#32583,#32584,#32585,#32586,#32587,#32588,#32589,#32590,#32591,#32592,
#32593,#32594,#32595,#32596,#32597,#32598,#32599,#32600,#32601,#32602,#32603,
#32604,#32605,#32606,#32607,#32608,#32609,#32610,#32611,#32612,#32613,#32614,
#32615,#32616,#32617,#32618,#32619,#32620,#32621,#32622,#32623,#32624,#32625,
#32626,#32627,#32628,#32629,#32630,#32631,#32632,#32633,#32634,#32635,#32636,
#32637,#32638,#32639,#32640,#32641,#32642,#32643,#32644,#32645,#32646,#32647,
#32648,#32649,#32650,#32651,#32652,#32653,#32654,#32655,#32656),
 .UNSPECIFIED.,.F.,.F.,(4,3,3,3,3,3,3,3,3,3,3,3,3,3,3,3,3,3,3,3,3,3,3,3,
3,3,3,3,3,3,4),(0.,0.0199602231747668,0.0508723816443174,0.0823900365368249,
0.106689326960221,0.118838972171919,0.126476351449351,0.130988617383617,
0.163718139381269,0.196968473281095,0.230459187891393,0.259483610402608,
0.263706435719309,0.298090982061561,0.332366604613236,0.364032629283523,
0.387610012978702,0.395474382928205,0.402776496513689,0.43735314616912,
0.471952684989827,0.507230106948907,0.541083095135413,0.546695484975304,
0.582678619508019,0.618902355831596,0.635230940109389,0.645245254509382,
0.682087619663568,0.718444888016225,0.741270768406373),.UNSPECIFIED.);
#301=B_SPLINE_CURVE_WITH_KNOTS('',3,(#33382,#33383,#33384,#33385,#33386,
#33387,#33388,#33389,#33390,#33391,#33392,#33393,#33394,#33395,#33396,#33397,
#33398,#33399,#33400,#33401,#33402,#33403,#33404,#33405,#33406,#33407,#33408,
#33409,#33410,#33411,#33412,#33413,#33414,#33415,#33416,#33417,#33418,#33419,
#33420,#33421,#33422,#33423,#33424,#33425,#33426,#33427,#33428,#33429,#33430,
#33431,#33432,#33433,#33434,#33435,#33436,#33437,#33438,#33439,#33440,#33441,
#33442,#33443,#33444,#33445,#33446,#33447,#33448,#33449,#33450,#33451,#33452,
#33453,#33454,#33455,#33456,#33457,#33458,#33459,#33460,#33461,#33462,#33463,
#33464,#33465,#33466,#33467,#33468,#33469,#33470,#33471,#33472),
 .UNSPECIFIED.,.F.,.F.,(4,3,3,3,3,3,3,3,3,3,3,3,3,3,3,3,3,3,3,3,3,3,3,3,
3,3,3,3,3,3,4),(0.,0.0199602231747703,0.0508325943020119,0.0823137401186949,
0.114499218705538,0.125197051716921,0.130988613640588,0.163718126795733,
0.19696845695766,0.230459172327224,0.259483613438486,0.263706438258355,
0.298090983919407,0.332366606139957,0.364032629283524,0.387610012978706,
0.395474380525451,0.401789396924481,0.435694450351821,0.470229671357451,
0.505471622292725,0.5345543541377,0.54108302961338,0.546695468865373,0.5826459540699,
0.618859895288609,0.635230906731221,0.644561776401932,0.681404605551153,
0.717768931114021,0.741270768406441),.UNSPECIFIED.);
#302=B_SPLINE_CURVE_WITH_KNOTS('',3,(#33473,#33474,#33475,#33476),
 .UNSPECIFIED.,.F.,.F.,(4,4),(0.,0.0151628972499269),.UNSPECIFIED.);
#303=B_SPLINE_CURVE_WITH_KNOTS('',3,(#33477,#33478,#33479,#33480,#33481,
#33482,#33483,#33484,#33485,#33486,#33487,#33488,#33489,#33490,#33491,#33492,
#33493,#33494,#33495,#33496,#33497,#33498,#33499,#33500,#33501,#33502,#33503,
#33504,#33505,#33506,#33507,#33508,#33509,#33510,#33511,#33512,#33513,#33514,
#33515,#33516,#33517,#33518,#33519,#33520,#33521,#33522,#33523,#33524,#33525,
#33526,#33527,#33528,#33529,#33530,#33531,#33532,#33533,#33534,#33535,#33536,
#33537,#33538,#33539,#33540,#33541,#33542,#33543,#33544,#33545,#33546,#33547,
#33548,#33549,#33550,#33551,#33552,#33553,#33554,#33555,#33556,#33557,#33558,
#33559,#33560,#33561,#33562,#33563,#33564,#33565,#33566,#33567),
 .UNSPECIFIED.,.F.,.F.,(4,3,3,3,3,3,3,3,3,3,3,3,3,3,3,3,3,3,3,3,3,3,3,3,
3,3,3,3,3,3,4),(0.,0.0241761716010214,0.0604875142823813,0.0972510993394287,
0.133975152747319,0.14757142866777,0.153998039183633,0.189892463368544,
0.225711365233482,0.260761585954893,0.28811529479708,0.295702013482264,
0.300662585464541,0.335153710250192,0.36871892746383,0.401396907608365,
0.422016977849024,0.432236392759498,0.440631052868171,0.474302686606213,
0.508270521577337,0.541982161358676,0.566357469533634,0.571944201298751,
0.605035401265075,0.637484032208542,0.658444729985083,0.664614717127708,
0.696427371609928,0.727373866046416,0.744397949170599),.UNSPECIFIED.);
#304=B_SPLINE_CURVE_WITH_KNOTS('',3,(#33626,#33627,#33628,#33629,#33630,
#33631,#33632,#33633,#33634,#33635,#33636,#33637,#33638,#33639,#33640,#33641,
#33642,#33643,#33644,#33645,#33646,#33647,#33648,#33649,#33650,#33651,#33652,
#33653,#33654,#33655,#33656,#33657,#33658,#33659,#33660,#33661,#33662,#33663,
#33664,#33665,#33666,#33667,#33668,#33669,#33670,#33671,#33672,#33673,#33674,
#33675,#33676,#33677,#33678,#33679,#33680,#33681,#33682,#33683,#33684,#33685,
#33686,#33687,#33688,#33689,#33690,#33691,#33692,#33693,#33694,#33695,#33696,
#33697,#33698,#33699,#33700,#33701,#33702,#33703,#33704,#33705,#33706,#33707,
#33708,#33709,#33710,#33711,#33712,#33713,#33714,#33715,#33716,#33717,#33718,
#33719,#33720,#33721,#33722,#33723,#33724,#33725,#33726,#33727,#33728,#33729,
#33730,#33731),.UNSPECIFIED.,.F.,.F.,(4,3,3,3,3,3,3,3,3,3,3,3,3,3,3,3,3,
3,3,3,3,3,3,3,3,3,3,3,3,3,3,3,3,3,3,4),(-157.874592628305,-157.786189611785,
-157.697869990434,-157.609576734025,-157.521341336046,-157.433113405113,
-157.344871570897,-157.256534662964,-157.168154411437,-157.079625306774,
-156.991523939165,-156.902974396096,-156.814539659262,-156.726195920889,
-156.634368671629,-156.546127348114,-156.457899483313,-156.369663705481,
-156.281398642303,-156.193033160389,-156.104608179461,-156.016052750418,
-155.991577926814,-155.903028384309,-155.814593648058,-155.726249910282,
-155.634422660805,-155.546181337927,-155.457953473776,-155.369717696606,
-155.281452634103,-155.193087152878,-155.104662172649,-155.016106744312,
-154.991631914463,-154.889196412504),.UNSPECIFIED.);
#305=B_SPLINE_CURVE_WITH_KNOTS('',3,(#33734,#33735,#33736,#33737,#33738,
#33739,#33740,#33741,#33742,#33743,#33744,#33745,#33746,#33747,#33748,#33749,
#33750,#33751,#33752,#33753,#33754,#33755,#33756,#33757,#33758,#33759,#33760,
#33761,#33762,#33763,#33764,#33765,#33766,#33767,#33768,#33769,#33770,#33771,
#33772,#33773,#33774,#33775,#33776,#33777,#33778,#33779,#33780,#33781,#33782,
#33783,#33784,#33785,#33786,#33787,#33788,#33789,#33790,#33791,#33792,#33793,
#33794,#33795,#33796,#33797,#33798,#33799,#33800,#33801,#33802,#33803,#33804,
#33805,#33806,#33807,#33808,#33809,#33810,#33811,#33812,#33813,#33814,#33815,
#33816,#33817,#33818,#33819,#33820,#33821,#33822,#33823,#33824,#33825,#33826,
#33827,#33828,#33829,#33830,#33831,#33832,#33833,#33834,#33835,#33836,#33837,
#33838,#33839,#33840,#33841,#33842,#33843,#33844,#33845,#33846,#33847,#33848,
#33849,#33850,#33851,#33852,#33853,#33854,#33855,#33856,#33857,#33858,#33859,
#33860,#33861,#33862,#33863,#33864,#33865,#33866,#33867,#33868,#33869,#33870,
#33871,#33872,#33873,#33874,#33875),.UNSPECIFIED.,.F.,.F.,(4,3,3,3,3,3,
3,3,3,3,3,3,3,3,3,3,3,3,3,3,3,3,3,3,3,3,3,3,3,3,3,3,3,3,3,3,3,3,3,3,3,3,
3,3,3,3,3,4),(151.906492583222,151.991793877409,152.080343420566,152.168778157483,
152.257121895935,152.348949145163,152.437190468744,152.525418333606,152.613654111494,
152.701919174722,152.790284656678,152.878709637644,152.967265066718,152.99173988976,
153.080289432964,153.168724169926,153.257067908422,153.348895157633,153.437136481254,
153.525364346154,153.61360012408,153.701865187344,153.790230669334,153.878655650331,
153.967211079435,153.991685902111,154.08023544587,154.16867018339,154.257013922446,
154.348841171448,154.43708249563,154.52531036109,154.613546139575,154.701811203397,
154.790176685939,154.878601667486,154.967157097132,154.991631914463,155.080192114906,
155.173042552799,155.261373796928,155.349645458985,155.437878960375,155.526095688543,
155.614346382667,155.702616937377,155.790964593394,155.822995618054),
 .UNSPECIFIED.);
#306=B_SPLINE_CURVE_WITH_KNOTS('',3,(#33881,#33882,#33883,#33884,#33885,
#33886,#33887,#33888,#33889,#33890,#33891,#33892,#33893,#33894,#33895,#33896,
#33897,#33898,#33899,#33900,#33901,#33902,#33903,#33904,#33905,#33906,#33907,
#33908,#33909,#33910,#33911,#33912,#33913,#33914,#33915,#33916,#33917,#33918,
#33919,#33920,#33921,#33922,#33923,#33924,#33925,#33926,#33927,#33928,#33929,
#33930,#33931,#33932,#33933,#33934,#33935,#33936,#33937,#33938,#33939,#33940,
#33941,#33942,#33943,#33944,#33945,#33946,#33947,#33948,#33949,#33950,#33951,
#33952,#33953,#33954,#33955,#33956,#33957,#33958,#33959,#33960,#33961,#33962,
#33963,#33964,#33965,#33966,#33967,#33968,#33969,#33970,#33971,#33972,#33973,
#33974,#33975,#33976,#33977,#33978,#33979,#33980,#33981,#33982,#33983,#33984,
#33985,#33986,#33987,#33988,#33989,#33990,#33991,#33992,#33993,#33994,#33995,
#33996,#33997,#33998,#33999,#34000,#34001,#34002,#34003,#34004,#34005,#34006,
#34007,#34008,#34009,#34010,#34011,#34012,#34013,#34014,#34015,#34016,#34017,
#34018,#34019,#34020,#34021,#34022,#34023,#34024,#34025,#34026,#34027,#34028,
#34029,#34030,#34031,#34032,#34033,#34034,#34035,#34036,#34037,#34038,#34039,
#34040,#34041,#34042,#34043,#34044,#34045,#34046,#34047,#34048,#34049,#34050,
#34051,#34052,#34053,#34054,#34055),.UNSPECIFIED.,.F.,.F.,(4,3,3,3,3,3,
3,3,3,3,3,3,3,3,3,3,3,3,3,3,3,3,3,3,3,3,3,3,3,3,3,3,3,3,3,3,3,3,3,3,3,3,
3,3,3,3,3,3,3,3,3,3,3,3,3,3,3,3,4),(140.743350880823,140.831741437458,140.920276004824,
140.992387741544,141.080937284805,141.169372021824,141.257715760379,141.349543009569,
141.437784333251,141.526012198212,141.6142479762,141.702513039528,141.790878521581,
141.879303502642,141.96785893181,141.992333753895,142.080883297156,142.169318034175,
142.257661772731,142.34948902192,142.437730345602,142.525958210564,142.614193988552,
142.702459051879,142.790824533932,142.879249514994,142.967804944162,142.992279766246,
143.080829309507,143.169264046527,143.257607785082,143.349435034271,143.437676357953,
143.525904222915,143.614140000903,143.70240506423,143.790770546284,143.879195527345,
143.967750956513,143.992225778598,144.080775321858,144.169210058877,144.257553797432,
144.349381046622,144.437622370303,144.525850235265,144.614086013251,144.702351076578,
144.79071655863,144.879141539691,144.967696968859,144.992171790949,145.081319122906,
145.170348342848,145.259280195558,145.350286965679,145.439082830911,145.531195053476,
145.623307276042),.UNSPECIFIED.);
#307=B_SPLINE_CURVE_WITH_KNOTS('',3,(#34058,#34059,#34060,#34061,#34062,
#34063,#34064,#34065,#34066,#34067,#34068,#34069,#34070,#34071,#34072,#34073,
#34074,#34075,#34076,#34077,#34078,#34079,#34080,#34081,#34082,#34083,#34084,
#34085,#34086,#34087,#34088,#34089,#34090,#34091,#34092,#34093,#34094,#34095,
#34096,#34097,#34098,#34099,#34100,#34101,#34102,#34103,#34104,#34105,#34106,
#34107,#34108,#34109,#34110,#34111,#34112,#34113,#34114,#34115,#34116,#34117,
#34118,#34119,#34120,#34121,#34122,#34123,#34124,#34125,#34126,#34127,#34128,
#34129,#34130,#34131,#34132,#34133,#34134,#34135,#34136,#34137,#34138,#34139,
#34140,#34141,#34142,#34143,#34144,#34145,#34146,#34147,#34148,#34149,#34150,
#34151,#34152,#34153,#34154,#34155,#34156,#34157,#34158,#34159,#34160,#34161,
#34162,#34163,#34164,#34165,#34166,#34167,#34168,#34169,#34170,#34171,#34172,
#34173,#34174,#34175,#34176,#34177,#34178,#34179,#34180,#34181,#34182,#34183,
#34184,#34185,#34186,#34187,#34188,#34189,#34190,#34191,#34192,#34193,#34194,
#34195,#34196,#34197,#34198,#34199,#34200,#34201,#34202,#34203,#34204,#34205,
#34206,#34207,#34208,#34209,#34210,#34211,#34212,#34213,#34214,#34215,#34216,
#34217,#34218,#34219,#34220,#34221,#34222,#34223,#34224,#34225,#34226,#34227,
#34228,#34229,#34230,#34231,#34232,#34233,#34234,#34235,#34236,#34237,#34238,
#34239,#34240,#34241,#34242,#34243,#34244,#34245,#34246,#34247,#34248,#34249,
#34250,#34251,#34252,#34253,#34254,#34255,#34256,#34257,#34258,#34259,#34260,
#34261,#34262,#34263,#34264,#34265,#34266,#34267,#34268),.UNSPECIFIED.,
 .F.,.F.,(4,3,3,3,3,3,3,3,3,3,3,3,3,3,3,3,3,3,3,3,3,3,3,3,3,3,3,3,3,3,3,
3,3,3,3,3,3,3,3,3,3,3,3,3,3,3,3,3,3,3,3,3,3,3,3,3,3,3,3,3,3,3,3,3,3,3,3,
3,3,3,4),(-148.606011105325,-148.516896311246,-148.427765779446,-148.338599573289,
-148.249313397802,-148.159965224952,-148.070452324036,-147.992009828003,
-147.903460284745,-147.815025547728,-147.726681809176,-147.634854559986,
-147.546613236307,-147.458385371348,-147.370149593363,-147.281884530039,
-147.193519047988,-147.10509406693,-147.016538637765,-146.992063815652,
-146.903514272392,-146.815079535374,-146.72673579682,-146.63490854763,-146.546667223949,
-146.458439358988,-146.370203581002,-146.281938517676,-146.193573035624,
-146.105148054564,-146.016592625397,-145.9921178033,-145.903568260038,-145.815133523017,
-145.72678978446,-145.634962535271,-145.546721211588,-145.458493346624,
-145.370257568635,-145.281992505305,-145.19362702325,-145.105202042187,
-145.016646613017,-144.992171790949,-144.903622247689,-144.81518751067,
-144.726843772116,-144.635016522926,-144.546775199245,-144.458547334283,
-144.370311556296,-144.28204649297,-144.193681010918,-144.105256029857,
-144.016700600689,-143.992225778598,-143.903676235337,-143.815241498317,
-143.726897759762,-143.635070510573,-143.54682918689,-143.458601321928,
-143.37036554394,-143.282100480614,-143.193734998561,-143.1053100175,-143.016754588331,
-142.992279766246,-142.903798486074,-142.815448035224,-142.804552478338),
 .UNSPECIFIED.);
#308=B_SPLINE_CURVE_WITH_KNOTS('',3,(#34274,#34275,#34276,#34277,#34278),
 .UNSPECIFIED.,.F.,.F.,(4,1,4),(164.458927397274,165.306256689024,166.198929965428),
 .UNSPECIFIED.);
#309=B_SPLINE_CURVE_WITH_KNOTS('',3,(#34282,#34283,#34284,#34285,#34286,
#34287,#34288,#34289,#34290,#34291,#34292,#34293,#34294,#34295,#34296,#34297,
#34298,#34299,#34300,#34301,#34302,#34303,#34304,#34305,#34306,#34307,#34308,
#34309,#34310,#34311,#34312,#34313,#34314,#34315,#34316,#34317,#34318,#34319,
#34320,#34321),.UNSPECIFIED.,.F.,.F.,(4,2,2,2,2,2,2,2,2,2,2,2,2,2,2,2,2,
2,2,4),(-4.06137411129811,-4.03546814208168,-4.03260936723115,-4.03068543622094,
-4.02910207865154,-4.02742394594966,-4.02528765473165,-4.02188101107949,
-4.00378125912536,-3.99087511127817,-3.92336215122477,-3.89390000861074,
-3.87625324670922,-3.87100804923103,-3.86772941140725,-3.86470704756532,
-3.86081439142151,-3.85437488405435,-3.81121148531092,-3.76149375020669),
 .UNSPECIFIED.);
#310=B_SPLINE_CURVE_WITH_KNOTS('',3,(#34322,#34323,#34324,#34325,#34326,
#34327,#34328,#34329,#34330,#34331,#34332,#34333,#34334,#34335,#34336,#34337,
#34338,#34339,#34340,#34341,#34342,#34343,#34344,#34345,#34346,#34347,#34348,
#34349,#34350,#34351,#34352,#34353,#34354,#34355,#34356,#34357,#34358,#34359,
#34360,#34361,#34362,#34363,#34364,#34365,#34366,#34367,#34368,#34369,#34370,
#34371,#34372,#34373,#34374,#34375,#34376,#34377,#34378,#34379,#34380,#34381,
#34382,#34383,#34384,#34385,#34386,#34387,#34388,#34389,#34390,#34391,#34392,
#34393,#34394,#34395,#34396,#34397,#34398,#34399,#34400,#34401,#34402,#34403,
#34404,#34405,#34406,#34407,#34408,#34409),.UNSPECIFIED.,.F.,.F.,(4,2,2,
2,2,2,2,2,2,2,2,2,2,2,2,2,2,2,2,2,2,2,2,2,2,2,2,2,2,2,2,2,2,2,2,2,2,2,2,
2,2,2,2,4),(-0.662156536932336,-0.648956013746852,-0.621418192193571,-0.617234499775957,
-0.615108581233505,-0.613431055280487,-0.611475622140756,-0.607966632969675,
-0.591020215921372,-0.514722936640716,-0.465485531341795,-0.458903121030178,
-0.454968378544555,-0.451939320614257,-0.448679115744897,-0.443518536519126,
-0.426662623721119,-0.399038694208074,-0.355194168524487,-0.298655849376382,
-0.294253481146245,-0.292112018854427,-0.290433286732513,-0.290426632483179,
-0.290420084506535,-0.290413640687297,-0.290407299018121,-0.290401057478961,
-0.2903949140909,-0.288474887817562,-0.285144057785002,-0.280975459144695,
-0.272195312542459,-0.246600417983609,-0.184345430883523,-0.142200987206802,
-0.135789521101596,-0.13190488755513,-0.128883447241603,-0.125600486147694,
-0.120336747935594,-0.102516454894325,-0.0726393233951299,-0.000963379534404715),
 .UNSPECIFIED.);
#311=B_SPLINE_CURVE_WITH_KNOTS('',3,(#34415,#34416,#34417,#34418,#34419,
#34420,#34421,#34422,#34423,#34424,#34425,#34426,#34427,#34428,#34429,#34430,
#34431,#34432,#34433,#34434,#34435,#34436,#34437,#34438,#34439,#34440,#34441,
#34442,#34443,#34444,#34445,#34446,#34447,#34448,#34449,#34450,#34451,#34452,
#34453,#34454,#34455,#34456,#34457,#34458,#34459,#34460,#34461,#34462,#34463,
#34464,#34465,#34466,#34467,#34468,#34469,#34470,#34471,#34472,#34473,#34474,
#34475,#34476,#34477,#34478,#34479,#34480,#34481,#34482,#34483,#34484,#34485,
#34486,#34487,#34488,#34489,#34490),.UNSPECIFIED.,.F.,.F.,(4,2,2,2,2,2,
2,2,2,2,2,2,2,2,2,2,2,2,2,2,2,2,2,2,2,2,2,2,2,2,2,2,2,2,2,2,2,4),(-4.0614630673581,
-4.05235423870892,-3.96283840444798,-3.93777252469754,-3.93188013811726,
-3.92845778818342,-3.92546300471007,-3.92175396700727,-3.91606035920602,
-3.88902746696132,-3.8050304357142,-3.78310043186638,-3.77517962828362,
-3.77130702260846,-3.76816909778494,-3.76629336885218,-3.76469327318415,
-3.76255009404327,-3.75814060112062,-3.7020680575884,-3.65787276096341,
-3.6302390214585,-3.6133762570027,-3.60821407922187,-3.60495294503442,-3.60192307173183,
-3.59798732806223,-3.59140329432733,-3.54215389317604,-3.4657303365375,
-3.44886309154659,-3.44535811526621,-3.44340319417903,-3.44172502335401,
-3.43959686996878,-3.43540447334862,-3.40763336833459,-3.40023537643569),
 .UNSPECIFIED.);
#312=B_SPLINE_CURVE_WITH_KNOTS('',3,(#34491,#34492,#34493,#34494,#34495,
#34496,#34497,#34498,#34499),.UNSPECIFIED.,.F.,.F.,(4,1,1,1,1,1,4),(160.22122533308,
160.306526627267,161.306472639618,162.306418651969,163.306364664321,164.306310676672,
164.458927397274),.UNSPECIFIED.);
#313=B_SPLINE_CURVE_WITH_KNOTS('',3,(#34500,#34501,#34502,#34503,#34504,
#34505,#34506,#34507,#34508,#34509,#34510,#34511,#34512,#34513,#34514,#34515,
#34516,#34517,#34518,#34519,#34520,#34521,#34522,#34523,#34524,#34525,#34526,
#34527,#34528,#34529,#34530,#34531,#34532,#34533,#34534,#34535,#34536,#34537,
#34538,#34539,#34540,#34541,#34542,#34543,#34544,#34545,#34546,#34547,#34548,
#34549,#34550,#34551,#34552,#34553,#34554,#34555,#34556,#34557,#34558,#34559,
#34560,#34561,#34562,#34563,#34564,#34565,#34566,#34567,#34568,#34569,#34570,
#34571,#34572,#34573,#34574,#34575,#34576,#34577,#34578,#34579,#34580,#34581,
#34582,#34583,#34584,#34585,#34586,#34587,#34588,#34589,#34590,#34591,#34592,
#34593,#34594,#34595,#34596,#34597,#34598,#34599,#34600,#34601,#34602,#34603,
#34604,#34605,#34606,#34607,#34608,#34609,#34610,#34611,#34612,#34613,#34614,
#34615,#34616,#34617,#34618,#34619,#34620,#34621,#34622,#34623,#34624,#34625,
#34626,#34627,#34628,#34629,#34630,#34631,#34632,#34633,#34634,#34635,#34636,
#34637,#34638,#34639,#34640,#34641,#34642,#34643,#34644,#34645,#34646,#34647,
#34648,#34649,#34650,#34651,#34652,#34653,#34654,#34655,#34656,#34657,#34658,
#34659,#34660,#34661,#34662,#34663,#34664,#34665,#34666,#34667,#34668,#34669,
#34670,#34671,#34672,#34673,#34674,#34675,#34676,#34677,#34678,#34679,#34680,
#34681,#34682,#34683,#34684,#34685,#34686,#34687,#34688,#34689,#34690,#34691,
#34692,#34693,#34694,#34695,#34696,#34697,#34698,#34699,#34700,#34701,#34702,
#34703,#34704,#34705,#34706,#34707,#34708,#34709,#34710,#34711),
 .UNSPECIFIED.,.F.,.F.,(4,2,2,2,2,2,2,2,2,2,2,2,2,2,2,2,2,2,2,2,2,2,2,2,
2,2,2,2,2,2,2,2,2,2,2,2,2,2,2,2,2,2,2,2,2,2,2,2,2,2,2,2,2,2,2,2,2,2,2,2,
2,2,2,2,2,2,2,2,2,2,2,2,2,2,2,2,2,2,2,2,2,2,2,2,2,2,2,2,2,2,2,2,2,2,2,2,
2,2,2,2,2,2,2,2,2,4),(-2.69232820337898,-2.65215331755146,-2.57610388787892,
-2.55874252190226,-2.55520845908299,-2.55324739746129,-2.55157016471346,
-2.54945118635699,-2.5453008033091,-2.51868116942949,-2.44436574494018,
-2.41690138391812,-2.40011266218735,-2.39495896467106,-2.391699930452,-2.38866976400286,
-2.38473045818825,-2.37813347333805,-2.32868997370835,-2.25191573891669,
-2.23552390746872,-2.23204851955261,-2.23010018678417,-2.22842149070606,
-2.22628472487605,-2.22287778578281,-2.20478565495202,-2.1045602781164,
-2.07843784358157,-2.07247131749459,-2.06903277073797,-2.06603972630721,
-2.06235328025359,-2.05673239951629,-2.03080471296937,-1.97580982653872,
-1.94588728187544,-1.93779308354745,-1.9134451694628,-1.90938428253259,
-1.90728467757254,-1.90560885148976,-1.90363318936277,-1.90003129527163,
-1.88145719932781,-1.80063827631087,-1.7574399740288,-1.75099908058603,
-1.74710571190354,-1.7440828863301,-1.74080384074389,-1.73555819605331,
-1.71791208240507,-1.68844885628179,-1.63096870377777,-1.59100057425755,
-1.58650919985396,-1.58435018577139,-1.5826697993837,-1.5807373452675,-1.57733328749,
-1.56202461388756,-1.48445088468712,-1.43468019637624,-1.42808727138658,
-1.42414948173725,-1.42111996890225,-1.41786113492771,-1.41270668666146,
-1.39590617689815,-1.36840897502444,-1.29423806712174,-1.26748633929008,
-1.26333151633647,-1.2612117690953,-1.25953470699639,-1.25757473367821,
-1.25404488214976,-1.23674817735237,-1.16070716478711,-1.11159742061136,
-1.10501758302102,-1.10108359618052,-1.09805466260356,-1.0947941410465,
-1.08963210011751,-1.07276280810492,-1.04510818063073,-0.972368929468456,
-0.944493035068862,-0.940299499291466,-0.938171484898872,-0.936493800339113,
-0.934539899570493,-0.931037926828355,-0.914207256388892,-0.837824288323109,
-0.788545872915298,-0.781962655556508,-0.778027682083294,-0.774998593294991,
-0.771738499937146,-0.766578405634705,-0.749726837719345,-0.7221128406229,
-0.662156536932336),.UNSPECIFIED.);
#314=B_SPLINE_CURVE_WITH_KNOTS('',3,(#34718,#34719,#34720,#34721,#34722,
#34723,#34724,#34725,#34726,#34727,#34728,#34729,#34730,#34731,#34732,#34733,
#34734,#34735,#34736,#34737,#34738,#34739,#34740,#34741,#34742,#34743,#34744,
#34745,#34746,#34747,#34748,#34749,#34750,#34751,#34752,#34753),
 .UNSPECIFIED.,.F.,.F.,(4,2,2,2,2,2,2,2,2,2,2,2,2,2,2,2,2,4),(-1.37015241264804,
-1.35570167221927,-1.34911020280277,-1.34517184391813,-1.34214104368373,
-1.33887998266,-1.33372020388906,-1.31688586729512,-1.28931555875076,-1.21574475579553,
-1.18851814157379,-1.18434507533776,-1.18222082213135,-1.18054267426951,
-1.17858425479071,-1.17506423658523,-1.15795382549888,-1.12238864779317),
 .UNSPECIFIED.);
#315=B_SPLINE_CURVE_WITH_KNOTS('',3,(#35478,#35479,#35480,#35481,#35482,
#35483,#35484,#35485,#35486,#35487,#35488,#35489,#35490,#35491),
 .UNSPECIFIED.,.F.,.F.,(4,2,2,2,2,2,4),(0.0079371660209936,0.157935777681907,
0.317600902596195,0.481956426355492,0.644216700819685,0.777027678467974,
0.901017531905197),.UNSPECIFIED.);
#316=B_SPLINE_CURVE_WITH_KNOTS('',3,(#35492,#35493,#35494,#35495,#35496,
#35497,#35498,#35499,#35500,#35501),.UNSPECIFIED.,.F.,.F.,(4,1,1,1,1,1,
1,4),(145.623314962503,145.9921178033,146.992063815652,147.992009828003,
148.991955840354,149.991901852706,150.991847865057,151.906483871255),
 .UNSPECIFIED.);
#317=B_SPLINE_CURVE_WITH_KNOTS('',3,(#35502,#35503,#35504,#35505,#35506,
#35507,#35508,#35509,#35510,#35511,#35512,#35513,#35514,#35515),
 .UNSPECIFIED.,.F.,.F.,(4,2,2,2,2,2,4),(0.0050079574061546,0.120802454330559,
0.259394492895916,0.351675444238468,0.427932493074399,0.483828923769819,
0.523620932636945),.UNSPECIFIED.);
#318=B_SPLINE_CURVE_WITH_KNOTS('',3,(#35516,#35517,#35518,#35519,#35520,
#35521,#35522,#35523,#35524,#35525,#35526,#35527,#35528,#35529,#35530,#35531,
#35532,#35533,#35534,#35535,#35536,#35537,#35538,#35539,#35540,#35541,#35542,
#35543,#35544,#35545,#35546,#35547,#35548,#35549,#35550,#35551,#35552,#35553,
#35554,#35555,#35556,#35557,#35558,#35559,#35560,#35561,#35562,#35563,#35564,
#35565,#35566,#35567,#35568,#35569,#35570,#35571,#35572,#35573,#35574,#35575,
#35576,#35577,#35578,#35579,#35580,#35581,#35582,#35583,#35584,#35585,#35586,
#35587,#35588,#35589,#35590,#35591,#35592,#35593,#35594,#35595,#35596,#35597,
#35598,#35599,#35600,#35601,#35602,#35603,#35604,#35605,#35606,#35607,#35608,
#35609,#35610,#35611,#35612,#35613,#35614,#35615,#35616,#35617,#35618,#35619,
#35620,#35621,#35622,#35623,#35624,#35625,#35626,#35627,#35628,#35629,#35630,
#35631,#35632,#35633,#35634,#35635,#35636,#35637,#35638,#35639,#35640,#35641,
#35642,#35643,#35644,#35645,#35646,#35647,#35648,#35649,#35650,#35651,#35652,
#35653,#35654,#35655,#35656,#35657,#35658,#35659,#35660,#35661,#35662,#35663,
#35664,#35665,#35666,#35667,#35668,#35669,#35670,#35671,#35672,#35673,#35674,
#35675,#35676,#35677,#35678,#35679,#35680,#35681,#35682,#35683,#35684,#35685,
#35686,#35687,#35688,#35689,#35690,#35691,#35692,#35693,#35694,#35695,#35696,
#35697,#35698,#35699,#35700,#35701,#35702,#35703,#35704,#35705,#35706,#35707,
#35708,#35709,#35710,#35711,#35712,#35713,#35714,#35715,#35716,#35717,#35718,
#35719,#35720,#35721,#35722,#35723,#35724,#35725,#35726,#35727,#35728,#35729),
 .UNSPECIFIED.,.F.,.F.,(4,2,2,2,2,2,2,2,2,2,2,2,2,2,2,2,2,2,2,2,2,2,2,2,
2,2,2,2,2,2,2,2,2,2,2,2,2,2,2,2,2,2,2,2,2,2,2,2,2,2,2,2,2,2,2,2,2,2,2,2,
2,2,2,2,2,2,2,2,2,2,2,2,2,2,2,2,2,2,2,2,2,2,2,2,2,2,2,2,2,2,2,2,2,2,2,2,
2,2,2,2,2,2,2,2,2,2,4),(-3.40023537643569,-3.33482078185619,-3.30719486950161,
-3.29033523387914,-3.28517320247625,-3.28191197376044,-3.27888188358579,
-3.27494567499668,-3.26836045983183,-3.21906860335362,-3.1425569306785,
-3.12580076494813,-3.12230240871166,-3.12034886027345,-3.11867042783018,
-3.11654008924492,-3.1123377816331,-3.08421993346944,-3.01182460862819,
-2.98415801707282,-2.96728033953895,-2.96211612285055,-2.95885428238125,
-2.95582415422582,-2.95188864913119,-2.94530626920494,-2.89617337285961,
-2.81998983409003,-2.80278126440513,-2.79925552182887,-2.79729593292003,
-2.79561801718591,-2.7934956514125,-2.78933106242006,-2.76233708521128,
-2.68852255018912,-2.66100033844717,-2.64418544131733,-2.63902794809165,
-2.63576747103202,-2.63273661807035,-2.62879734251646,-2.62220241790063,
-2.57245296636962,-2.49483755632898,-2.47947731681429,-2.47606857340942,
-2.47413450500865,-2.47245336709749,-2.47029422017985,-2.46580539845458,
-2.4262386953559,-2.36847625742542,-2.33896598030259,-2.32129602970495,
-2.31604619892625,-2.3127651407173,-2.30974086132929,-2.30584617027375,
-2.29940420549618,-2.25626330165687,-2.19386345910526,-2.16905381699869,
-2.1561088099532,-2.15288002433365,-2.1509856900146,-2.14929700013531,-2.14710888804055,
-2.14345323594964,-2.12034146941491,-2.10962599753095,-2.03152314379028,
-2.02122744771306,-1.99944375006007,-1.99361917422242,-1.99017733836269,
-1.98718316977388,-1.9834975552179,-1.97637918050148,-1.9200651726639,-1.85963851291728,
-1.83458282172232,-1.83049138590502,-1.82838461643966,-1.8267076302322,
-1.82473587112967,-1.82115458829943,-1.80297942502917,-1.72618180678269,
-1.67871268495384,-1.67216469347124,-1.66823897361453,-1.66521007514229,
-1.66194332995739,-1.65675802400204,-1.6396911344249,-1.6115862890577,-1.54671124652989,
-1.51195632735406,-1.50752256950061,-1.50537423955513,-1.50369411251794,
-1.50175277797187,-1.49831093281251,-1.48245266118319,-1.40528043645708,
-1.37015241264804),.UNSPECIFIED.);
#319=B_SPLINE_CURVE_WITH_KNOTS('',3,(#35732,#35733,#35734,#35735,#35736,
#35737,#35738,#35739,#35740,#35741,#35742,#35743,#35744,#35745,#35746,#35747,
#35748,#35749,#35750,#35751,#35752,#35753,#35754,#35755,#35756,#35757,#35758,
#35759,#35760,#35761,#35762,#35763,#35764,#35765,#35766,#35767,#35768,#35769,
#35770,#35771,#35772,#35773,#35774,#35775,#35776,#35777,#35778,#35779,#35780,
#35781,#35782,#35783,#35784,#35785,#35786,#35787,#35788,#35789,#35790,#35791,
#35792,#35793,#35794,#35795,#35796,#35797,#35798,#35799,#35800,#35801,#35802,
#35803,#35804,#35805,#35806,#35807,#35808,#35809,#35810,#35811,#35812,#35813,
#35814,#35815,#35816,#35817,#35818,#35819,#35820,#35821,#35822,#35823,#35824,
#35825,#35826,#35827,#35828,#35829,#35830,#35831,#35832,#35833,#35834,#35835,
#35836,#35837,#35838,#35839,#35840,#35841,#35842,#35843,#35844,#35845,#35846,
#35847,#35848,#35849,#35850,#35851,#35852,#35853,#35854,#35855,#35856,#35857,
#35858,#35859,#35860,#35861,#35862,#35863,#35864,#35865,#35866,#35867,#35868,
#35869,#35870,#35871,#35872,#35873,#35874,#35875,#35876,#35877,#35878,#35879,
#35880,#35881,#35882,#35883,#35884,#35885,#35886,#35887,#35888,#35889,#35890,
#35891,#35892,#35893,#35894,#35895),.UNSPECIFIED.,.F.,.F.,(4,2,2,2,2,2,
2,2,2,2,2,2,2,2,2,2,2,2,2,2,2,2,2,2,2,2,2,2,2,2,2,2,2,2,2,2,2,2,2,2,2,2,
2,2,2,2,2,2,2,2,2,2,2,2,2,2,2,2,2,2,2,2,2,2,2,2,2,2,2,2,2,2,2,2,2,2,2,2,
2,2,2,4),(-4.0614287578822,-4.03248871540076,-4.01846104360662,-4.01365489798641,
-4.01033316269565,-4.00752181880818,-4.00452327004274,-4.0007622030692,
-3.99489804196461,-3.96524899606189,-3.94584283611108,-3.88111634163756,
-3.85452293802728,-3.84879489543677,-3.84641168900244,-3.84469933804932,
-3.84309929440734,-3.84039647146944,-3.8331451375629,-3.77212380131558,
-3.72144008924457,-3.70353835756497,-3.69530252279819,-3.68872717556511,
-3.68517352177786,-3.68247422333838,-3.67909297441338,-3.67338468946435,
-3.65345836652772,-3.55643899838608,-3.53774678690756,-3.53064256320669,
-3.52546566485076,-3.52317800715839,-3.52148127783768,-3.5196194663786,
-3.51653417352629,-3.50641678134479,-3.50451420221678,-3.41361908352743,
-3.38615026898234,-3.36936041640254,-3.36420716022018,-3.36094858742808,
-3.35791897603315,-3.35398057099992,-3.34738549014509,-3.29815696099868,
-3.22183041738727,-3.20486364478017,-3.2013533191308,-3.1993975661187,-3.19772002182691,
-3.19559442110385,-3.19141237522778,-3.16388011103469,-3.09076122624934,
-3.06315893043958,-3.04631045962763,-3.04115055523152,-3.03789039483268,
-3.03486111368623,-3.03092570368943,-3.02434129471597,-2.97503329712059,
-2.89858817553595,-2.8817742661767,-2.87827305475125,-2.87631921920786,
-2.87464136090194,-2.87251284295468,-2.86831745264589,-2.84038932807227,
-2.76775598971946,-2.74010440623786,-2.72323413696449,-2.71807163743497,
-2.71481077727113,-2.71178149438938,-2.70784700259689,-2.70126615755269,
-2.69232820337898),.UNSPECIFIED.);
#320=B_SPLINE_CURVE_WITH_KNOTS('',3,(#35897,#35898,#35899,#35900,#35901,
#35902,#35903,#35904,#35905,#35906,#35907,#35908,#35909,#35910,#35911,#35912,
#35913,#35914,#35915,#35916,#35917,#35918,#35919,#35920,#35921,#35922,#35923,
#35924,#35925,#35926,#35927,#35928,#35929,#35930,#35931,#35932,#35933,#35934,
#35935,#35936,#35937,#35938,#35939,#35940,#35941,#35942,#35943,#35944,#35945,
#35946,#35947,#35948,#35949,#35950,#35951,#35952,#35953,#35954),
 .UNSPECIFIED.,.F.,.F.,(4,2,2,2,2,2,2,2,2,2,2,2,2,2,2,2,2,2,2,2,2,2,2,2,
2,2,2,2,4),(-0.510303440387924,-0.468140561817124,-0.462130454299904,-0.437689929728706,
-0.433625192760907,-0.431524767779201,-0.429848909425109,-0.42787393520875,
-0.424275166859475,-0.405758519692253,-0.325536566182482,-0.281740120617086,
-0.275267094480029,-0.271364303988575,-0.268340089133171,-0.265538401924824,
-0.261004058170068,-0.248366526641298,-0.22953730751555,-0.193035807796621,
-0.118118298295534,-0.111729377774037,-0.10916430395282,-0.107590514978991,
-0.105855895048481,-0.103355943930342,-0.096903514059749,-0.0634855304692036,
-0.000963188783679523),.UNSPECIFIED.);
#321=B_SPLINE_CURVE_WITH_KNOTS('',3,(#35957,#35958,#35959,#35960,#35961,
#35962,#35963,#35964,#35965,#35966),.UNSPECIFIED.,.F.,.F.,(4,1,1,1,1,1,
1,4),(-154.889187401721,-153.991685902111,-152.99173988976,-151.991793877409,
-150.991847865057,-149.991901852706,-148.991955840354,-148.606018529037),
 .UNSPECIFIED.);
#322=B_SPLINE_CURVE_WITH_KNOTS('',3,(#36691,#36692,#36693,#36694,#36695,
#36696,#36697,#36698,#36699,#36700,#36701,#36702,#36703,#36704),
 .UNSPECIFIED.,.F.,.F.,(4,2,2,2,2,2,4),(0.00555754112882316,0.130635807126562,
0.266975111939351,0.422108165342909,0.562616294044253,0.663795202990439,
0.760829564106722),.UNSPECIFIED.);
#323=B_SPLINE_CURVE_WITH_KNOTS('',3,(#36705,#36706,#36707,#36708,#36709,
#36710,#36711,#36712,#36713,#36714,#36715,#36716,#36717,#36718),
 .UNSPECIFIED.,.F.,.F.,(4,2,2,2,2,2,4),(0.00715775406190771,0.144210143720968,
0.294872793307161,0.424783240858239,0.547591224239104,0.631024462616706,
0.688336229299088),.UNSPECIFIED.);
#324=B_SPLINE_CURVE_WITH_KNOTS('',3,(#36923,#36924,#36925,#36926),
 .UNSPECIFIED.,.F.,.F.,(4,4),(55.632514020542,55.7635335033061),
 .UNSPECIFIED.);
#325=B_SPLINE_CURVE_WITH_KNOTS('',3,(#36929,#36930,#36931,#36932,#36933),
 .UNSPECIFIED.,.F.,.F.,(4,1,4),(55.6324918109698,55.8152285143725,56.2866044747298),
 .UNSPECIFIED.);
#326=B_SPLINE_CURVE_WITH_KNOTS('',3,(#36939,#36940,#36941,#36942,#36943,
#36944,#36945,#36946,#36947,#36948,#36949,#36950,#36951,#36952,#36953,#36954,
#36955,#36956,#36957,#36958,#36959,#36960,#36961,#36962,#36963,#36964,#36965,
#36966,#36967,#36968,#36969,#36970,#36971,#36972,#36973,#36974,#36975,#36976,
#36977,#36978,#36979,#36980,#36981,#36982,#36983,#36984,#36985,#36986,#36987,
#36988,#36989,#36990,#36991,#36992,#36993,#36994,#36995,#36996,#36997,#36998,
#36999,#37000,#37001,#37002,#37003,#37004,#37005,#37006,#37007,#37008,#37009,
#37010,#37011,#37012,#37013,#37014,#37015,#37016,#37017,#37018,#37019,#37020,
#37021,#37022,#37023,#37024,#37025,#37026,#37027,#37028,#37029,#37030,#37031,
#37032,#37033,#37034,#37035,#37036,#37037,#37038,#37039,#37040,#37041,#37042,
#37043,#37044,#37045,#37046,#37047,#37048,#37049,#37050,#37051,#37052,#37053,
#37054,#37055,#37056,#37057,#37058,#37059,#37060,#37061,#37062,#37063,#37064,
#37065,#37066,#37067,#37068,#37069,#37070,#37071,#37072,#37073,#37074,#37075,
#37076,#37077,#37078,#37079,#37080,#37081,#37082,#37083,#37084,#37085,#37086,
#37087,#37088,#37089,#37090,#37091,#37092,#37093,#37094,#37095,#37096,#37097,
#37098,#37099,#37100,#37101,#37102,#37103,#37104,#37105,#37106,#37107,#37108,
#37109,#37110),.UNSPECIFIED.,.F.,.F.,(4,3,3,3,3,3,3,3,3,3,3,3,3,3,3,3,3,
3,3,3,3,3,3,3,3,3,3,3,3,3,3,3,3,3,3,3,3,3,3,3,3,3,3,3,3,3,3,3,3,3,3,3,3,
3,3,3,3,4),(49.3493405936366,49.4193689479141,49.4893896861999,49.5609427698437,
49.6309674799891,49.7032847503821,49.7756020207751,49.8456426343618,49.9156713518887,
49.9856922954051,50.0579182993003,50.1279429852639,50.201269648125,50.274596310986,
50.3446366811021,50.4146651537395,50.4846858515977,50.5569120389975,50.6269364804616,
50.7002635408293,50.7735906011969,50.8436318783237,50.9136612616073,50.9836828713458,
51.0559083763613,51.1259337214531,51.1992593064304,51.2725848914078,51.3426239524563,
51.4126511125654,51.4826704978761,51.5548976688117,51.6249208138906,51.6982499977546,
51.7715791816187,51.8416224003585,51.9116537285312,51.9816772813509,52.0539013289706,
52.1239285887193,52.1972510302745,52.2705734718297,52.3406109642765,52.4106365581925,
52.4806543837547,52.5528827283262,52.6229043486391,52.6962360553399,52.7695677620406,
52.8396086885631,52.9096377028379,52.9796589263131,53.0518847077977,53.1219096292928,
53.1952358407721,53.2685620522515,53.3417764954199,53.4070751084796),
 .UNSPECIFIED.);
#327=B_SPLINE_CURVE_WITH_KNOTS('',3,(#37111,#37112,#37113,#37114,#37115,
#37116,#37117,#37118),.UNSPECIFIED.,.F.,.F.,(4,1,1,1,1,4),(53.4070751110265,
53.7675563424624,54.2665506326734,54.7655449228843,55.2645392130952,55.632514020542),
 .UNSPECIFIED.);
#328=B_SPLINE_CURVE_WITH_KNOTS('',3,(#37120,#37121,#37122,#37123,#37124,
#37125,#37126,#37127),.UNSPECIFIED.,.F.,.F.,(4,1,1,1,1,4),(53.4070751344278,
53.8192513535288,54.3182456437397,54.8172399339506,55.3162342241615,55.6324918109698),
 .UNSPECIFIED.);
#329=B_SPLINE_CURVE_WITH_KNOTS('',3,(#37128,#37129,#37130,#37131,#37132,
#37133,#37134,#37135,#37136,#37137,#37138,#37139,#37140,#37141,#37142,#37143,
#37144,#37145,#37146,#37147,#37148,#37149,#37150,#37151,#37152,#37153,#37154,
#37155,#37156,#37157,#37158,#37159,#37160,#37161,#37162,#37163,#37164,#37165,
#37166,#37167,#37168,#37169,#37170,#37171,#37172,#37173,#37174,#37175,#37176,
#37177,#37178,#37179,#37180,#37181,#37182,#37183,#37184,#37185,#37186,#37187,
#37188,#37189,#37190,#37191,#37192,#37193,#37194,#37195,#37196,#37197,#37198,
#37199,#37200,#37201,#37202,#37203,#37204,#37205,#37206,#37207,#37208,#37209,
#37210,#37211,#37212,#37213,#37214,#37215,#37216,#37217,#37218,#37219,#37220,
#37221,#37222,#37223,#37224,#37225,#37226,#37227,#37228,#37229,#37230,#37231,
#37232,#37233,#37234,#37235,#37236,#37237,#37238,#37239,#37240,#37241,#37242,
#37243,#37244,#37245,#37246,#37247,#37248,#37249,#37250,#37251,#37252,#37253,
#37254,#37255,#37256,#37257,#37258,#37259,#37260,#37261,#37262,#37263,#37264,
#37265,#37266,#37267,#37268,#37269,#37270,#37271,#37272,#37273,#37274,#37275,
#37276,#37277,#37278,#37279,#37280,#37281,#37282,#37283,#37284,#37285,#37286,
#37287,#37288,#37289,#37290,#37291,#37292,#37293,#37294,#37295,#37296,#37297,
#37298,#37299,#37300,#37301,#37302),.UNSPECIFIED.,.F.,.F.,(4,3,3,3,3,3,
3,3,3,3,3,3,3,3,3,3,3,3,3,3,3,3,3,3,3,3,3,3,3,3,3,3,3,3,3,3,3,3,3,3,3,3,
3,3,3,3,3,3,3,3,3,3,3,3,3,3,3,3,4),(49.3493315211037,49.4193681064343,49.4893940333262,
49.5594134227735,49.6294388812757,49.6994638047524,49.7695045346538,49.8272970318414,
49.8973376266719,49.9673663251347,50.0373872493319,50.109613267512,50.1796379337725,
50.2529646279124,50.3262913220523,50.3963319018199,50.4663605851638,50.5363814942255,
50.6086075237349,50.678632175007,50.7519588936351,50.8252856122632,50.8953262259418,
50.9653549432983,51.0353758863851,51.1076018904074,51.1776265753145,51.2509532388943,
51.3242799024742,51.3943204573068,51.4643491156853,51.5343699998164,51.6065960480335,
51.6766206747678,51.7499474337265,51.8232741926851,51.8933148183004,51.963343547517,
52.0333645023575,52.1055904974922,52.1756151937477,52.2489418383219,52.322268482896,
52.3923090961645,52.4623378133711,52.5323587565658,52.6045847607011,52.674609446344,
52.7479361097254,52.8212627731069,52.8913031445529,52.961331618526,53.0313523177225,
53.1035785041213,53.1736029469128,53.2469300051154,53.3202570633179,53.3951479415614,
53.4070751110265),.UNSPECIFIED.);
#330=B_SPLINE_CURVE_WITH_KNOTS('',3,(#37308,#37309,#37310,#37311,#37312,
#37313,#37314,#37315,#37316,#37317,#37318,#37319,#37320,#37321,#37322,#37323,
#37324,#37325,#37326,#37327,#37328,#37329,#37330,#37331,#37332,#37333,#37334,
#37335,#37336,#37337,#37338,#37339,#37340,#37341,#37342,#37343,#37344,#37345,
#37346,#37347,#37348,#37349,#37350,#37351,#37352,#37353,#37354,#37355,#37356,
#37357,#37358,#37359,#37360,#37361,#37362,#37363,#37364,#37365,#37366,#37367,
#37368,#37369,#37370,#37371,#37372,#37373,#37374,#37375,#37376,#37377,#37378,
#37379,#37380,#37381,#37382,#37383,#37384,#37385,#37386,#37387,#37388,#37389,
#37390,#37391,#37392,#37393,#37394,#37395,#37396,#37397,#37398,#37399,#37400,
#37401,#37402,#37403,#37404,#37405,#37406,#37407,#37408,#37409,#37410,#37411,
#37412,#37413,#37414,#37415,#37416,#37417,#37418,#37419,#37420,#37421,#37422,
#37423,#37424,#37425,#37426,#37427,#37428,#37429,#37430,#37431,#37432,#37433,
#37434,#37435,#37436,#37437,#37438,#37439,#37440,#37441,#37442,#37443,#37444,
#37445,#37446,#37447,#37448,#37449,#37450,#37451,#37452,#37453,#37454,#37455,
#37456,#37457,#37458,#37459,#37460,#37461,#37462,#37463,#37464,#37465,#37466,
#37467,#37468,#37469,#37470,#37471,#37472,#37473,#37474,#37475,#37476,#37477,
#37478,#37479,#37480,#37481,#37482),.UNSPECIFIED.,.F.,.F.,(4,3,3,3,3,3,
3,3,3,3,3,3,3,3,3,3,3,3,3,3,3,3,3,3,3,3,3,3,3,3,3,3,3,3,3,3,3,3,3,3,3,3,
3,3,3,3,3,3,3,3,3,3,3,3,3,3,3,3,4),(43.0661349437165,43.1361595852945,43.2061863657319,
43.2762263384948,43.2886762480331,43.3587168388614,43.4287455333042,43.4987664534742,
43.5709924746666,43.6410171369318,43.7143438375879,43.787670538244,43.8577111290883,
43.9277398235473,43.9977607437335,44.0699867649139,44.1400114271953,44.2133381278251,
44.2866648284549,44.356705419211,44.426734113581,44.4967550336782,44.5689810549251,
44.6390057171185,44.7123324178922,44.7856591186658,44.8556997096685,44.9257284042863,
44.9957493246315,45.0679753456928,45.1380000081315,45.2113267085041,45.2846534088767,
45.3546939993659,45.4247226934689,45.4947436132985,45.5669696347458,45.6369942966754,
45.7103209978815,45.7836476990877,45.8536882903938,45.9237169853148,45.9937379059628,
46.0659639267968,46.1359885895326,46.2093152894156,46.2826419892986,46.3526825797948,
46.4227112739064,46.4927321937468,46.5649582151875,46.6349828771319,46.7083095783207,
46.7816362795095,46.8516132827516,46.9215804164053,46.9915381364908,47.0614983061719,
47.1238898038469),.UNSPECIFIED.);
#331=B_SPLINE_CURVE_WITH_KNOTS('',3,(#37483,#37484,#37485,#37486,#37487,
#37488,#37489,#37490,#37491,#37492,#37493,#37494,#37495,#37496,#37497,#37498,
#37499,#37500,#37501,#37502,#37503,#37504,#37505,#37506,#37507,#37508,#37509,
#37510,#37511,#37512,#37513,#37514,#37515,#37516,#37517,#37518,#37519,#37520,
#37521,#37522,#37523,#37524,#37525,#37526,#37527,#37528,#37529,#37530,#37531,
#37532,#37533,#37534,#37535,#37536,#37537,#37538,#37539,#37540,#37541,#37542,
#37543,#37544,#37545,#37546,#37547,#37548,#37549,#37550,#37551,#37552,#37553,
#37554,#37555,#37556,#37557,#37558,#37559,#37560,#37561,#37562,#37563,#37564,
#37565,#37566,#37567,#37568,#37569,#37570,#37571,#37572,#37573,#37574,#37575,
#37576,#37577,#37578,#37579),.UNSPECIFIED.,.F.,.F.,(4,3,3,3,3,3,3,3,3,3,
3,3,3,3,3,3,3,3,3,3,3,3,3,3,3,3,3,3,3,3,3,3,4),(47.1238898039153,47.1966069931218,
47.269346291875,47.2806305697204,47.3506711645816,47.4206998630754,47.4907207873035,
47.5629468054605,47.6329714717519,47.7062981658417,47.7796248599314,47.8496654396268,
47.919694122898,47.9897150318869,48.0619410614508,48.1319657126511,48.2052924313967,
48.2786191501423,48.3486597639494,48.4186884814349,48.4887094246505,48.5609354285762,
48.6309601136108,48.704286776982,48.7776134403532,48.8476539950211,48.9176826532346,
48.987703537201,49.0599295855418,49.1299542121136,49.2032809713389,49.2766077305641,
49.3493405936366),.UNSPECIFIED.);
#332=B_SPLINE_CURVE_WITH_KNOTS('',3,(#37581,#37582,#37583,#37584,#37585,
#37586,#37587,#37588,#37589,#37590,#37591,#37592,#37593,#37594,#37595,#37596,
#37597,#37598,#37599,#37600,#37601,#37602,#37603,#37604,#37605,#37606,#37607,
#37608,#37609,#37610,#37611,#37612,#37613,#37614,#37615,#37616,#37617,#37618,
#37619,#37620,#37621,#37622,#37623,#37624,#37625,#37626,#37627,#37628,#37629,
#37630,#37631,#37632,#37633,#37634,#37635,#37636,#37637,#37638,#37639,#37640,
#37641,#37642,#37643,#37644,#37645,#37646,#37647,#37648,#37649,#37650,#37651,
#37652,#37653,#37654,#37655,#37656,#37657,#37658,#37659,#37660,#37661,#37662,
#37663,#37664,#37665,#37666,#37667,#37668,#37669,#37670,#37671,#37672,#37673,
#37674,#37675,#37676,#37677),.UNSPECIFIED.,.F.,.F.,(4,3,3,3,3,3,3,3,3,3,
3,3,3,3,3,3,3,3,3,3,3,3,3,3,3,3,3,3,3,3,3,3,4),(47.1238898039108,47.1954657532806,
47.2670653523193,47.3323255807868,47.4023661717881,47.4723948664045,47.5424157867478,
47.6146418078103,47.6846664702475,47.7579931706226,47.8313198709977,47.9013604614893,
47.9713891555945,48.0414100754268,48.1136360968722,48.1836607588042,48.2569874600064,
48.3303141612086,48.4003547525115,48.4703834474297,48.5404043680745,48.6126303889108,
48.6826550516439,48.7559817515317,48.8293084514195,48.8993490419166,48.9693777360291,
49.0393986558705,49.1116246773105,49.1816493392556,49.2549760404431,49.3283027416305,
49.3493315211037),.UNSPECIFIED.);
#333=B_SPLINE_CURVE_WITH_KNOTS('',3,(#37678,#37679,#37680,#37681,#37682,
#37683,#37684,#37685,#37686,#37687,#37688,#37689,#37690,#37691,#37692,#37693,
#37694,#37695,#37696,#37697,#37698,#37699,#37700,#37701,#37702,#37703,#37704,
#37705,#37706,#37707,#37708,#37709,#37710,#37711,#37712,#37713,#37714,#37715,
#37716,#37717,#37718,#37719,#37720,#37721,#37722,#37723,#37724,#37725,#37726,
#37727,#37728,#37729,#37730,#37731,#37732,#37733,#37734,#37735,#37736,#37737,
#37738,#37739,#37740,#37741,#37742,#37743,#37744,#37745,#37746,#37747,#37748,
#37749,#37750,#37751,#37752,#37753,#37754,#37755,#37756,#37757,#37758,#37759,
#37760,#37761,#37762,#37763,#37764,#37765,#37766,#37767,#37768,#37769,#37770,
#37771,#37772,#37773,#37774,#37775,#37776,#37777,#37778,#37779,#37780,#37781,
#37782,#37783,#37784,#37785,#37786,#37787,#37788,#37789,#37790,#37791,#37792,
#37793,#37794,#37795,#37796,#37797,#37798,#37799,#37800,#37801,#37802,#37803,
#37804,#37805,#37806,#37807,#37808,#37809,#37810,#37811,#37812,#37813,#37814,
#37815,#37816,#37817,#37818,#37819,#37820,#37821,#37822,#37823,#37824,#37825,
#37826,#37827,#37828,#37829,#37830,#37831,#37832,#37833,#37834,#37835,#37836,
#37837,#37838,#37839,#37840,#37841,#37842,#37843,#37844,#37845,#37846,#37847,
#37848,#37849),.UNSPECIFIED.,.F.,.F.,(4,3,3,3,3,3,3,3,3,3,3,3,3,3,3,3,3,
3,3,3,3,3,3,3,3,3,3,3,3,3,3,3,3,3,3,3,3,3,3,3,3,3,3,3,3,3,3,3,3,3,3,3,3,
3,3,3,3,4),(43.0661440137509,43.1361697254765,43.2061945280937,43.2762355868376,
43.3403712590994,43.4104118499255,43.4804405443662,43.550461464534,43.6226874857281,
43.6927121479913,43.7660388486508,43.8393655493103,43.909406140138,43.9794348345803,
44.0494557547496,44.1216817759425,44.1917064382073,44.2650331388643,44.3383598395212,
44.408400430345,44.4784291247834,44.5484500449487,44.6206760661446,44.6907007284056,
44.7640274290689,44.8373541297322,44.9073947205635,44.9774234150094,45.0474443351824,
45.1196703563726,45.1896950186409,45.263021719292,45.3363484199431,45.4063890107635,
45.4764177051986,45.5464386253606,45.618664646559,45.6886893088167,45.7620160094854,
45.835342710154,45.9053833009824,45.9754119954253,46.0454329155953,46.1176589367877,
46.187683599053,46.2610102997089,46.3343370003649,46.4043775912091,46.4744062856679,
46.544427205854,46.6166532270345,46.6866778893158,46.7600045899459,46.8333312905759,
46.9059709188937,46.9763616597276,47.0501257317873,47.1238898038469),
 .UNSPECIFIED.);
#334=B_SPLINE_CURVE_WITH_KNOTS('',3,(#37855,#37856,#37857,#37858,#37859,
#37860,#37861,#37862,#37863,#37864,#37865,#37866,#37867),.UNSPECIFIED.,
 .F.,.F.,(4,1,1,1,1,1,1,1,1,1,4),(36.7829477512195,36.8017504752911,37.300744765502,
37.7997390557129,38.2987333459238,38.7977276361348,39.2967219263457,39.7957162165566,
40.2947105067675,40.7937047969784,40.8407044966673),.UNSPECIFIED.);
#335=B_SPLINE_CURVE_WITH_KNOTS('',3,(#37868,#37869,#37870,#37871,#37872,
#37873,#37874,#37875,#37876,#37877,#37878,#37879,#37880,#37881,#37882,#37883,
#37884,#37885,#37886,#37887,#37888,#37889,#37890,#37891,#37892,#37893,#37894,
#37895,#37896,#37897,#37898,#37899,#37900,#37901,#37902,#37903,#37904,#37905,
#37906,#37907,#37908,#37909,#37910,#37911,#37912,#37913,#37914,#37915,#37916,
#37917,#37918,#37919,#37920,#37921,#37922,#37923,#37924,#37925,#37926,#37927,
#37928,#37929,#37930,#37931,#37932,#37933,#37934,#37935,#37936,#37937,#37938,
#37939,#37940,#37941,#37942,#37943,#37944,#37945,#37946,#37947,#37948,#37949,
#37950,#37951,#37952,#37953,#37954,#37955,#37956,#37957,#37958,#37959,#37960,
#37961,#37962,#37963,#37964),.UNSPECIFIED.,.F.,.F.,(4,3,3,3,3,3,3,3,3,3,
3,3,3,3,3,3,3,3,3,3,3,3,3,3,3,3,3,3,3,3,3,3,4),(40.8407044966673,40.910513107026,
40.9803103162599,41.050100831576,41.1198969722149,41.1896937756429,41.2595054868552,
41.2926990871894,41.3627396780171,41.4327683724595,41.5027892926283,41.5750153138213,
41.645039976086,41.7183666767432,41.7916933774003,41.861733968224,41.9317626626622,
42.0017835828273,42.0740096040233,42.1440342662842,42.2173609669477,42.2906876676112,
42.3607282584425,42.4307569528884,42.500777873061,42.5730038942513,42.6430285565196,
42.7163552571708,42.7896819578221,42.859723254519,42.9297517388031,42.9997772294764,
43.0661349437165),.UNSPECIFIED.);
#336=B_SPLINE_CURVE_WITH_KNOTS('',3,(#37966,#37967,#37968,#37969,#37970,
#37971,#37972,#37973,#37974,#37975,#37976,#37977,#37978,#37979,#37980,#37981,
#37982,#37983,#37984,#37985,#37986,#37987,#37988,#37989,#37990,#37991,#37992,
#37993,#37994,#37995,#37996,#37997,#37998,#37999,#38000,#38001,#38002,#38003,
#38004,#38005,#38006,#38007,#38008,#38009,#38010,#38011,#38012,#38013,#38014,
#38015,#38016,#38017,#38018,#38019,#38020,#38021,#38022,#38023,#38024,#38025,
#38026,#38027,#38028,#38029,#38030,#38031,#38032,#38033,#38034,#38035,#38036,
#38037,#38038,#38039,#38040,#38041,#38042,#38043,#38044,#38045,#38046,#38047,
#38048,#38049,#38050,#38051,#38052,#38053,#38054,#38055,#38056,#38057,#38058,
#38059,#38060,#38061,#38062,#38063,#38064,#38065),.UNSPECIFIED.,.F.,.F.,
(4,3,3,3,3,3,3,3,3,3,3,3,3,3,3,3,3,3,3,3,3,3,3,3,3,3,3,3,3,3,3,3,3,4),(40.8407044966673,
40.8453998080448,40.9154403988712,40.9854690933122,41.0554900134805,41.1277160346743,
41.1977406969378,41.2710673975968,41.3443940982557,41.4144346890823,41.4844633835235,
41.5544843036917,41.6267103248854,41.6967349871492,41.7700616878079,41.8433883884666,
41.913428979293,41.9834576737341,42.0534785939022,42.1257046150961,42.1957292773597,
42.2690559780186,42.3423826786776,42.4124232695042,42.4824519639455,42.5524728841137,
42.6246989053074,42.6947235675711,42.7680502682298,42.8413769688885,42.9114171285507,
42.981444789593,43.051465392962,43.0661440137509),.UNSPECIFIED.);
#337=B_SPLINE_CURVE_WITH_KNOTS('',3,(#38066,#38067,#38068,#38069,#38070,
#38071,#38072,#38073,#38074,#38075,#38076,#38077,#38078,#38079,#38080,#38081,
#38082,#38083,#38084,#38085,#38086,#38087,#38088,#38089,#38090,#38091,#38092,
#38093,#38094,#38095,#38096,#38097,#38098,#38099,#38100,#38101,#38102,#38103,
#38104,#38105,#38106,#38107,#38108,#38109,#38110,#38111,#38112,#38113,#38114,
#38115,#38116,#38117,#38118,#38119,#38120,#38121,#38122,#38123,#38124,#38125,
#38126,#38127,#38128,#38129,#38130,#38131,#38132,#38133,#38134,#38135,#38136,
#38137,#38138,#38139,#38140,#38141,#38142,#38143,#38144,#38145,#38146,#38147,
#38148,#38149,#38150,#38151,#38152,#38153,#38154,#38155,#38156,#38157,#38158,
#38159,#38160,#38161,#38162,#38163,#38164,#38165,#38166,#38167,#38168,#38169,
#38170,#38171,#38172,#38173,#38174,#38175,#38176,#38177,#38178,#38179,#38180,
#38181,#38182,#38183,#38184,#38185,#38186,#38187,#38188,#38189,#38190,#38191,
#38192,#38193,#38194,#38195,#38196,#38197,#38198,#38199,#38200,#38201,#38202,
#38203,#38204,#38205,#38206,#38207,#38208,#38209,#38210,#38211,#38212,#38213,
#38214,#38215,#38216,#38217,#38218,#38219,#38220,#38221,#38222,#38223,#38224,
#38225,#38226,#38227,#38228,#38229,#38230,#38231,#38232,#38233,#38234,#38235,
#38236,#38237),.UNSPECIFIED.,.F.,.F.,(4,3,3,3,3,3,3,3,3,3,3,3,3,3,3,3,3,
3,3,3,3,3,3,3,3,3,3,3,3,3,3,3,3,3,3,3,3,3,3,3,3,3,3,3,3,3,3,3,3,3,3,3,3,
3,3,3,3,4),(36.7829389522053,36.8534454863574,36.9234860771838,36.993514771625,
37.0635356917935,37.1357617129872,37.2057863752507,37.2791130759095,37.3524397765683,
37.4224803673948,37.4925090618357,37.5625299820039,37.6347560031977,37.7047806654614,
37.7781073661203,37.8514340667792,37.9214746576057,37.9915033520468,38.0615242722151,
38.1337502934089,38.2037749556726,38.2771016563314,38.3504283569902,38.4204689478168,
38.4904976422578,38.5605185624258,38.6327445836196,38.7027692458831,38.7760959465421,
38.8494226472011,38.9194632380276,38.9894919324685,39.0595128526359,39.1317388738299,
39.2017635360937,39.2750902367529,39.348416937412,39.4184575282385,39.4884862226793,
39.5585071428479,39.6307331640416,39.7007578263054,39.7740845269641,39.8474112276229,
39.9174518184494,39.9874805128906,40.0575014330589,40.1297274542526,40.1997521165164,
40.2730788171751,40.3464055178339,40.4164150422325,40.4864125754172,40.5564023218123,
40.6274778655123,40.6974714282655,40.7690879624389,40.8407044966123),
 .UNSPECIFIED.);
#338=B_SPLINE_CURVE_WITH_KNOTS('',3,(#38243,#38244,#38245,#38246,#38247,
#38248,#38249,#38250,#38251,#38252,#38253,#38254,#38255,#38256,#38257,#38258,
#38259,#38260,#38261,#38262,#38263,#38264,#38265,#38266,#38267,#38268,#38269,
#38270,#38271,#38272,#38273,#38274,#38275,#38276,#38277,#38278,#38279,#38280,
#38281,#38282,#38283,#38284,#38285,#38286,#38287,#38288,#38289,#38290,#38291,
#38292,#38293,#38294,#38295,#38296,#38297,#38298,#38299,#38300,#38301,#38302,
#38303,#38304,#38305,#38306,#38307,#38308,#38309,#38310,#38311,#38312,#38313,
#38314,#38315,#38316,#38317,#38318,#38319,#38320,#38321,#38322,#38323,#38324,
#38325,#38326,#38327,#38328,#38329,#38330,#38331,#38332,#38333,#38334,#38335,
#38336,#38337,#38338,#38339,#38340,#38341,#38342,#38343,#38344,#38345,#38346,
#38347,#38348,#38349,#38350,#38351,#38352,#38353,#38354,#38355,#38356,#38357,
#38358,#38359,#38360,#38361,#38362,#38363,#38364,#38365,#38366,#38367,#38368,
#38369,#38370,#38371,#38372,#38373,#38374,#38375,#38376,#38377,#38378,#38379,
#38380,#38381,#38382,#38383,#38384,#38385,#38386,#38387,#38388,#38389,#38390,
#38391,#38392,#38393,#38394,#38395,#38396,#38397,#38398,#38399,#38400,#38401,
#38402,#38403,#38404,#38405,#38406,#38407,#38408,#38409,#38410,#38411,#38412,
#38413,#38414,#38415,#38416,#38417),.UNSPECIFIED.,.F.,.F.,(4,3,3,3,3,3,
3,3,3,3,3,3,3,3,3,3,3,3,3,3,3,3,3,3,3,3,3,3,3,3,3,3,3,3,3,3,3,3,3,3,3,3,
3,3,3,3,3,3,3,3,3,3,3,3,3,3,3,3,4),(30.4997797388357,30.5697978420759,30.6398226552016,
30.7098483404733,30.7798883251637,30.81381899276,30.8838595835864,30.9538882780275,
31.0239091981955,31.0961352193893,31.166159881653,31.2394865823119,31.3128132829709,
31.3828538737974,31.4528825682385,31.5229034884066,31.5951295096004,31.6651541718641,
31.7384808725229,31.8118075731818,31.8818481640083,31.9518768584493,32.0218977786175,
32.0941237998113,32.164148462075,32.2374751627339,32.3108018633928,32.3808424542193,
32.4508711486604,32.5208920688285,32.5931180900223,32.6631427522861,32.7364694529449,
32.8097961536037,32.8798367444301,32.9498654388712,33.0198863590392,33.0921123802331,
33.1621370424967,33.2354637431556,33.3087904438146,33.378831034641,33.4488597290821,
33.5188806492501,33.5911066704439,33.6611313327075,33.7344580333665,33.8077847340255,
33.877825324852,33.9478540192931,34.0178749394612,34.090100960655,34.1601256229187,
34.2334523235775,34.3067790242364,34.3776775785114,34.4485623759747,34.5194352520091,
34.5575191894138),.UNSPECIFIED.);
#339=B_SPLINE_CURVE_WITH_KNOTS('',3,(#38418,#38419,#38420,#38421,#38422,
#38423,#38424,#38425),.UNSPECIFIED.,.F.,.F.,(4,1,1,1,1,4),(34.5575191894877,
34.8057733144474,35.3047676046583,35.8037618948692,36.3027561850801,36.7829477512195),
 .UNSPECIFIED.);
#340=B_SPLINE_CURVE_WITH_KNOTS('',3,(#38427,#38428,#38429,#38430,#38431,
#38432,#38433,#38434,#38435,#38436,#38437,#38438,#38439,#38440,#38441,#38442,
#38443,#38444,#38445,#38446,#38447,#38448,#38449,#38450,#38451,#38452,#38453,
#38454,#38455,#38456,#38457,#38458,#38459,#38460,#38461,#38462,#38463,#38464,
#38465,#38466,#38467,#38468,#38469,#38470,#38471,#38472,#38473,#38474,#38475,
#38476,#38477,#38478,#38479,#38480,#38481,#38482,#38483,#38484,#38485,#38486,
#38487,#38488,#38489,#38490,#38491,#38492,#38493,#38494,#38495,#38496,#38497,
#38498,#38499,#38500,#38501,#38502,#38503,#38504,#38505,#38506,#38507,#38508,
#38509,#38510,#38511,#38512,#38513,#38514,#38515,#38516,#38517,#38518,#38519,
#38520,#38521,#38522,#38523),.UNSPECIFIED.,.F.,.F.,(4,3,3,3,3,3,3,3,3,3,
3,3,3,3,3,3,3,3,3,3,3,3,3,3,3,3,3,3,3,3,3,3,4),(34.5575191894877,34.6277996055737,
34.6980904637057,34.7683845128919,34.8386929125139,34.8574683255137,34.9275089163402,
34.9975376107813,35.0675585309494,35.1397845521432,35.2098092144068,35.2831359150657,
35.3564626157246,35.4265032065511,35.4965319009923,35.5665528211606,35.6387788423543,
35.7088035046181,35.7821302052769,35.8554569059356,35.9254974967621,35.9955261912031,
36.0655471113711,36.1377731325649,36.2077977948286,36.2811244954875,36.3544511961465,
36.4244912351492,36.4945191737348,36.5666241183524,36.6366450905632,36.7097920213842,
36.7829389522053),.UNSPECIFIED.);
#341=B_SPLINE_CURVE_WITH_KNOTS('',3,(#38524,#38525,#38526,#38527,#38528,
#38529,#38530,#38531,#38532,#38533,#38534,#38535,#38536,#38537,#38538,#38539,
#38540,#38541,#38542,#38543,#38544,#38545,#38546,#38547,#38548,#38549,#38550,
#38551,#38552,#38553,#38554,#38555,#38556,#38557,#38558,#38559,#38560,#38561,
#38562,#38563,#38564,#38565,#38566,#38567,#38568,#38569,#38570,#38571,#38572,
#38573,#38574,#38575,#38576,#38577,#38578,#38579,#38580,#38581,#38582,#38583,
#38584,#38585,#38586,#38587,#38588,#38589,#38590,#38591,#38592,#38593,#38594,
#38595,#38596,#38597,#38598,#38599,#38600,#38601,#38602,#38603,#38604,#38605,
#38606,#38607,#38608,#38609,#38610,#38611,#38612,#38613,#38614,#38615,#38616,
#38617,#38618,#38619,#38620,#38621,#38622,#38623,#38624,#38625,#38626,#38627,
#38628,#38629,#38630,#38631,#38632,#38633,#38634,#38635,#38636,#38637,#38638,
#38639,#38640,#38641,#38642,#38643,#38644,#38645,#38646,#38647,#38648,#38649,
#38650,#38651,#38652,#38653,#38654,#38655,#38656,#38657,#38658,#38659,#38660,
#38661,#38662,#38663,#38664,#38665,#38666,#38667,#38668,#38669,#38670,#38671,
#38672,#38673,#38674,#38675,#38676,#38677,#38678,#38679,#38680,#38681,#38682,
#38683,#38684,#38685,#38686,#38687,#38688,#38689,#38690,#38691,#38692,#38693,
#38694,#38695,#38696,#38697,#38698),.UNSPECIFIED.,.F.,.F.,(4,3,3,3,3,3,
3,3,3,3,3,3,3,3,3,3,3,3,3,3,3,3,3,3,3,3,3,3,3,3,3,3,3,3,3,3,3,3,3,3,3,3,
3,3,3,3,3,3,3,3,3,3,3,3,3,3,3,3,4),(30.4997851996723,30.5698066945125,30.6398241339171,
30.7098487763432,30.7798753719464,30.8499153073756,30.8655140038263,30.9355545946528,
31.0055832890939,31.0756042092621,31.1478302304559,31.2178548927196,31.2911815933785,
31.3645082940373,31.4345488848638,31.5045775793049,31.574598499473,31.6468245206668,
31.7168491829305,31.7901758835893,31.8635025842482,31.9335431750747,32.0035718695158,
32.0735927896839,32.1458188108777,32.2158434731413,32.2891701738002,32.3624968744591,
32.4325374652855,32.5025661597266,32.5725870798947,32.6448131010885,32.7148377633521,
32.788164464011,32.86149116467,32.9315317554965,33.0015604499375,33.0715813701056,
33.1438073912994,33.2138320535631,33.287158754222,33.3604854548809,33.4305260457074,
33.5005547401485,33.5705756603166,33.6428016815104,33.712826343774,33.786153044433,
33.8594797450919,33.9295203359184,33.9995490303595,34.0695699505274,34.1417959717213,
34.211820633985,34.2851473346439,34.3584740353028,34.4302564390369,34.5020210945599,
34.557519189415),.UNSPECIFIED.);
#342=B_SPLINE_CURVE_WITH_KNOTS('',3,(#38704,#38705,#38706,#38707,#38708,
#38709,#38710,#38711,#38712,#38713,#38714,#38715,#38716,#38717,#38718,#38719,
#38720,#38721,#38722,#38723,#38724,#38725,#38726,#38727,#38728,#38729,#38730,
#38731,#38732,#38733,#38734,#38735,#38736,#38737,#38738,#38739,#38740,#38741,
#38742,#38743,#38744,#38745,#38746,#38747,#38748,#38749,#38750,#38751,#38752,
#38753,#38754,#38755,#38756,#38757,#38758,#38759,#38760,#38761,#38762,#38763,
#38764,#38765,#38766,#38767,#38768,#38769,#38770,#38771,#38772,#38773,#38774,
#38775,#38776,#38777,#38778,#38779,#38780,#38781,#38782,#38783,#38784,#38785,
#38786,#38787,#38788,#38789,#38790,#38791,#38792,#38793,#38794,#38795,#38796,
#38797,#38798,#38799,#38800,#38801,#38802,#38803,#38804,#38805,#38806,#38807,
#38808,#38809,#38810,#38811,#38812,#38813,#38814,#38815,#38816,#38817,#38818,
#38819,#38820,#38821,#38822,#38823,#38824,#38825,#38826,#38827,#38828,#38829,
#38830,#38831,#38832,#38833,#38834,#38835,#38836,#38837,#38838,#38839,#38840,
#38841,#38842,#38843,#38844,#38845,#38846,#38847,#38848,#38849,#38850,#38851,
#38852,#38853,#38854,#38855,#38856,#38857,#38858,#38859,#38860,#38861,#38862,
#38863,#38864,#38865,#38866,#38867,#38868,#38869,#38870,#38871,#38872,#38873,
#38874,#38875,#38876,#38877,#38878),.UNSPECIFIED.,.F.,.F.,(4,3,3,3,3,3,
3,3,3,3,3,3,3,3,3,3,3,3,3,3,3,3,3,3,3,3,3,3,3,3,3,3,3,3,3,3,3,3,3,3,3,3,
3,3,3,3,3,3,3,3,3,3,3,3,3,3,3,3,4),(24.216566741472,24.2866068494992,24.326893220018,
24.3969338108387,24.4669625052738,24.5369834254368,24.6092094466348,24.6792341088923,
24.7525608095606,24.8258875102289,24.8959281010602,24.9659567955063,25.0359777156793,
25.1082037368695,25.1782283991379,25.2515550997889,25.3248818004398,25.3949223912636,
25.4649510857019,25.5349720058675,25.6071980270633,25.6772226893242,25.7505493899875,
25.8238760906508,25.8939166814786,25.963945375921,26.0339662960902,26.106192317283,
26.1762169795479,26.2495436802048,26.3228703808617,26.3929109716879,26.4629396661284,
26.5329605862962,26.6051866074903,26.6752112697534,26.748537970413,26.8218646710726,
26.8919052618991,26.9619339563401,27.031954876509,27.1041808977026,27.1742055599662,
27.2475322606249,27.3208589612835,27.3908995521103,27.4609282465518,27.5309491667197,
27.6031751879134,27.6731998501771,27.7465265508357,27.8198532514944,27.8896727070108,
27.9594796023928,28.0292786272708,28.0990816217299,28.1688842155913,28.238700456284,
28.2743338822293),.UNSPECIFIED.);
#343=B_SPLINE_CURVE_WITH_KNOTS('',3,(#38879,#38880,#38881,#38882,#38883,
#38884,#38885,#38886,#38887,#38888,#38889,#38890,#38891,#38892,#38893,#38894,
#38895,#38896,#38897,#38898,#38899,#38900,#38901,#38902,#38903,#38904,#38905,
#38906,#38907,#38908,#38909,#38910,#38911,#38912,#38913,#38914,#38915,#38916,
#38917,#38918,#38919,#38920,#38921,#38922,#38923,#38924,#38925,#38926,#38927,
#38928,#38929,#38930,#38931,#38932,#38933,#38934,#38935,#38936,#38937,#38938,
#38939,#38940,#38941,#38942,#38943,#38944,#38945,#38946,#38947,#38948,#38949,
#38950,#38951,#38952,#38953,#38954,#38955,#38956,#38957,#38958,#38959,#38960,
#38961,#38962,#38963,#38964,#38965,#38966,#38967,#38968,#38969,#38970,#38971,
#38972,#38973,#38974,#38975),.UNSPECIFIED.,.F.,.F.,(4,3,3,3,3,3,3,3,3,3,
3,3,3,3,3,3,3,3,3,3,3,3,3,3,3,3,3,3,3,3,3,3,4),(28.2743338823081,28.3188475417054,
28.3888881325318,28.4589168269729,28.5289377471412,28.601163768335,28.6711884305987,
28.7445151312575,28.8178418319163,28.8878824227428,28.9579111171838,29.0279320373515,
29.1001580585454,29.170182720809,29.2435094214681,29.3168361221272,29.3868767129537,
29.4569054073949,29.526926327563,29.5991523487568,29.6691770110205,29.7425037116793,
29.8158304123381,29.8858710031646,29.9558996976058,30.025920617774,30.0981466389678,
30.1681713012315,30.2414980018903,30.3148247025491,30.3848646031318,30.4548937584111,
30.4997797388357),.UNSPECIFIED.);
#344=B_SPLINE_CURVE_WITH_KNOTS('',3,(#38977,#38978,#38979,#38980,#38981,
#38982,#38983,#38984,#38985,#38986,#38987,#38988,#38989,#38990,#38991,#38992,
#38993,#38994,#38995,#38996,#38997,#38998,#38999,#39000,#39001,#39002,#39003,
#39004,#39005,#39006,#39007,#39008,#39009,#39010,#39011,#39012,#39013,#39014,
#39015,#39016,#39017,#39018,#39019,#39020,#39021,#39022,#39023,#39024,#39025,
#39026,#39027,#39028,#39029,#39030,#39031,#39032,#39033,#39034,#39035,#39036,
#39037,#39038,#39039,#39040,#39041,#39042,#39043,#39044,#39045,#39046,#39047,
#39048,#39049,#39050,#39051,#39052,#39053,#39054,#39055,#39056,#39057,#39058,
#39059,#39060,#39061,#39062,#39063,#39064,#39065,#39066,#39067,#39068,#39069,
#39070,#39071,#39072,#39073),.UNSPECIFIED.,.F.,.F.,(4,3,3,3,3,3,3,3,3,3,
3,3,3,3,3,3,3,3,3,3,3,3,3,3,3,3,3,3,3,3,3,3,4),(28.2743338823081,28.3488858316158,
28.3705425527717,28.4405831435994,28.5106118380417,28.5806327582111,28.652858779404,
28.7228834416689,28.7962101423258,28.8695368429826,28.9395774338088,29.0096061282494,
29.0796270484171,29.1518530696112,29.2218777318745,29.295204432534,29.3685311331936,
29.4385717240202,29.5086004184613,29.5786213386295,29.6508473598232,29.7208720220869,
29.7941987227457,29.8675254234045,29.937566014231,30.0075947086721,30.0776156288402,
30.149841650034,30.2198663122976,30.2931930129565,30.3665197136154,30.4365607218776,
30.4997851996723),.UNSPECIFIED.);
#345=B_SPLINE_CURVE_WITH_KNOTS('',3,(#39074,#39075,#39076,#39077,#39078,
#39079,#39080,#39081,#39082,#39083,#39084,#39085,#39086,#39087,#39088,#39089,
#39090,#39091,#39092,#39093,#39094,#39095,#39096,#39097,#39098,#39099,#39100,
#39101,#39102,#39103,#39104,#39105,#39106,#39107,#39108,#39109,#39110,#39111,
#39112,#39113,#39114,#39115,#39116,#39117,#39118,#39119,#39120,#39121,#39122,
#39123,#39124,#39125,#39126,#39127,#39128,#39129,#39130,#39131,#39132,#39133,
#39134,#39135,#39136,#39137,#39138,#39139,#39140,#39141,#39142,#39143,#39144,
#39145,#39146,#39147,#39148,#39149,#39150,#39151,#39152,#39153,#39154,#39155,
#39156,#39157,#39158,#39159,#39160,#39161,#39162,#39163,#39164,#39165,#39166,
#39167,#39168,#39169,#39170,#39171,#39172,#39173,#39174,#39175,#39176,#39177,
#39178,#39179,#39180,#39181,#39182,#39183,#39184,#39185,#39186,#39187,#39188,
#39189,#39190,#39191,#39192,#39193,#39194,#39195,#39196,#39197,#39198,#39199,
#39200,#39201,#39202,#39203,#39204,#39205,#39206,#39207,#39208,#39209,#39210,
#39211,#39212,#39213,#39214,#39215,#39216,#39217,#39218,#39219,#39220,#39221,
#39222,#39223,#39224,#39225,#39226,#39227,#39228,#39229,#39230,#39231,#39232,
#39233,#39234,#39235,#39236,#39237,#39238,#39239,#39240,#39241,#39242,#39243,
#39244,#39245,#39246,#39247,#39248),.UNSPECIFIED.,.F.,.F.,(4,3,3,3,3,3,
3,3,3,3,3,3,3,3,3,3,3,3,3,3,3,3,3,3,3,3,3,3,3,3,3,3,3,3,3,3,3,3,3,3,3,3,
3,3,3,3,3,3,3,3,3,3,3,3,3,3,3,3,4),(24.2165701374682,24.2865963860171,24.356636287462,
24.3785882310843,24.4486288215852,24.5186575156965,24.5886784355325,24.6609044569732,
24.7309291189008,24.804255820098,24.8775825212953,24.9476231122925,25.0176518069063,
25.0876727272481,25.1598987483126,25.2299234107518,25.303250111129,25.3765768115062,
25.4466174022641,25.5166460966359,25.5866670167347,25.6588930379803,25.7289177001737,
25.8022444009454,25.8755711017171,25.9456116925611,26.0156403870197,26.0856613072058,
26.1578873283863,26.2279119906679,26.3012386912979,26.374565391928,26.4446059827562,
26.5146346771987,26.5846555973683,26.6568816185609,26.7269062808266,26.8002329814827,
26.8735596821389,26.9436002729597,27.0136289673946,27.0836498875575,27.1558759087556,
27.2259005710137,27.2992272716818,27.3725539723499,27.4425945631809,27.5126232576271,
27.5826441778001,27.6548701989903,27.7248948612584,27.7982215619096,27.8715482625608,
27.9413131725913,28.0110652143382,28.0808150034561,28.1505602216933,28.2203156472821,
28.2743338822406),.UNSPECIFIED.);
#346=B_SPLINE_CURVE_WITH_KNOTS('',3,(#39254,#39255,#39256,#39257,#39258,
#39259,#39260,#39261,#39262),.UNSPECIFIED.,.F.,.F.,(4,1,1,1,1,1,4),(15.7079632679489,
15.8956852974986,16.3946795877096,16.8936738779205,17.3926681681314,17.8916624583423,
17.9334121841373),.UNSPECIFIED.);
#347=B_SPLINE_CURVE_WITH_KNOTS('',3,(#39264,#39265,#39266,#39267,#39268,
#39269),.UNSPECIFIED.,.F.,.F.,(4,1,1,4),(14.3987024268659,14.8976967170768,
15.3966910072877,15.7079632679489),.UNSPECIFIED.);
#348=B_SPLINE_CURVE_WITH_KNOTS('',3,(#39273,#39274,#39275,#39276,#39277,
#39278,#39279,#39280,#39281,#39282,#39283,#39284,#39285,#39286,#39287,#39288,
#39289,#39290,#39291,#39292,#39293,#39294,#39295,#39296,#39297,#39298,#39299,
#39300,#39301,#39302,#39303,#39304,#39305,#39306,#39307,#39308,#39309,#39310,
#39311,#39312,#39313,#39314,#39315,#39316,#39317,#39318,#39319,#39320,#39321,
#39322,#39323,#39324,#39325,#39326,#39327,#39328,#39329,#39330,#39331,#39332,
#39333,#39334,#39335,#39336,#39337,#39338,#39339,#39340,#39341,#39342,#39343,
#39344,#39345,#39346,#39347,#39348,#39349,#39350,#39351,#39352,#39353,#39354),
 .UNSPECIFIED.,.F.,.F.,(4,3,3,3,3,3,3,3,3,3,3,3,3,3,3,3,3,3,3,3,3,3,3,3,
3,3,3,4),(13.8756314554422,13.9455244015096,14.0154054819089,14.085279198689,
14.1551582454853,14.2250368331584,14.2949311931912,14.3470074157995,14.4170482343004,
14.487077175958,14.5570983621865,14.6293241981425,14.6993491698426,14.7726754379265,
14.8460017060104,14.9160393182244,14.9860649926552,15.0560828595175,15.1283111436935,
15.198332708346,15.2716643522837,15.3449959962214,15.4148686130277,15.488142276758,
15.5579967616873,15.6278466788921,15.697700868083,15.7079632679489),
 .UNSPECIFIED.);
#349=B_SPLINE_CURVE_WITH_KNOTS('',3,(#39355,#39356,#39357,#39358,#39359,
#39360,#39361,#39362,#39363,#39364,#39365,#39366,#39367,#39368,#39369,#39370,
#39371,#39372,#39373,#39374,#39375,#39376,#39377,#39378,#39379,#39380,#39381,
#39382,#39383,#39384,#39385,#39386,#39387,#39388,#39389,#39390,#39391,#39392,
#39393,#39394,#39395,#39396,#39397,#39398,#39399,#39400,#39401,#39402,#39403,
#39404,#39405,#39406,#39407,#39408,#39409,#39410,#39411,#39412,#39413,#39414,
#39415,#39416,#39417,#39418,#39419,#39420,#39421,#39422,#39423,#39424,#39425,
#39426,#39427,#39428,#39429,#39430,#39431,#39432,#39433,#39434,#39435,#39436,
#39437,#39438,#39439,#39440,#39441,#39442,#39443,#39444,#39445,#39446,#39447,
#39448,#39449,#39450,#39451),.UNSPECIFIED.,.F.,.F.,(4,3,3,3,3,3,3,3,3,3,
3,3,3,3,3,3,3,3,3,3,3,3,3,3,3,3,3,3,3,3,3,3,4),(15.7079632680278,15.781258546969,
15.8439902864323,15.9140293859905,15.9840565719878,16.0540759705774,16.1263031220939,
16.1963262492752,16.2696554129592,16.3429845766432,16.4130258394328,16.4830552130784,
16.5530768178735,16.6253023301186,16.6953276818739,16.768653274364,16.8419788668541,
16.9120192399517,16.9820477145933,17.0520684134795,17.1242945993759,17.1943190394544,
17.2676460982597,17.3409731570651,17.4110137716016,17.4810424897669,17.5510634336108,
17.6232894370271,17.6933141225493,17.7666407849127,17.839967447276,17.9100073812242,
17.933415291275),.UNSPECIFIED.);
#350=B_SPLINE_CURVE_WITH_KNOTS('',3,(#39457,#39458,#39459,#39460,#39461,
#39462,#39463,#39464,#39465,#39466,#39467,#39468,#39469,#39470,#39471,#39472,
#39473,#39474,#39475,#39476,#39477,#39478,#39479,#39480,#39481,#39482,#39483,
#39484,#39485,#39486,#39487,#39488,#39489,#39490,#39491,#39492,#39493,#39494,
#39495,#39496,#39497,#39498,#39499,#39500,#39501,#39502,#39503,#39504,#39505,
#39506,#39507,#39508,#39509,#39510,#39511,#39512,#39513,#39514,#39515,#39516,
#39517,#39518,#39519,#39520,#39521,#39522,#39523,#39524,#39525,#39526),
 .UNSPECIFIED.,.F.,.F.,(4,3,3,3,3,3,3,3,3,3,3,3,3,3,3,3,3,3,3,3,3,3,3,4),
(42.3163681282077,42.389003921528,42.4145146679284,42.48729869792,42.5600703328061,
42.632833872698,42.7056024032701,42.7783690429379,42.8511510266575,42.9135089581394,
42.9859787125309,43.0584354826672,43.1308844455598,43.2033410888313,43.275797773863,
43.3482751674385,43.4125032483503,43.4856192267066,43.5587218933442,43.6318145250677,
43.7049066040599,43.7779931512484,43.8510867420094,43.9114975385612),
 .UNSPECIFIED.);
#351=B_SPLINE_CURVE_WITH_KNOTS('',3,(#39529,#39530,#39531,#39532,#39533,
#39534,#39535,#39536,#39537,#39538,#39539,#39540,#39541,#39542,#39543,#39544,
#39545,#39546,#39547,#39548,#39549,#39550,#39551,#39552,#39553,#39554,#39555,
#39556,#39557,#39558,#39559,#39560,#39561,#39562,#39563,#39564,#39565,#39566,
#39567,#39568,#39569,#39570,#39571,#39572,#39573,#39574,#39575,#39576,#39577,
#39578,#39579,#39580),.UNSPECIFIED.,.F.,.F.,(4,2,2,2,2,2,2,2,2,2,2,2,2,
2,2,2,2,2,2,2,2,2,2,2,2,4),(-44.0788261103538,-43.9100592942155,-43.7715029329665,
-43.7074184572621,-43.6112929604573,-43.4302409268727,-43.2699713391976,
-43.0774948020758,-42.9661053858083,-42.8280933119776,-42.6572261911526,
-42.5615004460577,-42.3810883050336,-42.2202473083055,-42.0277910513795,
-41.9140420430288,-41.7767841864719,-41.610215244241,-41.5129059215617,
-41.4051211968993,-41.2624970586652,-41.0648615614014,-40.9791137834735,
-40.8748767190918,-40.7342210145313,-40.6004689346889),.UNSPECIFIED.);
#352=B_SPLINE_CURVE_WITH_KNOTS('',3,(#39586,#39587,#39588,#39589,#39590,
#39591,#39592,#39593,#39594,#39595),.UNSPECIFIED.,.F.,.F.,(4,1,1,1,1,1,
1,4),(36.0332287400247,36.4265831853974,36.9255774756083,37.4245717658192,
37.9235660560301,38.4225603462411,38.921554636452,39.0083726841606),
 .UNSPECIFIED.);
#353=B_SPLINE_CURVE_WITH_KNOTS('',3,(#39596,#39597,#39598,#39599,#39600,
#39601,#39602,#39603,#39604,#39605,#39606,#39607,#39608,#39609,#39610,#39611,
#39612,#39613,#39614,#39615,#39616,#39617,#39618,#39619,#39620,#39621,#39622,
#39623,#39624,#39625,#39626,#39627,#39628,#39629,#39630,#39631,#39632,#39633,
#39634,#39635,#39636,#39637,#39638,#39639,#39640,#39641,#39642,#39643,#39644,
#39645,#39646,#39647,#39648,#39649,#39650,#39651,#39652,#39653,#39654,#39655,
#39656,#39657,#39658,#39659,#39660,#39661,#39662,#39663,#39664,#39665,#39666,
#39667,#39668,#39669,#39670,#39671,#39672,#39673,#39674,#39675,#39676,#39677,
#39678,#39679,#39680,#39681,#39682,#39683,#39684,#39685,#39686,#39687,#39688,
#39689,#39690,#39691,#39692,#39693,#39694,#39695,#39696,#39697,#39698,#39699,
#39700,#39701,#39702,#39703,#39704,#39705,#39706,#39707,#39708,#39709,#39710,
#39711,#39712,#39713,#39714,#39715,#39716,#39717,#39718,#39719,#39720,#39721,
#39722,#39723,#39724,#39725,#39726,#39727,#39728,#39729,#39730,#39731,#39732,
#39733,#39734,#39735,#39736,#39737),.UNSPECIFIED.,.F.,.F.,(4,3,3,3,3,3,
3,3,3,3,3,3,3,3,3,3,3,3,3,3,3,3,3,3,3,3,3,3,3,3,3,3,3,3,3,3,3,3,3,3,3,3,
3,3,3,3,3,4),(39.0083726877398,39.0807497775609,39.1531170797185,39.225488567641,
39.2978589558457,39.3702461345474,39.4205489266629,39.4932256719064,39.5658896866155,
39.6385455807479,39.711207210472,39.7838675238172,39.8565448817808,39.9195432168738,
39.9922242628658,40.0648925892348,40.1375527937686,40.2102187009694,40.2828832672999,
40.3555648079552,40.4185375070847,40.4912126225807,40.5638750101892,40.6365292843827,
40.7091893168006,40.7818480476756,40.8545238586228,40.9175317972957,40.9902104856699,
41.062876431308,41.1355342389029,41.2081977415302,41.2808599026547,41.353539054321,
41.4165260875066,41.4892161017965,41.561893459126,41.6345627313086,41.7072376971513,
41.7799113036542,41.8526017895961,41.9155203777175,41.9881552979112,42.0607769946022,
42.1333953792814,42.2060085346025,42.2786289307035,42.3163681282077),
 .UNSPECIFIED.);
#354=B_SPLINE_CURVE_WITH_KNOTS('',3,(#39738,#39739,#39740,#39741,#39742,
#39743,#39744,#39745,#39746,#39747,#39748,#39749,#39750,#39751,#39752,#39753,
#39754,#39755,#39756,#39757,#39758,#39759,#39760,#39761,#39762,#39763,#39764,
#39765,#39766,#39767,#39768,#39769,#39770,#39771,#39772,#39773,#39774,#39775,
#39776,#39777,#39778,#39779,#39780,#39781,#39782,#39783,#39784,#39785,#39786,
#39787,#39788,#39789,#39790,#39791,#39792,#39793,#39794,#39795,#39796,#39797,
#39798,#39799,#39800,#39801,#39802,#39803,#39804,#39805,#39806,#39807,#39808,
#39809,#39810,#39811,#39812,#39813,#39814,#39815,#39816,#39817,#39818,#39819,
#39820,#39821,#39822,#39823,#39824,#39825,#39826,#39827,#39828,#39829,#39830,
#39831,#39832,#39833,#39834,#39835,#39836,#39837,#39838,#39839),
 .UNSPECIFIED.,.F.,.F.,(4,2,2,2,2,2,2,2,2,2,2,2,2,2,2,2,2,2,2,2,2,2,2,2,
2,2,2,2,2,2,2,2,2,2,2,2,2,2,2,2,2,2,2,2,2,2,2,2,2,2,4),(-40.6004689346889,
-40.5382784573951,-40.4534405320164,-40.3416795319586,-40.2037368545846,
-40.0326379413695,-39.9370698191387,-39.8251955624539,-39.6845032915067,
-39.4885263073456,-39.403674714177,-39.2918929257224,-39.1539481787511,
-38.9828339395382,-38.8872668655935,-38.7067744022686,-38.5459606666476,
-38.3535424066591,-38.2397373413956,-38.1024465050108,-37.9357284554644,
-37.8384839479232,-37.7304538855592,-37.5879176504572,-37.3903593908053,
-37.304622440894,-37.2004669159065,-37.0597470509154,-36.8637359886231,
-36.7788689324912,-36.667072666136,-36.5291062499929,-36.3579734505362,
-36.2623864991692,-36.0819166913421,-35.9210530384614,-35.7285782081487,
-35.6147565473853,-35.4774450105914,-35.310701862699,-35.2134429347374,
-35.1053958777011,-34.962838858293,-34.7652516189409,-34.6795019382082,
-34.5753295110467,-34.4345891017111,-34.2385490090928,-34.1536696820834,
-34.0418530693211,-33.9901053404391),.UNSPECIFIED.);
#355=B_SPLINE_CURVE_WITH_KNOTS('',3,(#39845,#39846,#39847,#39848,#39849,
#39850,#39851,#39852,#39853,#39854,#39855,#39856,#39857,#39858,#39859,#39860,
#39861,#39862,#39863,#39864,#39865,#39866,#39867,#39868,#39869,#39870,#39871,
#39872,#39873,#39874,#39875,#39876,#39877,#39878,#39879,#39880,#39881,#39882,
#39883,#39884,#39885,#39886,#39887,#39888),.UNSPECIFIED.,.F.,.F.,(4,2,2,
2,2,2,2,2,2,2,2,2,2,2,2,2,2,2,2,2,2,4),(-3.12972961237737,-3.02357540757013,
-2.9118472766391,-2.82699219400489,-2.63100103262062,-2.49030154085052,
-2.38757442686493,-2.30338638173099,-2.10758954946452,-1.96765695708937,
-1.86128621636086,-1.66893810480045,-1.5071366225871,-1.33126439654607,
-1.23915881419717,-1.05929928033435,-0.920096409516259,-0.811915618831055,
-0.619563874526152,-0.458108313007325,-0.280274621053177,-9.05352858358878E-5),
 .UNSPECIFIED.);
#356=B_SPLINE_CURVE_WITH_KNOTS('',3,(#39889,#39890,#39891,#39892,#39893,
#39894,#39895,#39896,#39897,#39898,#39899),.UNSPECIFIED.,.F.,.F.,(4,1,1,
1,1,1,1,1,4),(32.725187376981,32.9336231539209,33.4326174441318,33.9316117343428,
34.4306060245537,34.9296003147646,35.4285946049755,35.9275888951864,36.0332287400247),
 .UNSPECIFIED.);
#357=B_SPLINE_CURVE_WITH_KNOTS('',3,(#39900,#39901,#39902,#39903,#39904,
#39905,#39906,#39907,#39908,#39909,#39910,#39911,#39912,#39913,#39914,#39915,
#39916,#39917,#39918,#39919,#39920,#39921,#39922,#39923,#39924,#39925,#39926,
#39927,#39928,#39929,#39930,#39931,#39932,#39933,#39934,#39935,#39936,#39937,
#39938,#39939,#39940,#39941,#39942,#39943,#39944,#39945,#39946,#39947,#39948,
#39949,#39950,#39951,#39952,#39953,#39954,#39955,#39956,#39957,#39958,#39959,
#39960,#39961,#39962,#39963,#39964,#39965,#39966,#39967,#39968,#39969,#39970,
#39971,#39972,#39973,#39974,#39975,#39976,#39977,#39978,#39979,#39980,#39981,
#39982,#39983,#39984,#39985,#39986,#39987,#39988,#39989,#39990,#39991,#39992,
#39993,#39994,#39995),.UNSPECIFIED.,.F.,.F.,(4,2,2,2,2,2,2,2,2,2,2,2,2,
2,2,2,2,2,2,2,2,2,2,2,2,2,2,2,2,2,2,2,2,2,2,2,2,2,2,2,2,2,2,2,2,2,2,4),
(-33.9901053404391,-33.9038673318948,-33.7327011419815,-33.637106182711,
-33.4565608324522,-33.2956990203788,-33.1032226333052,-32.9893828405317,
-32.8520512012745,-32.6852812141468,-32.5880094929732,-32.479942641251,
-32.3373661984005,-32.1397513242891,-32.0539895105622,-31.9498084148103,
-31.8090448132149,-31.6129742235052,-31.5280807487632,-31.4162587573692,
-31.2782486103253,-31.1070816380028,-31.0114528472798,-30.8310388829762,
-30.670069132821,-30.4774319561785,-30.3631025817692,-30.2258998761992,
-30.0582964428501,-29.9617041394288,-29.8519653702877,-29.7101594091751,
-29.5132722958157,-29.427812221667,-29.3194457043472,-29.1801681390832,
-29.0002019561717,-28.9080559415564,-28.7321128205142,-28.5701604041746,
-28.3774966919828,-28.2702927158626,-28.1305494704203,-27.9507188228387,
-27.8579567925644,-27.6805464113609,-27.5190867418308,-27.3770201043626),
 .UNSPECIFIED.);
#358=B_SPLINE_CURVE_WITH_KNOTS('',3,(#40000,#40001,#40002,#40003,#40004,
#40005,#40006,#40007,#40008,#40009,#40010,#40011,#40012,#40013,#40014,#40015,
#40016,#40017,#40018,#40019,#40020,#40021,#40022,#40023,#40024,#40025,#40026,
#40027,#40028,#40029,#40030,#40031,#40032,#40033,#40034,#40035,#40036,#40037,
#40038,#40039,#40040,#40041,#40042,#40043,#40044,#40045,#40046,#40047,#40048,
#40049,#40050,#40051,#40052,#40053,#40054,#40055,#40056,#40057,#40058,#40059,
#40060,#40061,#40062,#40063,#40064,#40065,#40066,#40067,#40068,#40069,#40070,
#40071,#40072,#40073,#40074,#40075,#40076,#40077,#40078,#40079,#40080,#40081,
#40082,#40083,#40084,#40085,#40086,#40087,#40088,#40089,#40090,#40091,#40092,
#40093,#40094,#40095,#40096,#40097,#40098,#40099),.UNSPECIFIED.,.F.,.F.,
(4,2,2,2,2,2,2,2,2,2,2,2,2,2,2,2,2,2,2,2,2,2,2,2,2,2,2,2,2,2,2,2,2,2,2,
2,2,2,2,2,2,2,2,2,2,2,2,2,2,4),(-9.73964911326357,-9.65894423564208,-9.52165405446729,
-9.3550271395587,-9.25772955066524,-9.14984664875812,-9.0072582203635,-8.8096536995634,
-8.72390183789383,-8.61720571772894,-8.47737195858178,-8.28150856230035,
-8.19745982266304,-8.09412525168699,-7.95365224694775,-7.75777396042404,
-7.67308436584228,-7.55990517587196,-7.42241227653874,-7.24394313945267,
-7.15319218095859,-6.98064229341811,-6.81757845654217,-6.68181777293533,
-6.60983127964453,-6.48324291880089,-6.31089336699378,-6.17277800050596,
-6.06145328491304,-5.97652415069389,-5.78044190248597,-5.63962740124722,
-5.5370822032355,-5.34422406511019,-5.18331135139813,-5.003004613449,-4.90741064099126,
-4.73631665844469,-4.59836968489508,-4.48660310628703,-4.40174350696052,
-4.2057366129771,-4.06502900376254,-3.96227941747858,-3.76913349288581,
-3.60798908702072,-3.42816805541769,-3.33253521362127,-3.16151849539383,
-3.12972961237737),.UNSPECIFIED.);
#359=B_SPLINE_CURVE_WITH_KNOTS('',3,(#40100,#40101,#40102,#40103,#40104,
#40105,#40106,#40107,#40108,#40109,#40110,#40111,#40112,#40113,#40114,#40115,
#40116,#40117,#40118,#40119,#40120,#40121,#40122,#40123,#40124,#40125,#40126,
#40127,#40128,#40129,#40130,#40131,#40132,#40133,#40134,#40135,#40136,#40137,
#40138,#40139,#40140,#40141,#40142,#40143,#40144,#40145,#40146,#40147,#40148,
#40149,#40150,#40151,#40152,#40153,#40154,#40155,#40156,#40157,#40158,#40159,
#40160,#40161,#40162,#40163,#40164,#40165,#40166,#40167,#40168,#40169,#40170,
#40171,#40172,#40173,#40174,#40175,#40176,#40177,#40178,#40179,#40180,#40181,
#40182,#40183,#40184,#40185,#40186,#40187,#40188,#40189,#40190,#40191,#40192,
#40193,#40194,#40195,#40196,#40197,#40198,#40199),.UNSPECIFIED.,.F.,.F.,
(4,2,2,2,2,2,2,2,2,2,2,2,2,2,2,2,2,2,2,2,2,2,2,2,2,2,2,2,2,2,2,2,2,2,2,
2,2,2,2,2,2,2,2,2,2,2,2,2,2,4),(-27.3770201043626,-27.3259869988704,-27.2121100458388,
-27.0747318318027,-26.907907677031,-26.8106015462648,-26.7025019622452,
-26.5598757460337,-26.3621925865554,-26.276401273343,-26.1721783179693,
-26.031369543728,-25.835234238612,-25.7503136825854,-25.6384428300776,-25.5003900650916,
-25.3291408924148,-25.2334994027494,-25.1215330292327,-24.980722116227,
-24.7845791659393,-24.6996577482217,-24.587751418088,-24.4497009256982,
-24.2783782653954,-24.1827821137484,-24.0018061486208,-23.8410358604269,
-23.648313506953,-23.5456683319773,-23.4047387851586,-23.208514119051,-23.1235150604426,
-23.0121125410751,-22.8738727807086,-22.7013677308331,-22.6062089414503,
-22.4931655671665,-22.3528244948875,-22.1626309692493,-22.0396620413223,
-21.8456830127117,-21.6867004145244,-21.5047151786164,-21.4130670928768,
-21.2333822520101,-21.0946713588781,-20.984635287894,-20.89943271034,-20.7616952607919),
 .UNSPECIFIED.);
#360=B_SPLINE_CURVE_WITH_KNOTS('',3,(#40205,#40206,#40207,#40208,#40209,
#40210,#40211,#40212,#40213,#40214,#40215,#40216,#40217,#40218,#40219,#40220,
#40221,#40222,#40223,#40224,#40225,#40226,#40227,#40228,#40229,#40230,#40231,
#40232,#40233,#40234,#40235,#40236,#40237,#40238,#40239,#40240,#40241,#40242,
#40243,#40244,#40245,#40246,#40247,#40248,#40249,#40250,#40251,#40252),
 .UNSPECIFIED.,.F.,.F.,(4,2,2,2,2,2,2,2,2,2,2,2,2,2,2,2,2,2,2,2,2,2,2,4),
(-3.1291763693966,-3.06051423746629,-2.92058449029293,-2.81420514005639,
-2.62190166055115,-2.46014874464375,-2.28413518085184,-2.19197068595235,
-2.01208501479044,-1.87281886403111,-1.7648008422835,-1.67935277495058,
-1.48248212458146,-1.3406588528544,-1.23128928405176,-1.13465866826387,
-0.967307336117015,-0.830191190375465,-0.716028156243458,-0.52358859575441,
-0.362789859682845,-0.261165452376227,-0.169848216096543,-9.06239312916104E-5),
 .UNSPECIFIED.);
#361=B_SPLINE_CURVE_WITH_KNOTS('',3,(#40253,#40254,#40255,#40256,#40257,
#40258,#40259,#40260,#40261,#40262,#40263,#40264,#40265,#40266,#40267,#40268,
#40269,#40270,#40271,#40272,#40273,#40274,#40275,#40276,#40277,#40278,#40279,
#40280,#40281,#40282,#40283,#40284,#40285,#40286,#40287,#40288,#40289,#40290,
#40291,#40292,#40293,#40294,#40295,#40296,#40297,#40298,#40299,#40300,#40301,
#40302),.UNSPECIFIED.,.F.,.F.,(4,2,2,2,2,2,2,2,2,2,2,2,2,2,2,2,2,2,2,2,
2,2,2,2,4),(-13.2194666776149,-12.9315530398099,-12.75122112135,-12.589908851332,
-12.3969841603575,-12.2832071728717,-12.1459516433032,-11.9792739482411,
-11.8820560811831,-11.7740494421549,-11.6315517500151,-11.4340460508408,
-11.3483315663086,-11.2442051653794,-11.1035204605134,-10.9075589984911,
-10.8227130527622,-10.7109499613579,-10.5730172528488,-10.4019388774833,
-10.3063678811762,-10.126014625418,-9.96515477963546,-9.77269368223828,
-9.73964911326357),.UNSPECIFIED.);
#362=B_SPLINE_CURVE_WITH_KNOTS('',3,(#40303,#40304,#40305,#40306,#40307,
#40308,#40309,#40310,#40311,#40312,#40313,#40314,#40315,#40316,#40317,#40318,
#40319,#40320,#40321,#40322,#40323,#40324,#40325,#40326,#40327,#40328,#40329,
#40330,#40331,#40332,#40333,#40334,#40335,#40336,#40337,#40338,#40339,#40340,
#40341,#40342,#40343,#40344,#40345,#40346,#40347,#40348,#40349,#40350,#40351,
#40352,#40353,#40354,#40355,#40356,#40357,#40358,#40359,#40360,#40361,#40362,
#40363,#40364,#40365,#40366,#40367,#40368,#40369,#40370,#40371,#40372,#40373,
#40374,#40375,#40376,#40377,#40378,#40379,#40380,#40381,#40382,#40383,#40384,
#40385,#40386,#40387,#40388,#40389,#40390,#40391,#40392,#40393,#40394,#40395,
#40396,#40397,#40398),.UNSPECIFIED.,.F.,.F.,(4,2,2,2,2,2,2,2,2,2,2,2,2,
2,2,2,2,2,2,2,2,2,2,2,2,2,2,2,2,2,2,2,2,2,2,2,2,2,2,2,2,2,2,2,2,2,2,4),
(-20.7616952607919,-20.7029496957438,-20.5616751617043,-20.4598332609485,
-20.3752879168612,-20.1793086272156,-20.0389735427187,-19.9259781567096,
-19.830811580402,-19.6583753171218,-19.5201676949303,-19.4087472888494,
-19.323760071219,-19.1275406855933,-18.9866294727618,-18.8840041560849,
-18.6906355469538,-18.5292460976927,-18.3515792968921,-18.2587033595283,
-18.0792230303878,-17.9395673429201,-17.8321166758214,-17.6396150280574,
-17.4778874941757,-17.3012505448391,-17.2088095322091,-17.0287011678067,
-16.8891105195559,-16.7815262771041,-16.5890128193696,-16.427297435627,
-16.2506692805385,-16.1582332097997,-15.9781367449341,-15.8385542371383,
-15.7309808305531,-15.5384940691259,-15.3768029696543,-15.2001485340552,
-15.1077027118569,-14.9276141391687,-14.7880249429551,-14.6805000622446,
-14.4879272859893,-14.326137266756,-14.1498118449496,-14.1472447933216),
 .UNSPECIFIED.);
#363=B_SPLINE_CURVE_WITH_KNOTS('',3,(#40403,#40404,#40405,#40406,#40407,
#40408,#40409,#40410,#40411,#40412,#40413,#40414,#40415,#40416,#40417,#40418,
#40419,#40420,#40421,#40422,#40423,#40424,#40425,#40426,#40427,#40428,#40429,
#40430,#40431,#40432,#40433,#40434,#40435,#40436,#40437,#40438,#40439,#40440,
#40441,#40442,#40443,#40444,#40445,#40446,#40447,#40448,#40449,#40450,#40451,
#40452,#40453,#40454,#40455,#40456,#40457,#40458,#40459,#40460,#40461,#40462,
#40463,#40464,#40465,#40466,#40467,#40468,#40469,#40470,#40471,#40472,#40473,
#40474,#40475,#40476,#40477,#40478,#40479,#40480,#40481,#40482,#40483,#40484,
#40485,#40486,#40487,#40488,#40489,#40490,#40491,#40492,#40493,#40494,#40495,
#40496),.UNSPECIFIED.,.F.,.F.,(4,2,2,2,2,2,2,2,2,2,2,2,2,2,2,2,2,2,2,2,
2,2,2,2,2,2,2,2,2,2,2,2,2,2,2,2,2,2,2,2,2,2,2,2,2,2,4),(-9.73907321948152,
-9.68207929033005,-9.50606682630167,-9.34429241933644,-9.15174505724938,
-9.04418921938962,-8.90471039453844,-8.72475108610191,-8.63238861275138,
-8.4558984142504,-8.29427536776061,-8.10176496422375,-7.99359727989772,
-7.85434396130632,-7.67445500876044,-7.58231096741114,-7.40634697865959,
-7.24452603681246,-7.05199716640114,-6.94479278155016,-6.80515102333529,
-6.60907326560968,-6.49007026026039,-6.29718462836577,-6.13630043188297,
-5.95593809362674,-5.86035028525291,-5.6892474537243,-5.55130125481543,
-5.4395305186487,-5.35467110717155,-5.15866392769172,-5.01795654371566,
-4.91520488564753,-4.72235805791818,-4.56150317778389,-4.38113214900285,
-4.28555670779011,-4.11446637221707,-3.97653408287644,-3.86477229610324,
-3.77992130119884,-3.58393321331188,-3.44323974315957,-3.3404971617921,
-3.25631275523785,-3.1291763693966),.UNSPECIFIED.);
#364=B_SPLINE_CURVE_WITH_KNOTS('',3,(#40497,#40498,#40499,#40500,#40501,
#40502,#40503,#40504,#40505,#40506,#40507,#40508,#40509,#40510,#40511,#40512,
#40513,#40514,#40515,#40516,#40517,#40518,#40519,#40520,#40521,#40522,#40523,
#40524,#40525,#40526,#40527,#40528,#40529,#40530,#40531,#40532,#40533,#40534,
#40535,#40536,#40537,#40538,#40539,#40540,#40541,#40542,#40543,#40544,#40545,
#40546,#40547,#40548,#40549,#40550,#40551,#40552,#40553,#40554,#40555,#40556,
#40557,#40558,#40559,#40560,#40561,#40562,#40563,#40564,#40565,#40566,#40567,
#40568,#40569,#40570,#40571,#40572,#40573,#40574,#40575,#40576,#40577,#40578,
#40579,#40580,#40581,#40582,#40583,#40584,#40585,#40586,#40587,#40588,#40589,
#40590,#40591,#40592,#40593,#40594),.UNSPECIFIED.,.F.,.F.,(4,2,2,2,2,2,
2,2,2,2,2,2,2,2,2,2,2,2,2,2,2,2,2,2,2,2,2,2,2,2,2,2,2,2,2,2,2,2,2,2,2,2,
2,2,2,2,2,2,4),(-14.1472447933216,-14.0575049034936,-13.8774699909368,-13.7380261550839,
-13.6301613925409,-13.5446124284645,-13.3475129133717,-13.2054895048621,
-13.0962773970659,-12.9994925420233,-12.8321382968731,-12.6949129619141,
-12.5807375184919,-12.3881730793577,-12.2272643235089,-12.0467975217235,
-11.9511856625091,-11.7800223315118,-11.642034203121,-11.530225553396,-11.4453399801411,
-11.2492718413425,-11.1085208405746,-11.0057366599301,-10.9215177099878,
-10.7256392876854,-10.5856521355424,-10.4792301701748,-10.2867797134512,
-10.1248885606261,-9.94900977779425,-9.85689350345923,-9.67697256748017,
-9.53774173278488,-9.42943981513686,-9.23675780060404,-9.07499128425171,
-8.89879946346959,-8.80655398530214,-8.62658737009246,-8.48722110161676,
-8.37930287719263,-8.29379866125501,-8.0968018075072,-7.95486647715765,
-7.84559633168378,-7.74887863963778,-7.58153365577835,-7.53564154876179),
 .UNSPECIFIED.);
#365=B_SPLINE_CURVE_WITH_KNOTS('',3,(#40600,#40601,#40602,#40603,#40604,
#40605,#40606,#40607,#40608,#40609,#40610,#40611,#40612,#40613),
 .UNSPECIFIED.,.F.,.F.,(4,2,2,2,2,2,4),(-0.926590328528814,-0.753955484513565,
-0.6139958295923,-0.515954230626158,-0.443702087204974,-0.243068847343075,
-0.000135688299652575),.UNSPECIFIED.);
#366=B_SPLINE_CURVE_WITH_KNOTS('',3,(#40616,#40617,#40618,#40619,#40620,
#40621,#40622,#40623,#40624,#40625,#40626,#40627,#40628,#40629,#40630,#40631,
#40632,#40633,#40634,#40635,#40636,#40637,#40638,#40639,#40640,#40641,#40642,
#40643,#40644,#40645,#40646,#40647,#40648,#40649,#40650,#40651,#40652,#40653,
#40654,#40655,#40656,#40657,#40658,#40659,#40660,#40661,#40662,#40663,#40664,
#40665,#40666,#40667,#40668,#40669,#40670,#40671,#40672,#40673,#40674,#40675,
#40676,#40677,#40678,#40679,#40680,#40681,#40682,#40683,#40684,#40685,#40686,
#40687,#40688,#40689,#40690,#40691,#40692,#40693,#40694,#40695,#40696,#40697,
#40698,#40699,#40700,#40701,#40702,#40703,#40704,#40705,#40706,#40707,#40708,
#40709,#40710,#40711,#40712,#40713,#40714,#40715,#40716,#40717,#40718,#40719,
#40720,#40721,#40722,#40723,#40724,#40725,#40726,#40727),.UNSPECIFIED.,
 .F.,.F.,(4,3,3,3,3,3,3,3,3,3,3,3,3,3,3,3,3,3,3,3,3,3,3,3,3,3,3,3,3,3,3,
3,3,3,3,3,3,4),(2.02359556728784,2.09612063785746,2.16863302303831,2.24113775293914,
2.31364811582229,2.38615861296181,2.45868474905377,2.49497145105461,2.56765002727523,
2.64031589890252,2.71297367059207,2.78563719645063,2.85829941345175,2.93097867400525,
2.99396574126554,3.06664098081929,3.13930345029594,3.21195776421116,3.28461777093719,
3.35727644001194,3.42995213051997,3.49296003147646,3.56564099670242,3.63830926977429,
3.71096944845288,3.78363537238572,3.85629997895852,3.92898159803042,3.99195432168738,
4.06463110674485,4.13729514772772,4.20995105460738,4.28261267608537,4.35527296959603,
4.42795028890617,4.49094861189831,4.56362770609116,4.61729307130943),
 .UNSPECIFIED.);
#367=B_SPLINE_CURVE_WITH_KNOTS('',3,(#40730,#40731,#40732,#40733,#40734,
#40735,#40736,#40737,#40738,#40739,#40740,#40741,#40742,#40743,#40744,#40745,
#40746,#40747,#40748,#40749,#40750,#40751,#40752,#40753,#40754,#40755,#40756,
#40757,#40758,#40759,#40760,#40761,#40762,#40763,#40764,#40765,#40766,#40767,
#40768,#40769,#40770,#40771,#40772,#40773,#40774,#40775,#40776,#40777,#40778,
#40779,#40780,#40781,#40782,#40783,#40784,#40785,#40786,#40787,#40788,#40789,
#40790,#40791,#40792,#40793,#40794,#40795,#40796,#40797,#40798,#40799,#40800,
#40801,#40802,#40803,#40804,#40805,#40806,#40807,#40808,#40809,#40810,#40811,
#40812,#40813,#40814,#40815,#40816,#40817,#40818,#40819,#40820,#40821,#40822,
#40823,#40824,#40825,#40826,#40827,#40828,#40829,#40830,#40831,#40832,#40833,
#40834,#40835,#40836,#40837,#40838,#40839,#40840,#40841,#40842,#40843,#40844,
#40845,#40846,#40847,#40848,#40849,#40850,#40851,#40852,#40853,#40854,#40855,
#40856),.UNSPECIFIED.,.F.,.F.,(4,3,3,3,3,3,3,3,3,3,3,3,3,3,3,3,3,3,3,3,
3,3,3,3,3,3,3,3,3,3,3,3,3,3,3,3,3,3,3,3,3,3,4),(4.61729307130943,4.68995293710172,
4.7649504283536,4.83761291716063,4.91377790963493,4.98994290210923,5.06262100423254,
5.13528637842111,5.20794363080203,5.280606607111,5.35326825861506,5.42594693144097,
5.48893719232016,5.56161554328838,5.63428116853687,5.70693867347046,5.77960190281452,
5.85226380724567,5.92494273101668,5.98793148253108,6.06060984370026,6.13327547967456,
6.20593299582697,6.27859623707525,6.35125815377287,6.42393709031945,6.486925772742,
6.55960406326347,6.63226962758147,6.70492707127597,6.77759023934746,6.85025208257815,
6.92293094570417,6.98592006295293,7.05859841273454,7.13126403706467,7.20392154135016,
7.27658477047137,7.3492466749157,7.42192559908852,7.48491435316385,7.56187309461106,
7.59244614826265),.UNSPECIFIED.);
#368=B_SPLINE_CURVE_WITH_KNOTS('',3,(#40857,#40858,#40859,#40860,#40861,
#40862,#40863,#40864,#40865,#40866,#40867,#40868,#40869,#40870,#40871,#40872,
#40873,#40874,#40875,#40876,#40877,#40878,#40879,#40880,#40881,#40882,#40883,
#40884,#40885,#40886,#40887,#40888,#40889,#40890,#40891,#40892,#40893,#40894,
#40895,#40896,#40897,#40898,#40899,#40900,#40901,#40902,#40903,#40904,#40905,
#40906),.UNSPECIFIED.,.F.,.F.,(4,2,2,2,2,2,2,2,2,2,2,2,2,2,2,2,2,2,2,2,
2,2,2,2,4),(-13.2184356728779,-13.0690661818794,-12.9182477272931,-12.8289515586441,
-12.6545072282153,-12.4931147641064,-12.3007284920065,-12.1919123903746,
-12.0529529736406,-11.8732347157786,-11.7813473250141,-11.6059894283038,
-11.4440147867751,-11.2513298643328,-11.1440427766819,-11.0044821083306,
-10.8245209291215,-10.7320706544749,-10.5553651898818,-10.3938460406952,
-10.2014560813668,-10.0933860004824,-9.95411910849321,-9.7742410176212,
-9.73907321948152),.UNSPECIFIED.);
#369=B_SPLINE_CURVE_WITH_KNOTS('',3,(#40907,#40908,#40909,#40910,#40911,
#40912,#40913,#40914,#40915,#40916,#40917,#40918,#40919,#40920,#40921,#40922,
#40923,#40924,#40925,#40926,#40927,#40928,#40929,#40930,#40931,#40932,#40933,
#40934,#40935,#40936,#40937,#40938,#40939,#40940,#40941,#40942,#40943,#40944,
#40945,#40946,#40947,#40948,#40949,#40950,#40951,#40952,#40953,#40954,#40955,
#40956,#40957,#40958,#40959,#40960,#40961,#40962,#40963,#40964,#40965,#40966,
#40967,#40968,#40969,#40970,#40971,#40972,#40973,#40974,#40975,#40976,#40977,
#40978,#40979,#40980,#40981,#40982,#40983,#40984,#40985,#40986,#40987,#40988,
#40989,#40990,#40991,#40992,#40993,#40994,#40995,#40996,#40997,#40998,#40999,
#41000,#41001,#41002,#41003,#41004,#41005,#41006),.UNSPECIFIED.,.F.,.F.,
(4,2,2,2,2,2,2,2,2,2,2,2,2,2,2,2,2,2,2,2,2,2,2,2,2,2,2,2,2,2,2,2,2,2,2,
2,2,2,2,2,2,2,2,2,2,2,2,2,2,4),(-7.53564154876179,-7.44435895692881,-7.33019444534583,
-7.24560723684192,-7.0497538285448,-6.90940624634637,-6.79677075262341,
-6.7015593268547,-6.52958416487551,-6.39153932403596,-6.28004969084625,
-6.19514425977817,-5.99908544723558,-5.85829995364484,-5.75572199185766,
-5.67149445949106,-5.47569870552628,-5.33574083826483,-5.22938458578421,
-5.14353261448337,-4.94556272004269,-4.80263040407831,-4.69544159686438,
-4.59782648178253,-4.43158586807976,-4.29425923625493,-4.18071001141288,
-3.9881945699854,-3.8272860352096,-3.64697769618344,-3.55122885095793,-3.3828040614263,
-3.24580686616462,-3.13127629889031,-2.93878885368664,-2.77879708127779,
-2.59757913471578,-2.5020689489392,-2.33058784772183,-2.19201882225214,
-2.08183329883684,-1.89039846798437,-1.73322226283244,-1.54238350525133,
-1.43850896943895,-1.27779998733979,-1.13690736638403,-1.03040158727961,
-0.943996000995363,-0.926590328528814),.UNSPECIFIED.);
#370=B_SPLINE_CURVE_WITH_KNOTS('',3,(#41009,#41010,#41011,#41012,#41013,
#41014,#41015,#41016,#41017,#41018,#41019,#41020,#41021,#41022,#41023,#41024,
#41025,#41026,#41027,#41028,#41029,#41030,#41031,#41032,#41033,#41034,#41035,
#41036,#41037,#41038,#41039,#41040,#41041,#41042,#41043,#41044,#41045,#41046,
#41047,#41048,#41049,#41050,#41051,#41052,#41053,#41054,#41055,#41056,#41057,
#41058,#41059,#41060,#41061,#41062,#41063,#41064,#41065,#41066,#41067,#41068,
#41069,#41070,#41071,#41072,#41073,#41074,#41075,#41076,#41077,#41078,#41079,
#41080,#41081,#41082,#41083,#41084,#41085,#41086,#41087,#41088,#41089,#41090,
#41091,#41092,#41093,#41094,#41095,#41096,#41097,#41098,#41099,#41100,#41101,
#41102,#41103,#41104,#41105,#41106,#41107,#41108,#41109,#41110,#41111,#41112,
#41113,#41114,#41115,#41116,#41117,#41118,#41119,#41120,#41121,#41122,#41123,
#41124,#41125,#41126,#41127,#41128,#41129,#41130,#41131,#41132,#41133,#41134,
#41135,#41136,#41137,#41138,#41139,#41140,#41141,#41142,#41143,#41144,#41145,
#41146,#41147,#41148,#41149,#41150,#41151,#41152,#41153,#41154,#41155,#41156,
#41157,#41158,#41159,#41160,#41161,#41162,#41163,#41164,#41165,#41166,#41167,
#41168,#41169,#41170,#41171,#41172,#41173,#41174,#41175,#41176,#41177,#41178,
#41179,#41180,#41181,#41182,#41183),.UNSPECIFIED.,.F.,.F.,(4,3,3,3,3,3,
3,3,3,3,3,3,3,3,3,3,3,3,3,3,3,3,3,3,3,3,3,3,3,3,3,3,3,3,3,3,3,3,3,3,3,3,
3,3,3,3,3,3,3,3,3,3,3,3,3,3,3,3,4),(17.933415291275,18.0034409627842,18.0734602373726,
18.1434856452887,18.2135106587962,18.2835513152064,18.3389617374869,18.4090022932936,
18.4790309522727,18.5490518366316,18.6212778843982,18.6913025104407,18.7646292690693,
18.8379560276978,18.9079966408986,18.9780253579764,19.048046300983,19.1202723052145,
19.1902969905308,19.2636236542198,19.3369503179088,19.406990897852,19.47701958129,
19.5470404903645,19.6192665198033,19.6892911708883,19.762617889504,19.8359446081197,
19.9059852029146,19.9760139013638,20.0460348255693,20.1182608437596,20.1882855100817,
20.2616122042062,20.3349388983306,20.4049794883864,20.4750081820518,20.5450291014412,
20.6172551232163,20.6872797847037,20.7606064866226,20.8339331885415,20.9039737790573,
20.9740024731822,21.0440233930295,21.1162494144602,21.1862740763956,21.259600777574,
21.3329274787524,21.4029680700421,21.4729967649525,21.5430176855947,21.6152437064369,
21.6852683691804,21.7585950690719,21.8319217689634,21.9045986695098,21.9772545252523,
21.9911485750577),.UNSPECIFIED.);
#371=B_SPLINE_CURVE_WITH_KNOTS('',3,(#41184,#41185,#41186,#41187,#41188,
#41189,#41190,#41191,#41192,#41193,#41194,#41195,#41196,#41197,#41198,#41199,
#41200,#41201,#41202,#41203,#41204,#41205,#41206,#41207,#41208,#41209,#41210,
#41211,#41212,#41213,#41214,#41215,#41216,#41217,#41218,#41219,#41220,#41221,
#41222,#41223,#41224,#41225,#41226,#41227,#41228,#41229,#41230,#41231,#41232,
#41233,#41234,#41235,#41236,#41237,#41238,#41239,#41240,#41241,#41242,#41243,
#41244,#41245,#41246,#41247,#41248,#41249,#41250,#41251,#41252,#41253,#41254,
#41255,#41256,#41257,#41258,#41259,#41260,#41261,#41262,#41263,#41264,#41265,
#41266,#41267,#41268,#41269,#41270,#41271,#41272,#41273,#41274,#41275,#41276,
#41277,#41278,#41279,#41280),.UNSPECIFIED.,.F.,.F.,(4,3,3,3,3,3,3,3,3,3,
3,3,3,3,3,3,3,3,3,3,3,3,3,3,3,3,3,3,3,3,3,3,4),(21.9911485751285,22.0611187640108,
22.1310953555668,22.2010715824223,22.2710644969389,22.3309160591743,22.4009566501728,
22.4709853447878,22.541006265131,22.6132322861946,22.683256948635,22.7565836490101,
22.8299103493852,22.8999509401425,22.9699796345137,23.0400005546109,23.1122265758572,
23.18225123805,23.2555779388231,23.3289046395961,23.3989452304404,23.4689739248994,
23.5389948450855,23.6112208662659,23.6812455285476,23.7545722291773,23.8278989298071,
23.8979388431038,23.9679665406906,24.0379905648376,24.1080093565331,24.1780338634582,
24.216566741472),.UNSPECIFIED.);
#372=B_SPLINE_CURVE_WITH_KNOTS('',3,(#41282,#41283,#41284,#41285,#41286,
#41287,#41288,#41289,#41290,#41291,#41292,#41293,#41294,#41295,#41296,#41297,
#41298,#41299,#41300,#41301,#41302,#41303,#41304,#41305,#41306,#41307,#41308,
#41309,#41310,#41311,#41312,#41313,#41314,#41315,#41316,#41317,#41318,#41319,
#41320,#41321,#41322,#41323,#41324,#41325,#41326,#41327,#41328,#41329,#41330,
#41331,#41332,#41333,#41334,#41335,#41336,#41337,#41338,#41339,#41340,#41341,
#41342,#41343,#41344,#41345,#41346,#41347,#41348,#41349,#41350,#41351,#41352,
#41353,#41354,#41355,#41356,#41357,#41358,#41359,#41360,#41361,#41362,#41363,
#41364,#41365,#41366,#41367,#41368,#41369,#41370,#41371,#41372,#41373,#41374,
#41375,#41376,#41377,#41378),.UNSPECIFIED.,.F.,.F.,(4,3,3,3,3,3,3,3,3,3,
3,3,3,3,3,3,3,3,3,3,3,3,3,3,3,3,3,3,3,3,3,3,4),(21.9911485751285,22.0609174698852,
22.1306788205048,22.2004452722809,22.2702117236623,22.339993679049,22.3826110702406,
22.4526516650052,22.522680363424,22.5927012875987,22.6649273058119,22.7349519721031,
22.8082786662773,22.8816053604516,22.9516459505158,23.0216746441895,23.0916955635876,
23.1639215853563,23.2339462468523,23.3072729487574,23.3805996506625,23.4506402411789,
23.5206689353042,23.5906898551522,23.6629158765825,23.7329405385186,23.806267239696,
23.8795939408734,23.9496338916419,24.0196644904711,24.0896860414985,24.1597095893078,
24.2165701374682),.UNSPECIFIED.);
#373=B_SPLINE_CURVE_WITH_KNOTS('',3,(#41379,#41380,#41381,#41382,#41383,
#41384,#41385,#41386,#41387,#41388,#41389,#41390),.UNSPECIFIED.,.F.,.F.,
(4,1,1,1,1,1,1,1,1,4),(17.9334121841373,18.3906567485533,18.8896510387642,
19.3886453289751,19.887639619186,20.386633909397,20.8856281996079,21.3846224898188,
21.8836167800297,21.9911485751285),.UNSPECIFIED.);
#374=B_SPLINE_CURVE_WITH_KNOTS('',3,(#41756,#41757,#41758,#41759,#41760,
#41761,#41762,#41763,#41764,#41765,#41766,#41767,#41768,#41769,#41770,#41771,
#41772,#41773,#41774,#41775,#41776,#41777,#41778,#41779,#41780,#41781,#41782,
#41783,#41784,#41785,#41786,#41787,#41788,#41789,#41790,#41791,#41792,#41793,
#41794,#41795,#41796,#41797,#41798,#41799,#41800,#41801,#41802,#41803,#41804,
#41805,#41806,#41807,#41808,#41809,#41810,#41811,#41812,#41813,#41814,#41815,
#41816,#41817,#41818,#41819,#41820,#41821,#41822,#41823,#41824,#41825,#41826,
#41827,#41828,#41829,#41830,#41831,#41832,#41833,#41834,#41835,#41836,#41837,
#41838,#41839,#41840,#41841,#41842,#41843,#41844,#41845,#41846,#41847,#41848,
#41849,#41850,#41851,#41852,#41853,#41854,#41855,#41856,#41857,#41858,#41859,
#41860,#41861,#41862,#41863,#41864,#41865,#41866,#41867,#41868,#41869,#41870,
#41871,#41872,#41873,#41874,#41875,#41876),.UNSPECIFIED.,.F.,.F.,(4,3,3,
3,3,3,3,3,3,3,3,3,3,3,3,3,3,3,3,3,3,3,3,3,3,3,3,3,3,3,3,3,3,3,3,3,3,3,3,
3,4),(0.,0.0847077516938065,0.170225033901306,0.255907500614097,0.341119279334384,
0.425059357872854,0.455383656591401,0.465770691009882,0.474513364932373,
0.55829834295187,0.600642802906426,0.684662560232657,0.76868652492825,0.851862297560265,
0.912900878915177,0.924214418880625,0.933065505594978,1.0153136859126,1.09836343076413,
1.18141317561567,1.26373325194704,1.3454132435303,1.36175593088453,1.37449997082537,
1.45485338293641,1.53535345085992,1.61538859693277,1.69412331541584,1.74187144182578,
1.78111905912933,1.79651186347856,1.80847555122129,1.88768501760864,1.96689410761267,
2.04543359578892,2.05585238025418,2.07005430058833,2.14795915885765,2.22484263433871,
2.28089532743822,2.31010750305873),.UNSPECIFIED.);
#375=B_SPLINE_CURVE_WITH_KNOTS('',3,(#41877,#41878,#41879,#41880,#41881,
#41882,#41883,#41884,#41885,#41886,#41887,#41888,#41889,#41890,#41891,#41892,
#41893,#41894,#41895,#41896,#41897,#41898,#41899,#41900,#41901,#41902,#41903,
#41904,#41905,#41906,#41907,#41908,#41909,#41910,#41911,#41912,#41913,#41914,
#41915,#41916,#41917,#41918,#41919,#41920,#41921,#41922,#41923,#41924,#41925,
#41926,#41927,#41928,#41929,#41930,#41931,#41932,#41933,#41934,#41935,#41936,
#41937,#41938,#41939,#41940,#41941,#41942,#41943,#41944,#41945,#41946,#41947,
#41948,#41949,#41950,#41951,#41952,#41953,#41954,#41955,#41956,#41957,#41958,
#41959,#41960,#41961,#41962,#41963,#41964,#41965,#41966,#41967,#41968,#41969,
#41970,#41971,#41972,#41973,#41974,#41975,#41976,#41977,#41978,#41979,#41980,
#41981,#41982,#41983,#41984,#41985,#41986,#41987,#41988,#41989,#41990,#41991),
 .UNSPECIFIED.,.F.,.F.,(4,3,3,3,3,3,3,3,3,3,3,3,3,3,3,3,3,3,3,3,3,3,3,3,
3,3,3,3,3,3,3,3,3,3,3,3,3,3,4),(0.,0.0756021000860287,0.152393199413229,
0.230392842039223,0.308644925336307,0.386546669540438,0.408880923643587,
0.422045036141436,0.501691131541529,0.537249170842264,0.616137946028814,
0.695699298413659,0.775607582803438,0.834608203354004,0.843321085046558,
0.924172696188012,1.00955071586659,1.09492873554517,1.18019567138666,1.26546260722815,
1.27900992162839,1.28771744272705,1.3694636855273,1.45259721932159,1.53602421303522,
1.61905253984465,1.6726411664557,1.7128618032572,1.72976589346393,1.74248623587268,
1.82597852348531,1.91057121440841,1.99440626086767,2.0125183165509,2.02643670804109,
2.11207588022372,2.19783429700933,2.26933164573093,2.30291422475425),
 .UNSPECIFIED.);
#376=B_SPLINE_CURVE_WITH_KNOTS('',3,(#41992,#41993,#41994,#41995),
 .UNSPECIFIED.,.F.,.F.,(4,4),(-0.00101470513518961,0.),.UNSPECIFIED.);
#377=B_SPLINE_CURVE_WITH_KNOTS('',3,(#42360,#42361,#42362,#42363,#42364,
#42365,#42366,#42367,#42368,#42369,#42370,#42371,#42372,#42373,#42374,#42375,
#42376,#42377,#42378,#42379,#42380,#42381,#42382,#42383,#42384,#42385,#42386,
#42387,#42388,#42389,#42390,#42391,#42392,#42393,#42394,#42395,#42396,#42397,
#42398,#42399,#42400,#42401,#42402,#42403,#42404,#42405,#42406,#42407,#42408,
#42409,#42410,#42411,#42412,#42413,#42414,#42415,#42416,#42417,#42418,#42419,
#42420,#42421,#42422,#42423,#42424,#42425,#42426,#42427,#42428,#42429,#42430,
#42431,#42432,#42433,#42434,#42435,#42436,#42437,#42438,#42439,#42440,#42441,
#42442,#42443,#42444,#42445,#42446,#42447,#42448,#42449,#42450,#42451,#42452,
#42453,#42454,#42455,#42456,#42457,#42458,#42459,#42460,#42461,#42462,#42463,
#42464,#42465,#42466,#42467,#42468,#42469,#42470,#42471,#42472,#42473,#42474),
 .UNSPECIFIED.,.F.,.F.,(4,3,3,3,3,3,3,3,3,3,3,3,3,3,3,3,3,3,3,3,3,3,3,3,
3,3,3,3,3,3,3,3,3,3,3,3,3,3,4),(0.,0.0756020442574548,0.152393097282484,
0.230392716822797,0.308644794442198,0.386546558051837,0.408880856230141,
0.420928744427606,0.50056989933121,0.537249170842273,0.616073663427341,
0.695678467127519,0.775598187384106,0.815514505904238,0.834608291732455,
0.848410336526209,0.929311979470198,1.01212035750768,1.09492873554516,1.1760664859709,
1.25762667198288,1.27900990554167,1.28771743639829,1.3694636568822,1.45259718086404,
1.53602417093209,1.61905249850157,1.6726411664557,1.73231431654345,1.74174492869213,
1.82529436366377,1.90959642787817,1.99435898893753,2.01251832412271,2.02375496071478,
2.10938057767908,2.19514471613238,2.26933164573094,2.30291844692703),
 .UNSPECIFIED.);
#378=B_SPLINE_CURVE_WITH_KNOTS('',3,(#42475,#42476,#42477,#42478,#42479,
#42480,#42481,#42482,#42483,#42484,#42485,#42486,#42487,#42488,#42489,#42490,
#42491,#42492,#42493,#42494,#42495,#42496,#42497,#42498,#42499,#42500,#42501,
#42502,#42503,#42504,#42505,#42506,#42507,#42508,#42509,#42510,#42511,#42512,
#42513,#42514,#42515,#42516,#42517,#42518,#42519,#42520,#42521,#42522,#42523,
#42524,#42525,#42526,#42527,#42528,#42529,#42530,#42531,#42532,#42533,#42534,
#42535,#42536,#42537,#42538,#42539,#42540,#42541,#42542,#42543,#42544,#42545,
#42546,#42547,#42548,#42549,#42550,#42551,#42552,#42553,#42554,#42555,#42556,
#42557,#42558,#42559,#42560,#42561,#42562,#42563,#42564,#42565,#42566,#42567,
#42568,#42569,#42570,#42571,#42572,#42573,#42574,#42575,#42576,#42577,#42578,
#42579,#42580,#42581,#42582,#42583,#42584,#42585,#42586,#42587,#42588,#42589,
#42590,#42591,#42592,#42593,#42594,#42595,#42596,#42597,#42598),
 .UNSPECIFIED.,.F.,.F.,(4,3,3,3,3,3,3,3,3,3,3,3,3,3,3,3,3,3,3,3,3,3,3,3,
3,3,3,3,3,3,3,3,3,3,3,3,3,3,3,3,3,4),(6.61845341725208E-15,0.0849506171234813,
0.170583039080586,0.256324783642234,0.342404288458281,0.406963917070316,
0.455383638529342,0.468536166026273,0.479421865762467,0.563197401537396,
0.600642802906421,0.684641773439803,0.768646494241719,0.852075754316474,
0.893242931978871,0.912628999576665,0.923529204381824,0.932945920282631,
0.963808296830803,1.04604185775375,1.12763182076683,1.18141317561565,1.26548811560765,
1.34956305559966,1.36175593015859,1.37449997074551,1.45485337915234,1.53535344654489,
1.61538859022719,1.69412330072992,1.74187144182573,1.79625541798791,1.80632110746682,
1.88551239813011,1.96470047938476,2.04374919139812,2.05752087843184,2.07312514683444,
2.15101428972444,2.22787487685276,2.28089532743819,2.31010750305869),
 .UNSPECIFIED.);
#379=FACE_BOUND('',#851,.T.);
#380=FACE_BOUND('',#854,.T.);
#381=FACE_BOUND('',#859,.T.);
#382=FACE_BOUND('',#863,.T.);
#383=FACE_BOUND('',#866,.T.);
#384=FACE_BOUND('',#868,.T.);
#385=FACE_BOUND('',#870,.T.);
#386=FACE_BOUND('',#872,.T.);
#387=FACE_BOUND('',#884,.T.);
#388=FACE_BOUND('',#912,.T.);
#389=FACE_BOUND('',#920,.T.);
#390=FACE_BOUND('',#959,.T.);
#391=FACE_BOUND('',#967,.T.);
#392=FACE_BOUND('',#1020,.T.);
#393=FACE_BOUND('',#1022,.T.);
#394=FACE_BOUND('',#1042,.T.);
#395=FACE_BOUND('',#1050,.T.);
#396=CYLINDRICAL_SURFACE('',#4166,9.);
#397=CYLINDRICAL_SURFACE('',#4178,7.5);
#398=CYLINDRICAL_SURFACE('',#4179,19.);
#399=CYLINDRICAL_SURFACE('',#4182,6.);
#400=CYLINDRICAL_SURFACE('',#4183,15.);
#401=CYLINDRICAL_SURFACE('',#4188,15.);
#402=CYLINDRICAL_SURFACE('',#4193,12.);
#403=CYLINDRICAL_SURFACE('',#4197,1.5);
#404=CYLINDRICAL_SURFACE('',#4204,1.5);
#405=CYLINDRICAL_SURFACE('',#4207,11.);
#406=CYLINDRICAL_SURFACE('',#4210,1.5);
#407=CYLINDRICAL_SURFACE('',#4216,1.5);
#408=CYLINDRICAL_SURFACE('',#4220,30.);
#409=CYLINDRICAL_SURFACE('',#4224,30.);
#410=CYLINDRICAL_SURFACE('',#4236,12.1745);
#411=CYLINDRICAL_SURFACE('',#4238,12.1745);
#412=CYLINDRICAL_SURFACE('',#4240,12.1745);
#413=CYLINDRICAL_SURFACE('',#4241,12.1745);
#414=CYLINDRICAL_SURFACE('',#4242,12.1745);
#415=CYLINDRICAL_SURFACE('',#4243,12.1745);
#416=CYLINDRICAL_SURFACE('',#4244,12.1745);
#417=CYLINDRICAL_SURFACE('',#4245,10.501);
#418=CYLINDRICAL_SURFACE('',#4247,10.501);
#419=CYLINDRICAL_SURFACE('',#4248,10.501);
#420=CYLINDRICAL_SURFACE('',#4249,10.501);
#421=CYLINDRICAL_SURFACE('',#4250,10.501);
#422=CYLINDRICAL_SURFACE('',#4251,10.501);
#423=CYLINDRICAL_SURFACE('',#4252,10.501);
#424=CYLINDRICAL_SURFACE('',#4254,12.1745);
#425=CYLINDRICAL_SURFACE('',#4265,3.22275);
#426=CYLINDRICAL_SURFACE('',#4267,3.22275);
#427=CYLINDRICAL_SURFACE('',#4268,3.22275);
#428=CYLINDRICAL_SURFACE('',#4269,3.22275);
#429=CYLINDRICAL_SURFACE('',#4270,3.22275);
#430=CYLINDRICAL_SURFACE('',#4271,3.22275);
#431=CYLINDRICAL_SURFACE('',#4272,3.22275);
#432=CYLINDRICAL_SURFACE('',#4273,3.22275);
#433=CYLINDRICAL_SURFACE('',#4274,3.22275);
#434=CYLINDRICAL_SURFACE('',#4275,3.22275);
#435=CYLINDRICAL_SURFACE('',#4276,3.22275);
#436=CYLINDRICAL_SURFACE('',#4277,3.22275);
#437=CYLINDRICAL_SURFACE('',#4278,3.22275);
#438=CYLINDRICAL_SURFACE('',#4279,3.22275);
#439=CYLINDRICAL_SURFACE('',#4280,3.22275);
#440=CYLINDRICAL_SURFACE('',#4281,3.22275);
#441=CYLINDRICAL_SURFACE('',#4282,3.22275);
#442=CYLINDRICAL_SURFACE('',#4283,3.22275);
#443=CYLINDRICAL_SURFACE('',#4284,3.22275);
#444=CYLINDRICAL_SURFACE('',#4285,3.22275);
#445=CYLINDRICAL_SURFACE('',#4286,3.22275);
#446=CYLINDRICAL_SURFACE('',#4287,3.22275);
#447=CYLINDRICAL_SURFACE('',#4288,3.22275);
#448=CYLINDRICAL_SURFACE('',#4289,3.22275);
#449=CYLINDRICAL_SURFACE('',#4290,3.22275);
#450=CYLINDRICAL_SURFACE('',#4291,3.22275);
#451=CYLINDRICAL_SURFACE('',#4292,3.22275);
#452=CYLINDRICAL_SURFACE('',#4293,3.22275);
#453=CYLINDRICAL_SURFACE('',#4294,3.933);
#454=CYLINDRICAL_SURFACE('',#4297,3.22275);
#455=CYLINDRICAL_SURFACE('',#4306,4.);
#456=CYLINDRICAL_SURFACE('',#4318,3.933);
#457=CYLINDRICAL_SURFACE('',#4320,3.933);
#458=CYLINDRICAL_SURFACE('',#4322,3.22275);
#459=CYLINDRICAL_SURFACE('',#4324,3.22275);
#460=CYLINDRICAL_SURFACE('',#4325,3.22275);
#461=CYLINDRICAL_SURFACE('',#4327,3.22275);
#462=CYLINDRICAL_SURFACE('',#4329,3.933);
#463=CYLINDRICAL_SURFACE('',#4335,0.5);
#464=CYLINDRICAL_SURFACE('',#4341,0.5);
#465=CYLINDRICAL_SURFACE('',#4347,0.5);
#466=CYLINDRICAL_SURFACE('',#4353,0.5);
#467=CYLINDRICAL_SURFACE('',#4359,0.5);
#468=CYLINDRICAL_SURFACE('',#4365,0.5);
#469=CYLINDRICAL_SURFACE('',#4371,0.5);
#470=CYLINDRICAL_SURFACE('',#4372,8.);
#471=CYLINDRICAL_SURFACE('',#4375,8.);
#472=CYLINDRICAL_SURFACE('',#4381,5.);
#473=CYLINDRICAL_SURFACE('',#4383,5.);
#474=CYLINDRICAL_SURFACE('',#4389,0.5);
#475=CYLINDRICAL_SURFACE('',#4395,0.5);
#476=CYLINDRICAL_SURFACE('',#4400,0.5);
#477=CYLINDRICAL_SURFACE('',#4405,0.5);
#478=CYLINDRICAL_SURFACE('',#4410,0.5);
#479=CYLINDRICAL_SURFACE('',#4415,0.5);
#480=CYLINDRICAL_SURFACE('',#4421,0.5);
#481=CYLINDRICAL_SURFACE('',#4423,5.);
#482=CYLINDRICAL_SURFACE('',#4425,5.);
#483=CYLINDRICAL_SURFACE('',#4427,10.);
#484=CYLINDRICAL_SURFACE('',#4431,12.1745);
#485=CYLINDRICAL_SURFACE('',#4433,12.1745);
#486=CYLINDRICAL_SURFACE('',#4434,12.1745);
#487=CYLINDRICAL_SURFACE('',#4435,12.1745);
#488=CYLINDRICAL_SURFACE('',#4436,12.1745);
#489=CYLINDRICAL_SURFACE('',#4437,12.1745);
#490=CYLINDRICAL_SURFACE('',#4438,12.1745);
#491=CYLINDRICAL_SURFACE('',#4440,10.501);
#492=CYLINDRICAL_SURFACE('',#4442,10.501);
#493=CYLINDRICAL_SURFACE('',#4443,10.501);
#494=CYLINDRICAL_SURFACE('',#4444,10.501);
#495=CYLINDRICAL_SURFACE('',#4445,10.501);
#496=CYLINDRICAL_SURFACE('',#4446,10.501);
#497=CYLINDRICAL_SURFACE('',#4447,10.501);
#498=CYLINDRICAL_SURFACE('',#4449,10.501);
#499=CYLINDRICAL_SURFACE('',#4450,12.1745);
#500=TOROIDAL_SURFACE('',#4162,8.5,0.5);
#501=TOROIDAL_SURFACE('',#4169,8.5,0.5);
#502=TOROIDAL_SURFACE('',#4174,8.,0.5);
#503=TOROIDAL_SURFACE('',#4200,9.5,1.5);
#504=TOROIDAL_SURFACE('',#4213,9.5,1.5);
#505=TOROIDAL_SURFACE('',#4330,5.5,0.5);
#506=TOROIDAL_SURFACE('',#4337,4.5,0.5);
#507=TOROIDAL_SURFACE('',#4343,7.5,0.5);
#508=TOROIDAL_SURFACE('',#4349,7.5,0.5);
#509=TOROIDAL_SURFACE('',#4355,4.5,0.5);
#510=TOROIDAL_SURFACE('',#4361,5.5,0.5);
#511=TOROIDAL_SURFACE('',#4367,9.5,0.5);
#512=TOROIDAL_SURFACE('',#4384,4.5,0.5);
#513=TOROIDAL_SURFACE('',#4391,5.5,0.5);
#514=TOROIDAL_SURFACE('',#4397,7.5,0.5);
#515=TOROIDAL_SURFACE('',#4402,7.5,0.5);
#516=TOROIDAL_SURFACE('',#4407,5.5,0.5);
#517=TOROIDAL_SURFACE('',#4412,4.5,0.5);
#518=TOROIDAL_SURFACE('',#4417,9.5,0.5);
#519=CIRCLE('',#4148,6.);
#520=CIRCLE('',#4150,6.);
#521=CIRCLE('',#4152,6.);
#522=CIRCLE('',#4154,6.);
#523=CIRCLE('',#4156,6.);
#524=CIRCLE('',#4158,6.);
#525=CIRCLE('',#4159,6.);
#526=CIRCLE('',#4163,8.5);
#527=CIRCLE('',#4164,0.5);
#528=CIRCLE('',#4165,9.);
#529=CIRCLE('',#4167,9.);
#530=CIRCLE('',#4170,0.5);
#531=CIRCLE('',#4171,8.5);
#532=CIRCLE('',#4173,8.);
#533=CIRCLE('',#4175,7.5);
#534=CIRCLE('',#4176,0.5);
#535=CIRCLE('',#4177,7.5);
#536=CIRCLE('',#4180,19.);
#537=CIRCLE('',#4181,19.);
#538=CIRCLE('',#4184,15.);
#539=CIRCLE('',#4185,15.);
#540=CIRCLE('',#4187,12.);
#541=CIRCLE('',#4189,15.);
#542=CIRCLE('',#4190,15.);
#543=CIRCLE('',#4192,12.);
#544=CIRCLE('',#4198,1.5);
#545=CIRCLE('',#4199,1.5);
#546=CIRCLE('',#4201,1.5);
#547=CIRCLE('',#4202,11.);
#548=CIRCLE('',#4203,9.5);
#549=CIRCLE('',#4205,1.5);
#550=CIRCLE('',#4208,11.);
#551=CIRCLE('',#4211,1.5);
#552=CIRCLE('',#4212,1.5);
#553=CIRCLE('',#4214,1.5);
#554=CIRCLE('',#4215,9.5);
#555=CIRCLE('',#4217,1.5);
#556=CIRCLE('',#4221,30.);
#557=CIRCLE('',#4222,30.);
#558=CIRCLE('',#4225,30.);
#559=CIRCLE('',#4226,30.);
#560=CIRCLE('',#4233,9.1643052178268);
#561=CIRCLE('',#4237,12.1745);
#562=CIRCLE('',#4239,12.1745);
#563=CIRCLE('',#4246,10.501);
#564=CIRCLE('',#4253,10.501);
#565=CIRCLE('',#4255,12.1745);
#566=CIRCLE('',#4266,3.22275);
#567=CIRCLE('',#4295,3.933);
#568=CIRCLE('',#4296,3.933);
#569=CIRCLE('',#4298,3.22275);
#570=CIRCLE('',#4303,9.1643052178268);
#571=CIRCLE('',#4307,4.);
#572=CIRCLE('',#4308,4.);
#573=CIRCLE('',#4319,3.933);
#574=CIRCLE('',#4321,3.933);
#575=CIRCLE('',#4323,3.22275);
#576=CIRCLE('',#4326,3.22275);
#577=CIRCLE('',#4328,3.22275);
#578=CIRCLE('',#4331,0.500000000000007);
#579=CIRCLE('',#4332,5.5);
#580=CIRCLE('',#4333,0.5);
#581=CIRCLE('',#4334,5.);
#582=CIRCLE('',#4336,0.5);
#583=CIRCLE('',#4338,0.5);
#584=CIRCLE('',#4339,5.);
#585=CIRCLE('',#4340,4.5);
#586=CIRCLE('',#4342,0.5);
#587=CIRCLE('',#4344,0.500000000000003);
#588=CIRCLE('',#4345,7.5);
#589=CIRCLE('',#4346,8.);
#590=CIRCLE('',#4348,0.5);
#591=CIRCLE('',#4350,0.500000000000003);
#592=CIRCLE('',#4351,7.5);
#593=CIRCLE('',#4352,8.);
#594=CIRCLE('',#4354,0.5);
#595=CIRCLE('',#4356,0.5);
#596=CIRCLE('',#4357,5.);
#597=CIRCLE('',#4358,4.5);
#598=CIRCLE('',#4360,0.5);
#599=CIRCLE('',#4362,0.5);
#600=CIRCLE('',#4363,5.);
#601=CIRCLE('',#4364,5.5);
#602=CIRCLE('',#4366,0.5);
#603=CIRCLE('',#4368,0.500000000000002);
#604=CIRCLE('',#4369,9.5);
#605=CIRCLE('',#4370,10.);
#606=CIRCLE('',#4373,8.);
#607=CIRCLE('',#4376,8.);
#608=CIRCLE('',#4378,4.5);
#609=CIRCLE('',#4379,5.5);
#610=CIRCLE('',#4385,0.500000000000007);
#611=CIRCLE('',#4386,4.5);
#612=CIRCLE('',#4387,0.5);
#613=CIRCLE('',#4388,5.);
#614=CIRCLE('',#4390,0.5);
#615=CIRCLE('',#4392,0.5);
#616=CIRCLE('',#4393,5.);
#617=CIRCLE('',#4394,5.5);
#618=CIRCLE('',#4396,0.5);
#619=CIRCLE('',#4398,0.500000000000003);
#620=CIRCLE('',#4399,7.5);
#621=CIRCLE('',#4401,0.5);
#622=CIRCLE('',#4403,0.500000000000003);
#623=CIRCLE('',#4404,7.5);
#624=CIRCLE('',#4406,0.5);
#625=CIRCLE('',#4408,0.5);
#626=CIRCLE('',#4409,5.);
#627=CIRCLE('',#4411,0.5);
#628=CIRCLE('',#4413,0.5);
#629=CIRCLE('',#4414,5.);
#630=CIRCLE('',#4416,0.5);
#631=CIRCLE('',#4418,0.500000000000002);
#632=CIRCLE('',#4419,9.5);
#633=CIRCLE('',#4420,10.);
#634=CIRCLE('',#4432,12.1745);
#635=CIRCLE('',#4439,12.1745);
#636=CIRCLE('',#4441,10.501);
#637=CIRCLE('',#4448,10.501);
#638=FACE_OUTER_BOUND('',#836,.T.);
#639=FACE_OUTER_BOUND('',#837,.T.);
#640=FACE_OUTER_BOUND('',#838,.T.);
#641=FACE_OUTER_BOUND('',#839,.T.);
#642=FACE_OUTER_BOUND('',#840,.T.);
#643=FACE_OUTER_BOUND('',#841,.T.);
#644=FACE_OUTER_BOUND('',#842,.T.);
#645=FACE_OUTER_BOUND('',#843,.T.);
#646=FACE_OUTER_BOUND('',#844,.T.);
#647=FACE_OUTER_BOUND('',#845,.T.);
#648=FACE_OUTER_BOUND('',#846,.T.);
#649=FACE_OUTER_BOUND('',#847,.T.);
#650=FACE_OUTER_BOUND('',#848,.T.);
#651=FACE_OUTER_BOUND('',#849,.T.);
#652=FACE_OUTER_BOUND('',#850,.T.);
#653=FACE_OUTER_BOUND('',#852,.T.);
#654=FACE_OUTER_BOUND('',#853,.T.);
#655=FACE_OUTER_BOUND('',#855,.T.);
#656=FACE_OUTER_BOUND('',#856,.T.);
#657=FACE_OUTER_BOUND('',#857,.T.);
#658=FACE_OUTER_BOUND('',#858,.T.);
#659=FACE_OUTER_BOUND('',#860,.T.);
#660=FACE_OUTER_BOUND('',#861,.T.);
#661=FACE_OUTER_BOUND('',#862,.T.);
#662=FACE_OUTER_BOUND('',#864,.T.);
#663=FACE_OUTER_BOUND('',#865,.T.);
#664=FACE_OUTER_BOUND('',#867,.T.);
#665=FACE_OUTER_BOUND('',#869,.T.);
#666=FACE_OUTER_BOUND('',#871,.T.);
#667=FACE_OUTER_BOUND('',#873,.T.);
#668=FACE_OUTER_BOUND('',#874,.T.);
#669=FACE_OUTER_BOUND('',#875,.T.);
#670=FACE_OUTER_BOUND('',#876,.T.);
#671=FACE_OUTER_BOUND('',#877,.T.);
#672=FACE_OUTER_BOUND('',#878,.T.);
#673=FACE_OUTER_BOUND('',#879,.T.);
#674=FACE_OUTER_BOUND('',#880,.T.);
#675=FACE_OUTER_BOUND('',#881,.T.);
#676=FACE_OUTER_BOUND('',#882,.T.);
#677=FACE_OUTER_BOUND('',#883,.T.);
#678=FACE_OUTER_BOUND('',#885,.T.);
#679=FACE_OUTER_BOUND('',#886,.T.);
#680=FACE_OUTER_BOUND('',#887,.T.);
#681=FACE_OUTER_BOUND('',#888,.T.);
#682=FACE_OUTER_BOUND('',#889,.T.);
#683=FACE_OUTER_BOUND('',#890,.T.);
#684=FACE_OUTER_BOUND('',#891,.T.);
#685=FACE_OUTER_BOUND('',#892,.T.);
#686=FACE_OUTER_BOUND('',#893,.T.);
#687=FACE_OUTER_BOUND('',#894,.T.);
#688=FACE_OUTER_BOUND('',#895,.T.);
#689=FACE_OUTER_BOUND('',#896,.T.);
#690=FACE_OUTER_BOUND('',#897,.T.);
#691=FACE_OUTER_BOUND('',#898,.T.);
#692=FACE_OUTER_BOUND('',#899,.T.);
#693=FACE_OUTER_BOUND('',#900,.T.);
#694=FACE_OUTER_BOUND('',#901,.T.);
#695=FACE_OUTER_BOUND('',#902,.T.);
#696=FACE_OUTER_BOUND('',#903,.T.);
#697=FACE_OUTER_BOUND('',#904,.T.);
#698=FACE_OUTER_BOUND('',#905,.T.);
#699=FACE_OUTER_BOUND('',#906,.T.);
#700=FACE_OUTER_BOUND('',#907,.T.);
#701=FACE_OUTER_BOUND('',#908,.T.);
#702=FACE_OUTER_BOUND('',#909,.T.);
#703=FACE_OUTER_BOUND('',#910,.T.);
#704=FACE_OUTER_BOUND('',#911,.T.);
#705=FACE_OUTER_BOUND('',#913,.T.);
#706=FACE_OUTER_BOUND('',#914,.T.);
#707=FACE_OUTER_BOUND('',#915,.T.);
#708=FACE_OUTER_BOUND('',#916,.T.);
#709=FACE_OUTER_BOUND('',#917,.T.);
#710=FACE_OUTER_BOUND('',#918,.T.);
#711=FACE_OUTER_BOUND('',#919,.T.);
#712=FACE_OUTER_BOUND('',#921,.T.);
#713=FACE_OUTER_BOUND('',#922,.T.);
#714=FACE_OUTER_BOUND('',#923,.T.);
#715=FACE_OUTER_BOUND('',#924,.T.);
#716=FACE_OUTER_BOUND('',#925,.T.);
#717=FACE_OUTER_BOUND('',#926,.T.);
#718=FACE_OUTER_BOUND('',#927,.T.);
#719=FACE_OUTER_BOUND('',#928,.T.);
#720=FACE_OUTER_BOUND('',#929,.T.);
#721=FACE_OUTER_BOUND('',#930,.T.);
#722=FACE_OUTER_BOUND('',#931,.T.);
#723=FACE_OUTER_BOUND('',#932,.T.);
#724=FACE_OUTER_BOUND('',#933,.T.);
#725=FACE_OUTER_BOUND('',#934,.T.);
#726=FACE_OUTER_BOUND('',#935,.T.);
#727=FACE_OUTER_BOUND('',#936,.T.);
#728=FACE_OUTER_BOUND('',#937,.T.);
#729=FACE_OUTER_BOUND('',#938,.T.);
#730=FACE_OUTER_BOUND('',#939,.T.);
#731=FACE_OUTER_BOUND('',#940,.T.);
#732=FACE_OUTER_BOUND('',#941,.T.);
#733=FACE_OUTER_BOUND('',#942,.T.);
#734=FACE_OUTER_BOUND('',#943,.T.);
#735=FACE_OUTER_BOUND('',#944,.T.);
#736=FACE_OUTER_BOUND('',#945,.T.);
#737=FACE_OUTER_BOUND('',#946,.T.);
#738=FACE_OUTER_BOUND('',#947,.T.);
#739=FACE_OUTER_BOUND('',#948,.T.);
#740=FACE_OUTER_BOUND('',#949,.T.);
#741=FACE_OUTER_BOUND('',#950,.T.);
#742=FACE_OUTER_BOUND('',#951,.T.);
#743=FACE_OUTER_BOUND('',#952,.T.);
#744=FACE_OUTER_BOUND('',#953,.T.);
#745=FACE_OUTER_BOUND('',#954,.T.);
#746=FACE_OUTER_BOUND('',#955,.T.);
#747=FACE_OUTER_BOUND('',#956,.T.);
#748=FACE_OUTER_BOUND('',#957,.T.);
#749=FACE_OUTER_BOUND('',#958,.T.);
#750=FACE_OUTER_BOUND('',#960,.T.);
#751=FACE_OUTER_BOUND('',#961,.T.);
#752=FACE_OUTER_BOUND('',#962,.T.);
#753=FACE_OUTER_BOUND('',#963,.T.);
#754=FACE_OUTER_BOUND('',#964,.T.);
#755=FACE_OUTER_BOUND('',#965,.T.);
#756=FACE_OUTER_BOUND('',#966,.T.);
#757=FACE_OUTER_BOUND('',#968,.T.);
#758=FACE_OUTER_BOUND('',#969,.T.);
#759=FACE_OUTER_BOUND('',#970,.T.);
#760=FACE_OUTER_BOUND('',#971,.T.);
#761=FACE_OUTER_BOUND('',#972,.T.);
#762=FACE_OUTER_BOUND('',#973,.T.);
#763=FACE_OUTER_BOUND('',#974,.T.);
#764=FACE_OUTER_BOUND('',#975,.T.);
#765=FACE_OUTER_BOUND('',#976,.T.);
#766=FACE_OUTER_BOUND('',#977,.T.);
#767=FACE_OUTER_BOUND('',#978,.T.);
#768=FACE_OUTER_BOUND('',#979,.T.);
#769=FACE_OUTER_BOUND('',#980,.T.);
#770=FACE_OUTER_BOUND('',#981,.T.);
#771=FACE_OUTER_BOUND('',#982,.T.);
#772=FACE_OUTER_BOUND('',#983,.T.);
#773=FACE_OUTER_BOUND('',#984,.T.);
#774=FACE_OUTER_BOUND('',#985,.T.);
#775=FACE_OUTER_BOUND('',#986,.T.);
#776=FACE_OUTER_BOUND('',#987,.T.);
#777=FACE_OUTER_BOUND('',#988,.T.);
#778=FACE_OUTER_BOUND('',#989,.T.);
#779=FACE_OUTER_BOUND('',#990,.T.);
#780=FACE_OUTER_BOUND('',#991,.T.);
#781=FACE_OUTER_BOUND('',#992,.T.);
#782=FACE_OUTER_BOUND('',#993,.T.);
#783=FACE_OUTER_BOUND('',#994,.T.);
#784=FACE_OUTER_BOUND('',#995,.T.);
#785=FACE_OUTER_BOUND('',#996,.T.);
#786=FACE_OUTER_BOUND('',#997,.T.);
#787=FACE_OUTER_BOUND('',#998,.T.);
#788=FACE_OUTER_BOUND('',#999,.T.);
#789=FACE_OUTER_BOUND('',#1000,.T.);
#790=FACE_OUTER_BOUND('',#1001,.T.);
#791=FACE_OUTER_BOUND('',#1002,.T.);
#792=FACE_OUTER_BOUND('',#1003,.T.);
#793=FACE_OUTER_BOUND('',#1004,.T.);
#794=FACE_OUTER_BOUND('',#1005,.T.);
#795=FACE_OUTER_BOUND('',#1006,.T.);
#796=FACE_OUTER_BOUND('',#1007,.T.);
#797=FACE_OUTER_BOUND('',#1008,.T.);
#798=FACE_OUTER_BOUND('',#1009,.T.);
#799=FACE_OUTER_BOUND('',#1010,.T.);
#800=FACE_OUTER_BOUND('',#1011,.T.);
#801=FACE_OUTER_BOUND('',#1012,.T.);
#802=FACE_OUTER_BOUND('',#1013,.T.);
#803=FACE_OUTER_BOUND('',#1014,.T.);
#804=FACE_OUTER_BOUND('',#1015,.T.);
#805=FACE_OUTER_BOUND('',#1016,.T.);
#806=FACE_OUTER_BOUND('',#1017,.T.);
#807=FACE_OUTER_BOUND('',#1018,.T.);
#808=FACE_OUTER_BOUND('',#1019,.T.);
#809=FACE_OUTER_BOUND('',#1021,.T.);
#810=FACE_OUTER_BOUND('',#1023,.T.);
#811=FACE_OUTER_BOUND('',#1024,.T.);
#812=FACE_OUTER_BOUND('',#1025,.T.);
#813=FACE_OUTER_BOUND('',#1026,.T.);
#814=FACE_OUTER_BOUND('',#1027,.T.);
#815=FACE_OUTER_BOUND('',#1028,.T.);
#816=FACE_OUTER_BOUND('',#1029,.T.);
#817=FACE_OUTER_BOUND('',#1030,.T.);
#818=FACE_OUTER_BOUND('',#1031,.T.);
#819=FACE_OUTER_BOUND('',#1032,.T.);
#820=FACE_OUTER_BOUND('',#1033,.T.);
#821=FACE_OUTER_BOUND('',#1034,.T.);
#822=FACE_OUTER_BOUND('',#1035,.T.);
#823=FACE_OUTER_BOUND('',#1036,.T.);
#824=FACE_OUTER_BOUND('',#1037,.T.);
#825=FACE_OUTER_BOUND('',#1038,.T.);
#826=FACE_OUTER_BOUND('',#1039,.T.);
#827=FACE_OUTER_BOUND('',#1040,.T.);
#828=FACE_OUTER_BOUND('',#1041,.T.);
#829=FACE_OUTER_BOUND('',#1043,.T.);
#830=FACE_OUTER_BOUND('',#1044,.T.);
#831=FACE_OUTER_BOUND('',#1045,.T.);
#832=FACE_OUTER_BOUND('',#1046,.T.);
#833=FACE_OUTER_BOUND('',#1047,.T.);
#834=FACE_OUTER_BOUND('',#1048,.T.);
#835=FACE_OUTER_BOUND('',#1049,.T.);
#836=EDGE_LOOP('',(#2536,#2537,#2538,#2539,#2540));
#837=EDGE_LOOP('',(#2541,#2542,#2543,#2544,#2545));
#838=EDGE_LOOP('',(#2546,#2547,#2548,#2549,#2550));
#839=EDGE_LOOP('',(#2551,#2552,#2553,#2554,#2555));
#840=EDGE_LOOP('',(#2556,#2557,#2558));
#841=EDGE_LOOP('',(#2559,#2560,#2561));
#842=EDGE_LOOP('',(#2562,#2563,#2564));
#843=EDGE_LOOP('',(#2565,#2566,#2567));
#844=EDGE_LOOP('',(#2568,#2569,#2570));
#845=EDGE_LOOP('',(#2571,#2572,#2573,#2574));
#846=EDGE_LOOP('',(#2575,#2576,#2577,#2578,#2579));
#847=EDGE_LOOP('',(#2580,#2581,#2582,#2583,#2584));
#848=EDGE_LOOP('',(#2585,#2586,#2587,#2588));
#849=EDGE_LOOP('',(#2589,#2590,#2591,#2592));
#850=EDGE_LOOP('',(#2593));
#851=EDGE_LOOP('',(#2594,#2595,#2596,#2597,#2598,#2599));
#852=EDGE_LOOP('',(#2600,#2601,#2602,#2603));
#853=EDGE_LOOP('',(#2604));
#854=EDGE_LOOP('',(#2605));
#855=EDGE_LOOP('',(#2606,#2607,#2608,#2609,#2610));
#856=EDGE_LOOP('',(#2611,#2612,#2613,#2614,#2615,#2616));
#857=EDGE_LOOP('',(#2617,#2618,#2619,#2620,#2621));
#858=EDGE_LOOP('',(#2622,#2623,#2624,#2625));
#859=EDGE_LOOP('',(#2626));
#860=EDGE_LOOP('',(#2627,#2628,#2629,#2630,#2631,#2632,#2633,#2634,#2635,
#2636,#2637));
#861=EDGE_LOOP('',(#2638,#2639,#2640,#2641));
#862=EDGE_LOOP('',(#2642));
#863=EDGE_LOOP('',(#2643));
#864=EDGE_LOOP('',(#2644,#2645,#2646,#2647));
#865=EDGE_LOOP('',(#2648));
#866=EDGE_LOOP('',(#2649));
#867=EDGE_LOOP('',(#2650,#2651,#2652,#2653));
#868=EDGE_LOOP('',(#2654,#2655));
#869=EDGE_LOOP('',(#2656));
#870=EDGE_LOOP('',(#2657));
#871=EDGE_LOOP('',(#2658));
#872=EDGE_LOOP('',(#2659));
#873=EDGE_LOOP('',(#2660,#2661,#2662,#2663));
#874=EDGE_LOOP('',(#2664,#2665,#2666,#2667));
#875=EDGE_LOOP('',(#2668,#2669,#2670,#2671));
#876=EDGE_LOOP('',(#2672,#2673,#2674,#2675));
#877=EDGE_LOOP('',(#2676,#2677,#2678,#2679));
#878=EDGE_LOOP('',(#2680,#2681,#2682,#2683));
#879=EDGE_LOOP('',(#2684,#2685,#2686,#2687));
#880=EDGE_LOOP('',(#2688,#2689,#2690,#2691));
#881=EDGE_LOOP('',(#2692,#2693,#2694,#2695));
#882=EDGE_LOOP('',(#2696,#2697,#2698,#2699));
#883=EDGE_LOOP('',(#2700,#2701,#2702,#2703,#2704,#2705,#2706,#2707));
#884=EDGE_LOOP('',(#2708,#2709,#2710,#2711));
#885=EDGE_LOOP('',(#2712,#2713,#2714,#2715));
#886=EDGE_LOOP('',(#2716,#2717,#2718,#2719));
#887=EDGE_LOOP('',(#2720,#2721,#2722,#2723));
#888=EDGE_LOOP('',(#2724,#2725,#2726,#2727,#2728));
#889=EDGE_LOOP('',(#2729,#2730,#2731,#2732));
#890=EDGE_LOOP('',(#2733,#2734,#2735,#2736,#2737));
#891=EDGE_LOOP('',(#2738,#2739,#2740,#2741));
#892=EDGE_LOOP('',(#2742));
#893=EDGE_LOOP('',(#2743));
#894=EDGE_LOOP('',(#2744,#2745,#2746));
#895=EDGE_LOOP('',(#2747,#2748,#2749,#2750,#2751,#2752,#2753));
#896=EDGE_LOOP('',(#2754,#2755,#2756,#2757,#2758,#2759));
#897=EDGE_LOOP('',(#2760,#2761,#2762,#2763,#2764,#2765));
#898=EDGE_LOOP('',(#2766,#2767,#2768,#2769,#2770,#2771));
#899=EDGE_LOOP('',(#2772,#2773,#2774,#2775,#2776,#2777));
#900=EDGE_LOOP('',(#2778,#2779,#2780,#2781,#2782,#2783));
#901=EDGE_LOOP('',(#2784,#2785,#2786,#2787,#2788));
#902=EDGE_LOOP('',(#2789,#2790,#2791,#2792,#2793));
#903=EDGE_LOOP('',(#2794,#2795,#2796,#2797));
#904=EDGE_LOOP('',(#2798,#2799,#2800,#2801,#2802));
#905=EDGE_LOOP('',(#2803,#2804,#2805,#2806));
#906=EDGE_LOOP('',(#2807,#2808,#2809,#2810,#2811));
#907=EDGE_LOOP('',(#2812,#2813,#2814,#2815));
#908=EDGE_LOOP('',(#2816,#2817,#2818,#2819,#2820,#2821));
#909=EDGE_LOOP('',(#2822,#2823,#2824,#2825,#2826,#2827,#2828,#2829,#2830,
#2831,#2832,#2833,#2834,#2835,#2836,#2837,#2838,#2839,#2840,#2841,#2842,
#2843,#2844,#2845,#2846));
#910=EDGE_LOOP('',(#2847,#2848,#2849,#2850,#2851,#2852,#2853,#2854,#2855,
#2856,#2857,#2858,#2859,#2860,#2861,#2862,#2863,#2864,#2865,#2866,#2867,
#2868,#2869,#2870,#2871,#2872,#2873));
#911=EDGE_LOOP('',(#2874,#2875,#2876,#2877,#2878,#2879));
#912=EDGE_LOOP('',(#2880,#2881,#2882,#2883,#2884));
#913=EDGE_LOOP('',(#2885,#2886,#2887,#2888));
#914=EDGE_LOOP('',(#2889,#2890,#2891,#2892));
#915=EDGE_LOOP('',(#2893,#2894,#2895,#2896));
#916=EDGE_LOOP('',(#2897,#2898,#2899,#2900));
#917=EDGE_LOOP('',(#2901,#2902,#2903,#2904));
#918=EDGE_LOOP('',(#2905,#2906,#2907,#2908));
#919=EDGE_LOOP('',(#2909,#2910,#2911,#2912,#2913,#2914));
#920=EDGE_LOOP('',(#2915,#2916,#2917,#2918,#2919));
#921=EDGE_LOOP('',(#2920,#2921,#2922,#2923));
#922=EDGE_LOOP('',(#2924,#2925,#2926,#2927,#2928,#2929));
#923=EDGE_LOOP('',(#2930,#2931,#2932,#2933));
#924=EDGE_LOOP('',(#2934,#2935,#2936,#2937,#2938,#2939));
#925=EDGE_LOOP('',(#2940,#2941,#2942,#2943,#2944));
#926=EDGE_LOOP('',(#2945,#2946,#2947,#2948,#2949));
#927=EDGE_LOOP('',(#2950,#2951,#2952,#2953,#2954));
#928=EDGE_LOOP('',(#2955,#2956,#2957,#2958,#2959));
#929=EDGE_LOOP('',(#2960,#2961,#2962,#2963,#2964));
#930=EDGE_LOOP('',(#2965,#2966,#2967,#2968,#2969));
#931=EDGE_LOOP('',(#2970,#2971,#2972,#2973,#2974));
#932=EDGE_LOOP('',(#2975,#2976,#2977,#2978,#2979));
#933=EDGE_LOOP('',(#2980,#2981,#2982,#2983,#2984,#2985));
#934=EDGE_LOOP('',(#2986,#2987,#2988,#2989));
#935=EDGE_LOOP('',(#2990,#2991,#2992,#2993,#2994,#2995));
#936=EDGE_LOOP('',(#2996,#2997,#2998,#2999));
#937=EDGE_LOOP('',(#3000,#3001,#3002,#3003,#3004,#3005));
#938=EDGE_LOOP('',(#3006,#3007,#3008,#3009,#3010));
#939=EDGE_LOOP('',(#3011,#3012,#3013,#3014,#3015));
#940=EDGE_LOOP('',(#3016,#3017,#3018,#3019,#3020));
#941=EDGE_LOOP('',(#3021,#3022,#3023,#3024,#3025));
#942=EDGE_LOOP('',(#3026,#3027,#3028,#3029,#3030));
#943=EDGE_LOOP('',(#3031,#3032,#3033,#3034,#3035));
#944=EDGE_LOOP('',(#3036,#3037,#3038,#3039,#3040));
#945=EDGE_LOOP('',(#3041,#3042,#3043,#3044,#3045));
#946=EDGE_LOOP('',(#3046,#3047,#3048,#3049,#3050,#3051));
#947=EDGE_LOOP('',(#3052,#3053,#3054,#3055));
#948=EDGE_LOOP('',(#3056,#3057,#3058,#3059,#3060,#3061));
#949=EDGE_LOOP('',(#3062,#3063,#3064,#3065,#3066,#3067,#3068,#3069,#3070,
#3071,#3072,#3073,#3074,#3075,#3076,#3077,#3078,#3079,#3080,#3081,#3082,
#3083,#3084,#3085,#3086,#3087,#3088,#3089,#3090,#3091,#3092,#3093,#3094,
#3095,#3096,#3097,#3098,#3099,#3100,#3101,#3102,#3103,#3104,#3105,#3106,
#3107,#3108,#3109,#3110,#3111,#3112,#3113,#3114,#3115,#3116,#3117,#3118,
#3119,#3120,#3121));
#950=EDGE_LOOP('',(#3122,#3123,#3124,#3125,#3126));
#951=EDGE_LOOP('',(#3127,#3128,#3129,#3130,#3131,#3132,#3133,#3134,#3135,
#3136,#3137,#3138,#3139,#3140,#3141,#3142,#3143,#3144,#3145,#3146,#3147,
#3148,#3149,#3150,#3151,#3152,#3153,#3154,#3155,#3156,#3157,#3158,#3159,
#3160,#3161,#3162,#3163,#3164,#3165,#3166,#3167,#3168,#3169,#3170,#3171,
#3172,#3173,#3174,#3175,#3176,#3177,#3178,#3179,#3180,#3181,#3182,#3183,
#3184,#3185,#3186,#3187,#3188,#3189,#3190,#3191,#3192,#3193,#3194,#3195,
#3196,#3197,#3198,#3199,#3200,#3201,#3202));
#952=EDGE_LOOP('',(#3203,#3204,#3205,#3206,#3207,#3208,#3209,#3210,#3211,
#3212,#3213,#3214,#3215,#3216,#3217,#3218,#3219,#3220,#3221,#3222,#3223,
#3224,#3225,#3226,#3227,#3228,#3229,#3230,#3231,#3232,#3233,#3234,#3235,
#3236,#3237,#3238,#3239,#3240,#3241,#3242,#3243,#3244,#3245,#3246,#3247,
#3248,#3249,#3250,#3251,#3252,#3253,#3254,#3255,#3256,#3257,#3258,#3259,
#3260,#3261,#3262,#3263,#3264,#3265,#3266,#3267,#3268,#3269,#3270,#3271,
#3272,#3273,#3274,#3275,#3276,#3277,#3278));
#953=EDGE_LOOP('',(#3279,#3280,#3281,#3282,#3283));
#954=EDGE_LOOP('',(#3284,#3285,#3286,#3287));
#955=EDGE_LOOP('',(#3288));
#956=EDGE_LOOP('',(#3289));
#957=EDGE_LOOP('',(#3290,#3291,#3292,#3293));
#958=EDGE_LOOP('',(#3294,#3295,#3296,#3297,#3298,#3299));
#959=EDGE_LOOP('',(#3300));
#960=EDGE_LOOP('',(#3301,#3302,#3303,#3304));
#961=EDGE_LOOP('',(#3305,#3306,#3307,#3308));
#962=EDGE_LOOP('',(#3309,#3310,#3311,#3312));
#963=EDGE_LOOP('',(#3313,#3314,#3315,#3316));
#964=EDGE_LOOP('',(#3317,#3318,#3319,#3320));
#965=EDGE_LOOP('',(#3321,#3322,#3323,#3324));
#966=EDGE_LOOP('',(#3325,#3326,#3327,#3328,#3329,#3330));
#967=EDGE_LOOP('',(#3331));
#968=EDGE_LOOP('',(#3332,#3333,#3334,#3335));
#969=EDGE_LOOP('',(#3336,#3337,#3338,#3339));
#970=EDGE_LOOP('',(#3340,#3341,#3342,#3343,#3344));
#971=EDGE_LOOP('',(#3345,#3346,#3347,#3348,#3349));
#972=EDGE_LOOP('',(#3350,#3351,#3352));
#973=EDGE_LOOP('',(#3353,#3354,#3355,#3356,#3357,#3358,#3359,#3360,#3361,
#3362));
#974=EDGE_LOOP('',(#3363,#3364,#3365,#3366,#3367,#3368));
#975=EDGE_LOOP('',(#3369,#3370,#3371,#3372));
#976=EDGE_LOOP('',(#3373,#3374,#3375,#3376,#3377,#3378,#3379,#3380,#3381,
#3382));
#977=EDGE_LOOP('',(#3383,#3384,#3385,#3386));
#978=EDGE_LOOP('',(#3387,#3388,#3389,#3390));
#979=EDGE_LOOP('',(#3391,#3392,#3393,#3394));
#980=EDGE_LOOP('',(#3395,#3396,#3397,#3398));
#981=EDGE_LOOP('',(#3399,#3400,#3401,#3402));
#982=EDGE_LOOP('',(#3403,#3404,#3405,#3406));
#983=EDGE_LOOP('',(#3407,#3408,#3409,#3410));
#984=EDGE_LOOP('',(#3411,#3412,#3413,#3414));
#985=EDGE_LOOP('',(#3415,#3416,#3417,#3418));
#986=EDGE_LOOP('',(#3419,#3420,#3421,#3422));
#987=EDGE_LOOP('',(#3423,#3424,#3425,#3426));
#988=EDGE_LOOP('',(#3427,#3428,#3429,#3430));
#989=EDGE_LOOP('',(#3431,#3432,#3433,#3434));
#990=EDGE_LOOP('',(#3435,#3436,#3437,#3438));
#991=EDGE_LOOP('',(#3439,#3440,#3441,#3442));
#992=EDGE_LOOP('',(#3443,#3444,#3445,#3446));
#993=EDGE_LOOP('',(#3447,#3448,#3449,#3450));
#994=EDGE_LOOP('',(#3451,#3452,#3453,#3454,#3455,#3456,#3457,#3458,#3459,
#3460,#3461,#3462));
#995=EDGE_LOOP('',(#3463,#3464,#3465,#3466));
#996=EDGE_LOOP('',(#3467,#3468,#3469,#3470));
#997=EDGE_LOOP('',(#3471,#3472,#3473,#3474));
#998=EDGE_LOOP('',(#3475,#3476,#3477,#3478));
#999=EDGE_LOOP('',(#3479,#3480,#3481,#3482));
#1000=EDGE_LOOP('',(#3483,#3484,#3485,#3486));
#1001=EDGE_LOOP('',(#3487,#3488,#3489,#3490));
#1002=EDGE_LOOP('',(#3491,#3492,#3493,#3494));
#1003=EDGE_LOOP('',(#3495,#3496,#3497,#3498));
#1004=EDGE_LOOP('',(#3499,#3500,#3501,#3502));
#1005=EDGE_LOOP('',(#3503,#3504,#3505,#3506));
#1006=EDGE_LOOP('',(#3507,#3508,#3509,#3510));
#1007=EDGE_LOOP('',(#3511,#3512,#3513,#3514));
#1008=EDGE_LOOP('',(#3515,#3516,#3517,#3518));
#1009=EDGE_LOOP('',(#3519,#3520,#3521,#3522));
#1010=EDGE_LOOP('',(#3523,#3524,#3525,#3526));
#1011=EDGE_LOOP('',(#3527,#3528,#3529,#3530));
#1012=EDGE_LOOP('',(#3531,#3532,#3533,#3534));
#1013=EDGE_LOOP('',(#3535,#3536,#3537,#3538));
#1014=EDGE_LOOP('',(#3539,#3540,#3541,#3542));
#1015=EDGE_LOOP('',(#3543,#3544,#3545,#3546));
#1016=EDGE_LOOP('',(#3547,#3548,#3549,#3550));
#1017=EDGE_LOOP('',(#3551,#3552,#3553,#3554,#3555,#3556,#3557,#3558,#3559,
#3560,#3561,#3562));
#1018=EDGE_LOOP('',(#3563,#3564,#3565,#3566));
#1019=EDGE_LOOP('',(#3567,#3568,#3569,#3570,#3571,#3572));
#1020=EDGE_LOOP('',(#3573,#3574,#3575,#3576,#3577));
#1021=EDGE_LOOP('',(#3578,#3579,#3580,#3581,#3582,#3583));
#1022=EDGE_LOOP('',(#3584,#3585,#3586,#3587));
#1023=EDGE_LOOP('',(#3588,#3589,#3590,#3591));
#1024=EDGE_LOOP('',(#3592,#3593,#3594,#3595,#3596,#3597));
#1025=EDGE_LOOP('',(#3598,#3599,#3600,#3601,#3602,#3603));
#1026=EDGE_LOOP('',(#3604,#3605,#3606,#3607,#3608,#3609));
#1027=EDGE_LOOP('',(#3610,#3611,#3612,#3613,#3614,#3615));
#1028=EDGE_LOOP('',(#3616,#3617,#3618,#3619,#3620,#3621));
#1029=EDGE_LOOP('',(#3622,#3623,#3624,#3625,#3626,#3627));
#1030=EDGE_LOOP('',(#3628,#3629,#3630,#3631));
#1031=EDGE_LOOP('',(#3632,#3633,#3634,#3635,#3636));
#1032=EDGE_LOOP('',(#3637,#3638,#3639,#3640,#3641));
#1033=EDGE_LOOP('',(#3642,#3643,#3644,#3645));
#1034=EDGE_LOOP('',(#3646,#3647,#3648,#3649,#3650));
#1035=EDGE_LOOP('',(#3651,#3652,#3653,#3654));
#1036=EDGE_LOOP('',(#3655,#3656,#3657,#3658));
#1037=EDGE_LOOP('',(#3659,#3660,#3661,#3662,#3663));
#1038=EDGE_LOOP('',(#3664,#3665,#3666,#3667,#3668,#3669));
#1039=EDGE_LOOP('',(#3670,#3671,#3672,#3673,#3674,#3675,#3676,#3677,#3678,
#3679,#3680,#3681,#3682,#3683,#3684,#3685,#3686,#3687,#3688,#3689,#3690,
#3691,#3692,#3693,#3694,#3695));
#1040=EDGE_LOOP('',(#3696,#3697,#3698,#3699,#3700,#3701,#3702,#3703,#3704,
#3705,#3706,#3707,#3708,#3709,#3710,#3711,#3712,#3713,#3714,#3715,#3716,
#3717,#3718,#3719,#3720,#3721,#3722,#3723,#3724));
#1041=EDGE_LOOP('',(#3725,#3726,#3727,#3728,#3729,#3730));
#1042=EDGE_LOOP('',(#3731,#3732,#3733,#3734,#3735));
#1043=EDGE_LOOP('',(#3736,#3737,#3738,#3739));
#1044=EDGE_LOOP('',(#3740,#3741,#3742,#3743));
#1045=EDGE_LOOP('',(#3744,#3745,#3746,#3747));
#1046=EDGE_LOOP('',(#3748,#3749,#3750,#3751));
#1047=EDGE_LOOP('',(#3752,#3753,#3754,#3755));
#1048=EDGE_LOOP('',(#3756,#3757,#3758,#3759));
#1049=EDGE_LOOP('',(#3760,#3761,#3762,#3763,#3764,#3765));
#1050=EDGE_LOOP('',(#3766,#3767,#3768,#3769));
#1051=LINE('',#5340,#1264);
#1052=LINE('',#5342,#1265);
#1053=LINE('',#5344,#1266);
#1054=LINE('',#5346,#1267);
#1055=LINE('',#5347,#1268);
#1056=LINE('',#5350,#1269);
#1057=LINE('',#5352,#1270);
#1058=LINE('',#5354,#1271);
#1059=LINE('',#5355,#1272);
#1060=LINE('',#5358,#1273);
#1061=LINE('',#5360,#1274);
#1062=LINE('',#5362,#1275);
#1063=LINE('',#5363,#1276);
#1064=LINE('',#5366,#1277);
#1065=LINE('',#5368,#1278);
#1066=LINE('',#5370,#1279);
#1067=LINE('',#5371,#1280);
#1068=LINE('',#5377,#1281);
#1069=LINE('',#5378,#1282);
#1070=LINE('',#5381,#1283);
#1071=LINE('',#5391,#1284);
#1072=LINE('',#5395,#1285);
#1073=LINE('',#5396,#1286);
#1074=LINE('',#5398,#1287);
#1075=LINE('',#5407,#1288);
#1076=LINE('',#5425,#1289);
#1077=LINE('',#5796,#1290);
#1078=LINE('',#5837,#1291);
#1079=LINE('',#5842,#1292);
#1080=LINE('',#5851,#1293);
#1081=LINE('',#5857,#1294);
#1082=LINE('',#5866,#1295);
#1083=LINE('',#5869,#1296);
#1084=LINE('',#5880,#1297);
#1085=LINE('',#5881,#1298);
#1086=LINE('',#5884,#1299);
#1087=LINE('',#5886,#1300);
#1088=LINE('',#5887,#1301);
#1089=LINE('',#5890,#1302);
#1090=LINE('',#5894,#1303);
#1091=LINE('',#5895,#1304);
#1092=LINE('',#5900,#1305);
#1093=LINE('',#5909,#1306);
#1094=LINE('',#5911,#1307);
#1095=LINE('',#5913,#1308);
#1096=LINE('',#5916,#1309);
#1097=LINE('',#5918,#1310);
#1098=LINE('',#5920,#1311);
#1099=LINE('',#5921,#1312);
#1100=LINE('',#5927,#1313);
#1101=LINE('',#5930,#1314);
#1102=LINE('',#5932,#1315);
#1103=LINE('',#5933,#1316);
#1104=LINE('',#5938,#1317);
#1105=LINE('',#5941,#1318);
#1106=LINE('',#5943,#1319);
#1107=LINE('',#5955,#1320);
#1108=LINE('',#5968,#1321);
#1109=LINE('',#6267,#1322);
#1110=LINE('',#6749,#1323);
#1111=LINE('',#7299,#1324);
#1112=LINE('',#7666,#1325);
#1113=LINE('',#8148,#1326);
#1114=LINE('',#8698,#1327);
#1115=LINE('',#9018,#1328);
#1116=LINE('',#9149,#1329);
#1117=LINE('',#9351,#1330);
#1118=LINE('',#9548,#1331);
#1119=LINE('',#9754,#1332);
#1120=LINE('',#11640,#1333);
#1121=LINE('',#11642,#1334);
#1122=LINE('',#11644,#1335);
#1123=LINE('',#11646,#1336);
#1124=LINE('',#11648,#1337);
#1125=LINE('',#11649,#1338);
#1126=LINE('',#11653,#1339);
#1127=LINE('',#11654,#1340);
#1128=LINE('',#11655,#1341);
#1129=LINE('',#11658,#1342);
#1130=LINE('',#11659,#1343);
#1131=LINE('',#11662,#1344);
#1132=LINE('',#11663,#1345);
#1133=LINE('',#11666,#1346);
#1134=LINE('',#11667,#1347);
#1135=LINE('',#11670,#1348);
#1136=LINE('',#11671,#1349);
#1137=LINE('',#11673,#1350);
#1138=LINE('',#11679,#1351);
#1139=LINE('',#11868,#1352);
#1140=LINE('',#12373,#1353);
#1141=LINE('',#12815,#1354);
#1142=LINE('',#13203,#1355);
#1143=LINE('',#13596,#1356);
#1144=LINE('',#14073,#1357);
#1145=LINE('',#14568,#1358);
#1146=LINE('',#15045,#1359);
#1147=LINE('',#15534,#1360);
#1148=LINE('',#15991,#1361);
#1149=LINE('',#16532,#1362);
#1150=LINE('',#16849,#1363);
#1151=LINE('',#17277,#1364);
#1152=LINE('',#17731,#1365);
#1153=LINE('',#18219,#1366);
#1154=LINE('',#18663,#1367);
#1155=LINE('',#19059,#1368);
#1156=LINE('',#19484,#1369);
#1157=LINE('',#19945,#1370);
#1158=LINE('',#20394,#1371);
#1159=LINE('',#20863,#1372);
#1160=LINE('',#21308,#1373);
#1161=LINE('',#21809,#1374);
#1162=LINE('',#22268,#1375);
#1163=LINE('',#22570,#1376);
#1164=LINE('',#22986,#1377);
#1165=LINE('',#23424,#1378);
#1166=LINE('',#33580,#1379);
#1167=LINE('',#33585,#1380);
#1168=LINE('',#33587,#1381);
#1169=LINE('',#33589,#1382);
#1170=LINE('',#33591,#1383);
#1171=LINE('',#33593,#1384);
#1172=LINE('',#33594,#1385);
#1173=LINE('',#33597,#1386);
#1174=LINE('',#33599,#1387);
#1175=LINE('',#33600,#1388);
#1176=LINE('',#33603,#1389);
#1177=LINE('',#33604,#1390);
#1178=LINE('',#33607,#1391);
#1179=LINE('',#33608,#1392);
#1180=LINE('',#33611,#1393);
#1181=LINE('',#33612,#1394);
#1182=LINE('',#33615,#1395);
#1183=LINE('',#33616,#1396);
#1184=LINE('',#33618,#1397);
#1185=LINE('',#33624,#1398);
#1186=LINE('',#33879,#1399);
#1187=LINE('',#34272,#1400);
#1188=LINE('',#34413,#1401);
#1189=LINE('',#34715,#1402);
#1190=LINE('',#36732,#1403);
#1191=LINE('',#36733,#1404);
#1192=LINE('',#36744,#1405);
#1193=LINE('',#36745,#1406);
#1194=LINE('',#36756,#1407);
#1195=LINE('',#36757,#1408);
#1196=LINE('',#36768,#1409);
#1197=LINE('',#36769,#1410);
#1198=LINE('',#36780,#1411);
#1199=LINE('',#36781,#1412);
#1200=LINE('',#36792,#1413);
#1201=LINE('',#36793,#1414);
#1202=LINE('',#36801,#1415);
#1203=LINE('',#36802,#1416);
#1204=LINE('',#36805,#1417);
#1205=LINE('',#36808,#1418);
#1206=LINE('',#36811,#1419);
#1207=LINE('',#36812,#1420);
#1208=LINE('',#36815,#1421);
#1209=LINE('',#36819,#1422);
#1210=LINE('',#36821,#1423);
#1211=LINE('',#36825,#1424);
#1212=LINE('',#36828,#1425);
#1213=LINE('',#36830,#1426);
#1214=LINE('',#36832,#1427);
#1215=LINE('',#36833,#1428);
#1216=LINE('',#36835,#1429);
#1217=LINE('',#36850,#1430);
#1218=LINE('',#36851,#1431);
#1219=LINE('',#36861,#1432);
#1220=LINE('',#36862,#1433);
#1221=LINE('',#36870,#1434);
#1222=LINE('',#36878,#1435);
#1223=LINE('',#36886,#1436);
#1224=LINE('',#36894,#1437);
#1225=LINE('',#36902,#1438);
#1226=LINE('',#36903,#1439);
#1227=LINE('',#36905,#1440);
#1228=LINE('',#36907,#1441);
#1229=LINE('',#36908,#1442);
#1230=LINE('',#36910,#1443);
#1231=LINE('',#36913,#1444);
#1232=LINE('',#36921,#1445);
#1233=LINE('',#36937,#1446);
#1234=LINE('',#37306,#1447);
#1235=LINE('',#37853,#1448);
#1236=LINE('',#38241,#1449);
#1237=LINE('',#38702,#1450);
#1238=LINE('',#39252,#1451);
#1239=LINE('',#39455,#1452);
#1240=LINE('',#39584,#1453);
#1241=LINE('',#39843,#1454);
#1242=LINE('',#39999,#1455);
#1243=LINE('',#40203,#1456);
#1244=LINE('',#40402,#1457);
#1245=LINE('',#40598,#1458);
#1246=LINE('',#42602,#1459);
#1247=LINE('',#42604,#1460);
#1248=LINE('',#42606,#1461);
#1249=LINE('',#42608,#1462);
#1250=LINE('',#42610,#1463);
#1251=LINE('',#42611,#1464);
#1252=LINE('',#42615,#1465);
#1253=LINE('',#42616,#1466);
#1254=LINE('',#42617,#1467);
#1255=LINE('',#42620,#1468);
#1256=LINE('',#42621,#1469);
#1257=LINE('',#42624,#1470);
#1258=LINE('',#42625,#1471);
#1259=LINE('',#42628,#1472);
#1260=LINE('',#42629,#1473);
#1261=LINE('',#42632,#1474);
#1262=LINE('',#42633,#1475);
#1263=LINE('',#42635,#1476);
#1264=VECTOR('',#4474,10.);
#1265=VECTOR('',#4475,10.);
#1266=VECTOR('',#4476,10.);
#1267=VECTOR('',#4477,10.);
#1268=VECTOR('',#4478,10.);
#1269=VECTOR('',#4481,10.);
#1270=VECTOR('',#4482,10.);
#1271=VECTOR('',#4483,10.);
#1272=VECTOR('',#4484,10.);
#1273=VECTOR('',#4487,10.);
#1274=VECTOR('',#4488,10.);
#1275=VECTOR('',#4489,10.);
#1276=VECTOR('',#4490,10.);
#1277=VECTOR('',#4493,9.99999999999999);
#1278=VECTOR('',#4494,10.);
#1279=VECTOR('',#4495,9.99999999999999);
#1280=VECTOR('',#4496,9.99999999999999);
#1281=VECTOR('',#4501,10.);
#1282=VECTOR('',#4502,10.);
#1283=VECTOR('',#4507,10.);
#1284=VECTOR('',#4524,10.);
#1285=VECTOR('',#4529,10.);
#1286=VECTOR('',#4530,10.);
#1287=VECTOR('',#4533,10.);
#1288=VECTOR('',#4544,9.);
#1289=VECTOR('',#4569,7.5);
#1290=VECTOR('',#4574,19.);
#1291=VECTOR('',#4579,6.);
#1292=VECTOR('',#4584,15.);
#1293=VECTOR('',#4595,15.);
#1294=VECTOR('',#4604,12.);
#1295=VECTOR('',#4615,10.);
#1296=VECTOR('',#4618,10.);
#1297=VECTOR('',#4631,10.);
#1298=VECTOR('',#4632,10.);
#1299=VECTOR('',#4635,10.);
#1300=VECTOR('',#4636,10.);
#1301=VECTOR('',#4637,10.);
#1302=VECTOR('',#4640,10.);
#1303=VECTOR('',#4645,10.);
#1304=VECTOR('',#4646,10.);
#1305=VECTOR('',#4651,10.);
#1306=VECTOR('',#4664,10.);
#1307=VECTOR('',#4667,10.);
#1308=VECTOR('',#4670,10.);
#1309=VECTOR('',#4671,10.);
#1310=VECTOR('',#4672,10.);
#1311=VECTOR('',#4673,10.);
#1312=VECTOR('',#4674,10.);
#1313=VECTOR('',#4679,10.);
#1314=VECTOR('',#4682,30.);
#1315=VECTOR('',#4685,10.);
#1316=VECTOR('',#4686,10.);
#1317=VECTOR('',#4691,30.);
#1318=VECTOR('',#4696,10.);
#1319=VECTOR('',#4699,10.);
#1320=VECTOR('',#4716,12.1745);
#1321=VECTOR('',#4721,12.1745);
#1322=VECTOR('',#4726,12.1745);
#1323=VECTOR('',#4729,12.1745);
#1324=VECTOR('',#4732,12.1745);
#1325=VECTOR('',#4735,12.1745);
#1326=VECTOR('',#4738,12.1745);
#1327=VECTOR('',#4741,10.501);
#1328=VECTOR('',#4746,10.501);
#1329=VECTOR('',#4749,10.501);
#1330=VECTOR('',#4752,10.501);
#1331=VECTOR('',#4755,10.501);
#1332=VECTOR('',#4758,10.501);
#1333=VECTOR('',#4769,10.);
#1334=VECTOR('',#4770,10.);
#1335=VECTOR('',#4771,10.);
#1336=VECTOR('',#4772,10.);
#1337=VECTOR('',#4773,10.);
#1338=VECTOR('',#4774,10.);
#1339=VECTOR('',#4777,10.);
#1340=VECTOR('',#4778,10.);
#1341=VECTOR('',#4779,10.);
#1342=VECTOR('',#4782,10.);
#1343=VECTOR('',#4783,10.);
#1344=VECTOR('',#4786,10.);
#1345=VECTOR('',#4787,10.);
#1346=VECTOR('',#4790,10.);
#1347=VECTOR('',#4791,10.);
#1348=VECTOR('',#4794,10.);
#1349=VECTOR('',#4795,10.);
#1350=VECTOR('',#4798,10.);
#1351=VECTOR('',#4805,3.22275);
#1352=VECTOR('',#4810,3.22275);
#1353=VECTOR('',#4813,3.22275);
#1354=VECTOR('',#4816,3.22275);
#1355=VECTOR('',#4819,3.22275);
#1356=VECTOR('',#4822,3.22275);
#1357=VECTOR('',#4825,3.22275);
#1358=VECTOR('',#4828,3.22275);
#1359=VECTOR('',#4831,3.22275);
#1360=VECTOR('',#4834,3.22275);
#1361=VECTOR('',#4837,3.22275);
#1362=VECTOR('',#4840,3.22275);
#1363=VECTOR('',#4843,3.22275);
#1364=VECTOR('',#4846,3.22275);
#1365=VECTOR('',#4849,3.22275);
#1366=VECTOR('',#4852,3.22275);
#1367=VECTOR('',#4855,3.22275);
#1368=VECTOR('',#4858,3.22275);
#1369=VECTOR('',#4861,3.22275);
#1370=VECTOR('',#4864,3.22275);
#1371=VECTOR('',#4867,3.22275);
#1372=VECTOR('',#4870,3.22275);
#1373=VECTOR('',#4873,3.22275);
#1374=VECTOR('',#4876,3.22275);
#1375=VECTOR('',#4879,3.22275);
#1376=VECTOR('',#4882,3.22275);
#1377=VECTOR('',#4885,3.22275);
#1378=VECTOR('',#4888,3.22275);
#1379=VECTOR('',#4917,4.);
#1380=VECTOR('',#4922,10.);
#1381=VECTOR('',#4923,10.);
#1382=VECTOR('',#4924,10.);
#1383=VECTOR('',#4925,10.);
#1384=VECTOR('',#4926,9.99999999999999);
#1385=VECTOR('',#4927,10.);
#1386=VECTOR('',#4930,10.);
#1387=VECTOR('',#4931,10.);
#1388=VECTOR('',#4932,10.);
#1389=VECTOR('',#4935,10.);
#1390=VECTOR('',#4936,10.);
#1391=VECTOR('',#4939,10.);
#1392=VECTOR('',#4940,10.);
#1393=VECTOR('',#4943,9.99999999999999);
#1394=VECTOR('',#4944,10.);
#1395=VECTOR('',#4947,10.);
#1396=VECTOR('',#4948,10.);
#1397=VECTOR('',#4951,10.);
#1398=VECTOR('',#4958,3.933);
#1399=VECTOR('',#4963,3.933);
#1400=VECTOR('',#4968,3.22275);
#1401=VECTOR('',#4973,3.22275);
#1402=VECTOR('',#4976,3.22275);
#1403=VECTOR('',#4999,10.);
#1404=VECTOR('',#5000,10.);
#1405=VECTOR('',#5013,10.);
#1406=VECTOR('',#5014,10.);
#1407=VECTOR('',#5027,10.);
#1408=VECTOR('',#5028,10.);
#1409=VECTOR('',#5041,10.);
#1410=VECTOR('',#5042,10.);
#1411=VECTOR('',#5055,10.);
#1412=VECTOR('',#5056,10.);
#1413=VECTOR('',#5069,10.);
#1414=VECTOR('',#5070,10.);
#1415=VECTOR('',#5081,10.);
#1416=VECTOR('',#5082,10.);
#1417=VECTOR('',#5085,10.);
#1418=VECTOR('',#5088,10.);
#1419=VECTOR('',#5091,10.);
#1420=VECTOR('',#5092,10.);
#1421=VECTOR('',#5095,10.);
#1422=VECTOR('',#5100,10.);
#1423=VECTOR('',#5101,10.);
#1424=VECTOR('',#5104,10.);
#1425=VECTOR('',#5107,10.);
#1426=VECTOR('',#5110,10.);
#1427=VECTOR('',#5113,10.);
#1428=VECTOR('',#5114,10.);
#1429=VECTOR('',#5117,10.);
#1430=VECTOR('',#5134,10.);
#1431=VECTOR('',#5135,10.);
#1432=VECTOR('',#5148,10.);
#1433=VECTOR('',#5149,10.);
#1434=VECTOR('',#5160,10.);
#1435=VECTOR('',#5171,10.);
#1436=VECTOR('',#5182,10.);
#1437=VECTOR('',#5193,10.);
#1438=VECTOR('',#5204,10.);
#1439=VECTOR('',#5205,10.);
#1440=VECTOR('',#5208,10.);
#1441=VECTOR('',#5211,10.);
#1442=VECTOR('',#5212,10.);
#1443=VECTOR('',#5215,10.);
#1444=VECTOR('',#5220,10.);
#1445=VECTOR('',#5231,12.1745);
#1446=VECTOR('',#5236,12.1745);
#1447=VECTOR('',#5239,12.1745);
#1448=VECTOR('',#5242,12.1745);
#1449=VECTOR('',#5245,12.1745);
#1450=VECTOR('',#5248,12.1745);
#1451=VECTOR('',#5251,12.1745);
#1452=VECTOR('',#5256,10.501);
#1453=VECTOR('',#5261,10.501);
#1454=VECTOR('',#5264,10.501);
#1455=VECTOR('',#5267,10.501);
#1456=VECTOR('',#5270,10.501);
#1457=VECTOR('',#5273,10.501);
#1458=VECTOR('',#5276,10.501);
#1459=VECTOR('',#5285,10.);
#1460=VECTOR('',#5286,10.);
#1461=VECTOR('',#5287,10.);
#1462=VECTOR('',#5288,10.);
#1463=VECTOR('',#5289,10.);
#1464=VECTOR('',#5290,10.);
#1465=VECTOR('',#5293,10.);
#1466=VECTOR('',#5294,10.);
#1467=VECTOR('',#5295,10.);
#1468=VECTOR('',#5298,10.);
#1469=VECTOR('',#5299,10.);
#1470=VECTOR('',#5302,10.);
#1471=VECTOR('',#5303,10.);
#1472=VECTOR('',#5306,10.);
#1473=VECTOR('',#5307,10.);
#1474=VECTOR('',#5310,10.);
#1475=VECTOR('',#5311,10.);
#1476=VECTOR('',#5314,10.);
#1477=VERTEX_POINT('',#5338);
#1478=VERTEX_POINT('',#5339);
#1479=VERTEX_POINT('',#5341);
#1480=VERTEX_POINT('',#5343);
#1481=VERTEX_POINT('',#5345);
#1482=VERTEX_POINT('',#5349);
#1483=VERTEX_POINT('',#5351);
#1484=VERTEX_POINT('',#5353);
#1485=VERTEX_POINT('',#5357);
#1486=VERTEX_POINT('',#5359);
#1487=VERTEX_POINT('',#5361);
#1488=VERTEX_POINT('',#5365);
#1489=VERTEX_POINT('',#5367);
#1490=VERTEX_POINT('',#5369);
#1491=VERTEX_POINT('',#5373);
#1492=VERTEX_POINT('',#5374);
#1493=VERTEX_POINT('',#5376);
#1494=VERTEX_POINT('',#5389);
#1495=VERTEX_POINT('',#5394);
#1496=VERTEX_POINT('',#5400);
#1497=VERTEX_POINT('',#5402);
#1498=VERTEX_POINT('',#5406);
#1499=VERTEX_POINT('',#5411);
#1500=VERTEX_POINT('',#5415);
#1501=VERTEX_POINT('',#5418);
#1502=VERTEX_POINT('',#5419);
#1503=VERTEX_POINT('',#5424);
#1504=VERTEX_POINT('',#5426);
#1505=VERTEX_POINT('',#5768);
#1506=VERTEX_POINT('',#5793);
#1507=VERTEX_POINT('',#5795);
#1508=VERTEX_POINT('',#5799);
#1509=VERTEX_POINT('',#5800);
#1510=VERTEX_POINT('',#5839);
#1511=VERTEX_POINT('',#5841);
#1512=VERTEX_POINT('',#5845);
#1513=VERTEX_POINT('',#5848);
#1514=VERTEX_POINT('',#5850);
#1515=VERTEX_POINT('',#5854);
#1516=VERTEX_POINT('',#5862);
#1517=VERTEX_POINT('',#5863);
#1518=VERTEX_POINT('',#5865);
#1519=VERTEX_POINT('',#5867);
#1520=VERTEX_POINT('',#5871);
#1521=VERTEX_POINT('',#5872);
#1522=VERTEX_POINT('',#5877);
#1523=VERTEX_POINT('',#5878);
#1524=VERTEX_POINT('',#5883);
#1525=VERTEX_POINT('',#5885);
#1526=VERTEX_POINT('',#5889);
#1527=VERTEX_POINT('',#5893);
#1528=VERTEX_POINT('',#5897);
#1529=VERTEX_POINT('',#5899);
#1530=VERTEX_POINT('',#5903);
#1531=VERTEX_POINT('',#5907);
#1532=VERTEX_POINT('',#5914);
#1533=VERTEX_POINT('',#5915);
#1534=VERTEX_POINT('',#5917);
#1535=VERTEX_POINT('',#5919);
#1536=VERTEX_POINT('',#5923);
#1537=VERTEX_POINT('',#5924);
#1538=VERTEX_POINT('',#5926);
#1539=VERTEX_POINT('',#5928);
#1540=VERTEX_POINT('',#5935);
#1541=VERTEX_POINT('',#5937);
#1542=VERTEX_POINT('',#5948);
#1543=VERTEX_POINT('',#5953);
#1544=VERTEX_POINT('',#5954);
#1545=VERTEX_POINT('',#5956);
#1546=VERTEX_POINT('',#5966);
#1547=VERTEX_POINT('',#5967);
#1548=VERTEX_POINT('',#5969);
#1549=VERTEX_POINT('',#6242);
#1550=VERTEX_POINT('',#6244);
#1551=VERTEX_POINT('',#6265);
#1552=VERTEX_POINT('',#6266);
#1553=VERTEX_POINT('',#6268);
#1554=VERTEX_POINT('',#6541);
#1555=VERTEX_POINT('',#6747);
#1556=VERTEX_POINT('',#6748);
#1557=VERTEX_POINT('',#6750);
#1558=VERTEX_POINT('',#7023);
#1559=VERTEX_POINT('',#7297);
#1560=VERTEX_POINT('',#7298);
#1561=VERTEX_POINT('',#7300);
#1562=VERTEX_POINT('',#7390);
#1563=VERTEX_POINT('',#7664);
#1564=VERTEX_POINT('',#7665);
#1565=VERTEX_POINT('',#7667);
#1566=VERTEX_POINT('',#7872);
#1567=VERTEX_POINT('',#8146);
#1568=VERTEX_POINT('',#8147);
#1569=VERTEX_POINT('',#8149);
#1570=VERTEX_POINT('',#8425);
#1571=VERTEX_POINT('',#8696);
#1572=VERTEX_POINT('',#8697);
#1573=VERTEX_POINT('',#8699);
#1574=VERTEX_POINT('',#8704);
#1575=VERTEX_POINT('',#8943);
#1576=VERTEX_POINT('',#9016);
#1577=VERTEX_POINT('',#9017);
#1578=VERTEX_POINT('',#9019);
#1579=VERTEX_POINT('',#9147);
#1580=VERTEX_POINT('',#9148);
#1581=VERTEX_POINT('',#9349);
#1582=VERTEX_POINT('',#9350);
#1583=VERTEX_POINT('',#9352);
#1584=VERTEX_POINT('',#9546);
#1585=VERTEX_POINT('',#9547);
#1586=VERTEX_POINT('',#9752);
#1587=VERTEX_POINT('',#9753);
#1588=VERTEX_POINT('',#9755);
#1589=VERTEX_POINT('',#9965);
#1590=VERTEX_POINT('',#10062);
#1591=VERTEX_POINT('',#10258);
#1592=VERTEX_POINT('',#10335);
#1593=VERTEX_POINT('',#10345);
#1594=VERTEX_POINT('',#10347);
#1595=VERTEX_POINT('',#10793);
#1596=VERTEX_POINT('',#11638);
#1597=VERTEX_POINT('',#11639);
#1598=VERTEX_POINT('',#11641);
#1599=VERTEX_POINT('',#11643);
#1600=VERTEX_POINT('',#11645);
#1601=VERTEX_POINT('',#11647);
#1602=VERTEX_POINT('',#11651);
#1603=VERTEX_POINT('',#11652);
#1604=VERTEX_POINT('',#11657);
#1605=VERTEX_POINT('',#11661);
#1606=VERTEX_POINT('',#11665);
#1607=VERTEX_POINT('',#11669);
#1608=VERTEX_POINT('',#11677);
#1609=VERTEX_POINT('',#11678);
#1610=VERTEX_POINT('',#11680);
#1611=VERTEX_POINT('',#11793);
#1612=VERTEX_POINT('',#11866);
#1613=VERTEX_POINT('',#11867);
#1614=VERTEX_POINT('',#11869);
#1615=VERTEX_POINT('',#12141);
#1616=VERTEX_POINT('',#12371);
#1617=VERTEX_POINT('',#12372);
#1618=VERTEX_POINT('',#12813);
#1619=VERTEX_POINT('',#12814);
#1620=VERTEX_POINT('',#12816);
#1621=VERTEX_POINT('',#13069);
#1622=VERTEX_POINT('',#13201);
#1623=VERTEX_POINT('',#13202);
#1624=VERTEX_POINT('',#13424);
#1625=VERTEX_POINT('',#13594);
#1626=VERTEX_POINT('',#13595);
#1627=VERTEX_POINT('',#13597);
#1628=VERTEX_POINT('',#14071);
#1629=VERTEX_POINT('',#14072);
#1630=VERTEX_POINT('',#14302);
#1631=VERTEX_POINT('',#14566);
#1632=VERTEX_POINT('',#14567);
#1633=VERTEX_POINT('',#14569);
#1634=VERTEX_POINT('',#15043);
#1635=VERTEX_POINT('',#15044);
#1636=VERTEX_POINT('',#15278);
#1637=VERTEX_POINT('',#15532);
#1638=VERTEX_POINT('',#15533);
#1639=VERTEX_POINT('',#15535);
#1640=VERTEX_POINT('',#15989);
#1641=VERTEX_POINT('',#15990);
#1642=VERTEX_POINT('',#16220);
#1643=VERTEX_POINT('',#16530);
#1644=VERTEX_POINT('',#16531);
#1645=VERTEX_POINT('',#16533);
#1646=VERTEX_POINT('',#16847);
#1647=VERTEX_POINT('',#16848);
#1648=VERTEX_POINT('',#16850);
#1649=VERTEX_POINT('',#17047);
#1650=VERTEX_POINT('',#17275);
#1651=VERTEX_POINT('',#17276);
#1652=VERTEX_POINT('',#17729);
#1653=VERTEX_POINT('',#17730);
#1654=VERTEX_POINT('',#17732);
#1655=VERTEX_POINT('',#17985);
#1656=VERTEX_POINT('',#18217);
#1657=VERTEX_POINT('',#18218);
#1658=VERTEX_POINT('',#18661);
#1659=VERTEX_POINT('',#18662);
#1660=VERTEX_POINT('',#18664);
#1661=VERTEX_POINT('',#18973);
#1662=VERTEX_POINT('',#19057);
#1663=VERTEX_POINT('',#19058);
#1664=VERTEX_POINT('',#19284);
#1665=VERTEX_POINT('',#19482);
#1666=VERTEX_POINT('',#19483);
#1667=VERTEX_POINT('',#19485);
#1668=VERTEX_POINT('',#19943);
#1669=VERTEX_POINT('',#19944);
#1670=VERTEX_POINT('',#20168);
#1671=VERTEX_POINT('',#20392);
#1672=VERTEX_POINT('',#20393);
#1673=VERTEX_POINT('',#20395);
#1674=VERTEX_POINT('',#20861);
#1675=VERTEX_POINT('',#20862);
#1676=VERTEX_POINT('',#21074);
#1677=VERTEX_POINT('',#21306);
#1678=VERTEX_POINT('',#21307);
#1679=VERTEX_POINT('',#21309);
#1680=VERTEX_POINT('',#21807);
#1681=VERTEX_POINT('',#21808);
#1682=VERTEX_POINT('',#22024);
#1683=VERTEX_POINT('',#22266);
#1684=VERTEX_POINT('',#22267);
#1685=VERTEX_POINT('',#22269);
#1686=VERTEX_POINT('',#22568);
#1687=VERTEX_POINT('',#22569);
#1688=VERTEX_POINT('',#22571);
#1689=VERTEX_POINT('',#22726);
#1690=VERTEX_POINT('',#22984);
#1691=VERTEX_POINT('',#22985);
#1692=VERTEX_POINT('',#23422);
#1693=VERTEX_POINT('',#23423);
#1694=VERTEX_POINT('',#23425);
#1695=VERTEX_POINT('',#23650);
#1696=VERTEX_POINT('',#23920);
#1697=VERTEX_POINT('',#23921);
#1698=VERTEX_POINT('',#23995);
#1699=VERTEX_POINT('',#23997);
#1700=VERTEX_POINT('',#24003);
#1701=VERTEX_POINT('',#24230);
#1702=VERTEX_POINT('',#24241);
#1703=VERTEX_POINT('',#24465);
#1704=VERTEX_POINT('',#24695);
#1705=VERTEX_POINT('',#24706);
#1706=VERTEX_POINT('',#24717);
#1707=VERTEX_POINT('',#24944);
#1708=VERTEX_POINT('',#24955);
#1709=VERTEX_POINT('',#25182);
#1710=VERTEX_POINT('',#25409);
#1711=VERTEX_POINT('',#25421);
#1712=VERTEX_POINT('',#25648);
#1713=VERTEX_POINT('',#25875);
#1714=VERTEX_POINT('',#26102);
#1715=VERTEX_POINT('',#26113);
#1716=VERTEX_POINT('',#26343);
#1717=VERTEX_POINT('',#26570);
#1718=VERTEX_POINT('',#26582);
#1719=VERTEX_POINT('',#26593);
#1720=VERTEX_POINT('',#26604);
#1721=VERTEX_POINT('',#26616);
#1722=VERTEX_POINT('',#26843);
#1723=VERTEX_POINT('',#27070);
#1724=VERTEX_POINT('',#27081);
#1725=VERTEX_POINT('',#27308);
#1726=VERTEX_POINT('',#27319);
#1727=VERTEX_POINT('',#27546);
#1728=VERTEX_POINT('',#27731);
#1729=VERTEX_POINT('',#27733);
#1730=VERTEX_POINT('',#27742);
#1731=VERTEX_POINT('',#27969);
#1732=VERTEX_POINT('',#28196);
#1733=VERTEX_POINT('',#28423);
#1734=VERTEX_POINT('',#28434);
#1735=VERTEX_POINT('',#28661);
#1736=VERTEX_POINT('',#28672);
#1737=VERTEX_POINT('',#28684);
#1738=VERTEX_POINT('',#28911);
#1739=VERTEX_POINT('',#28922);
#1740=VERTEX_POINT('',#29149);
#1741=VERTEX_POINT('',#29160);
#1742=VERTEX_POINT('',#29387);
#1743=VERTEX_POINT('',#29614);
#1744=VERTEX_POINT('',#29626);
#1745=VERTEX_POINT('',#29853);
#1746=VERTEX_POINT('',#30080);
#1747=VERTEX_POINT('',#30092);
#1748=VERTEX_POINT('',#30319);
#1749=VERTEX_POINT('',#30330);
#1750=VERTEX_POINT('',#30341);
#1751=VERTEX_POINT('',#30568);
#1752=VERTEX_POINT('',#30795);
#1753=VERTEX_POINT('',#31022);
#1754=VERTEX_POINT('',#31034);
#1755=VERTEX_POINT('',#31261);
#1756=VERTEX_POINT('',#31499);
#1757=VERTEX_POINT('',#31644);
#1758=VERTEX_POINT('',#31646);
#1759=VERTEX_POINT('',#33381);
#1760=VERTEX_POINT('',#33572);
#1761=VERTEX_POINT('',#33577);
#1762=VERTEX_POINT('',#33579);
#1763=VERTEX_POINT('',#33583);
#1764=VERTEX_POINT('',#33584);
#1765=VERTEX_POINT('',#33586);
#1766=VERTEX_POINT('',#33588);
#1767=VERTEX_POINT('',#33590);
#1768=VERTEX_POINT('',#33592);
#1769=VERTEX_POINT('',#33596);
#1770=VERTEX_POINT('',#33598);
#1771=VERTEX_POINT('',#33602);
#1772=VERTEX_POINT('',#33606);
#1773=VERTEX_POINT('',#33610);
#1774=VERTEX_POINT('',#33614);
#1775=VERTEX_POINT('',#33622);
#1776=VERTEX_POINT('',#33623);
#1777=VERTEX_POINT('',#33625);
#1778=VERTEX_POINT('',#33732);
#1779=VERTEX_POINT('',#33877);
#1780=VERTEX_POINT('',#33878);
#1781=VERTEX_POINT('',#33880);
#1782=VERTEX_POINT('',#34056);
#1783=VERTEX_POINT('',#34270);
#1784=VERTEX_POINT('',#34271);
#1785=VERTEX_POINT('',#34273);
#1786=VERTEX_POINT('',#34279);
#1787=VERTEX_POINT('',#34281);
#1788=VERTEX_POINT('',#34411);
#1789=VERTEX_POINT('',#34412);
#1790=VERTEX_POINT('',#34414);
#1791=VERTEX_POINT('',#34713);
#1792=VERTEX_POINT('',#34714);
#1793=VERTEX_POINT('',#34716);
#1794=VERTEX_POINT('',#35731);
#1795=VERTEX_POINT('',#35896);
#1796=VERTEX_POINT('',#36720);
#1797=VERTEX_POINT('',#36721);
#1798=VERTEX_POINT('',#36723);
#1799=VERTEX_POINT('',#36725);
#1800=VERTEX_POINT('',#36729);
#1801=VERTEX_POINT('',#36730);
#1802=VERTEX_POINT('',#36735);
#1803=VERTEX_POINT('',#36736);
#1804=VERTEX_POINT('',#36741);
#1805=VERTEX_POINT('',#36742);
#1806=VERTEX_POINT('',#36747);
#1807=VERTEX_POINT('',#36748);
#1808=VERTEX_POINT('',#36753);
#1809=VERTEX_POINT('',#36754);
#1810=VERTEX_POINT('',#36759);
#1811=VERTEX_POINT('',#36760);
#1812=VERTEX_POINT('',#36765);
#1813=VERTEX_POINT('',#36766);
#1814=VERTEX_POINT('',#36771);
#1815=VERTEX_POINT('',#36772);
#1816=VERTEX_POINT('',#36777);
#1817=VERTEX_POINT('',#36778);
#1818=VERTEX_POINT('',#36783);
#1819=VERTEX_POINT('',#36784);
#1820=VERTEX_POINT('',#36789);
#1821=VERTEX_POINT('',#36790);
#1822=VERTEX_POINT('',#36795);
#1823=VERTEX_POINT('',#36796);
#1824=VERTEX_POINT('',#36804);
#1825=VERTEX_POINT('',#36806);
#1826=VERTEX_POINT('',#36810);
#1827=VERTEX_POINT('',#36814);
#1828=VERTEX_POINT('',#36818);
#1829=VERTEX_POINT('',#36820);
#1830=VERTEX_POINT('',#36822);
#1831=VERTEX_POINT('',#36824);
#1832=VERTEX_POINT('',#36826);
#1833=VERTEX_POINT('',#36838);
#1834=VERTEX_POINT('',#36839);
#1835=VERTEX_POINT('',#36841);
#1836=VERTEX_POINT('',#36843);
#1837=VERTEX_POINT('',#36847);
#1838=VERTEX_POINT('',#36848);
#1839=VERTEX_POINT('',#36853);
#1840=VERTEX_POINT('',#36854);
#1841=VERTEX_POINT('',#36859);
#1842=VERTEX_POINT('',#36864);
#1843=VERTEX_POINT('',#36868);
#1844=VERTEX_POINT('',#36872);
#1845=VERTEX_POINT('',#36876);
#1846=VERTEX_POINT('',#36880);
#1847=VERTEX_POINT('',#36884);
#1848=VERTEX_POINT('',#36888);
#1849=VERTEX_POINT('',#36892);
#1850=VERTEX_POINT('',#36896);
#1851=VERTEX_POINT('',#36897);
#1852=VERTEX_POINT('',#36919);
#1853=VERTEX_POINT('',#36920);
#1854=VERTEX_POINT('',#36922);
#1855=VERTEX_POINT('',#36927);
#1856=VERTEX_POINT('',#36935);
#1857=VERTEX_POINT('',#36936);
#1858=VERTEX_POINT('',#36938);
#1859=VERTEX_POINT('',#37119);
#1860=VERTEX_POINT('',#37304);
#1861=VERTEX_POINT('',#37305);
#1862=VERTEX_POINT('',#37307);
#1863=VERTEX_POINT('',#37580);
#1864=VERTEX_POINT('',#37851);
#1865=VERTEX_POINT('',#37852);
#1866=VERTEX_POINT('',#37854);
#1867=VERTEX_POINT('',#37965);
#1868=VERTEX_POINT('',#38239);
#1869=VERTEX_POINT('',#38240);
#1870=VERTEX_POINT('',#38242);
#1871=VERTEX_POINT('',#38426);
#1872=VERTEX_POINT('',#38700);
#1873=VERTEX_POINT('',#38701);
#1874=VERTEX_POINT('',#38703);
#1875=VERTEX_POINT('',#38976);
#1876=VERTEX_POINT('',#39250);
#1877=VERTEX_POINT('',#39251);
#1878=VERTEX_POINT('',#39253);
#1879=VERTEX_POINT('',#39263);
#1880=VERTEX_POINT('',#39270);
#1881=VERTEX_POINT('',#39272);
#1882=VERTEX_POINT('',#39453);
#1883=VERTEX_POINT('',#39454);
#1884=VERTEX_POINT('',#39456);
#1885=VERTEX_POINT('',#39527);
#1886=VERTEX_POINT('',#39582);
#1887=VERTEX_POINT('',#39583);
#1888=VERTEX_POINT('',#39585);
#1889=VERTEX_POINT('',#39841);
#1890=VERTEX_POINT('',#39842);
#1891=VERTEX_POINT('',#39844);
#1892=VERTEX_POINT('',#39997);
#1893=VERTEX_POINT('',#39998);
#1894=VERTEX_POINT('',#40201);
#1895=VERTEX_POINT('',#40202);
#1896=VERTEX_POINT('',#40204);
#1897=VERTEX_POINT('',#40400);
#1898=VERTEX_POINT('',#40401);
#1899=VERTEX_POINT('',#40596);
#1900=VERTEX_POINT('',#40597);
#1901=VERTEX_POINT('',#40599);
#1902=VERTEX_POINT('',#40614);
#1903=VERTEX_POINT('',#40729);
#1904=VERTEX_POINT('',#41008);
#1905=VERTEX_POINT('',#41281);
#1906=VERTEX_POINT('',#41755);
#1907=VERTEX_POINT('',#42600);
#1908=VERTEX_POINT('',#42601);
#1909=VERTEX_POINT('',#42603);
#1910=VERTEX_POINT('',#42605);
#1911=VERTEX_POINT('',#42607);
#1912=VERTEX_POINT('',#42609);
#1913=VERTEX_POINT('',#42613);
#1914=VERTEX_POINT('',#42614);
#1915=VERTEX_POINT('',#42619);
#1916=VERTEX_POINT('',#42623);
#1917=VERTEX_POINT('',#42627);
#1918=VERTEX_POINT('',#42631);
#1919=EDGE_CURVE('',#1477,#1478,#1051,.T.);
#1920=EDGE_CURVE('',#1479,#1477,#1052,.T.);
#1921=EDGE_CURVE('',#1479,#1480,#1053,.T.);
#1922=EDGE_CURVE('',#1480,#1481,#1054,.T.);
#1923=EDGE_CURVE('',#1481,#1478,#1055,.T.);
#1924=EDGE_CURVE('',#1482,#1477,#1056,.T.);
#1925=EDGE_CURVE('',#1483,#1482,#1057,.T.);
#1926=EDGE_CURVE('',#1483,#1484,#1058,.T.);
#1927=EDGE_CURVE('',#1484,#1479,#1059,.T.);
#1928=EDGE_CURVE('',#1478,#1485,#1060,.T.);
#1929=EDGE_CURVE('',#1481,#1486,#1061,.T.);
#1930=EDGE_CURVE('',#1486,#1487,#1062,.T.);
#1931=EDGE_CURVE('',#1487,#1485,#1063,.T.);
#1932=EDGE_CURVE('',#1488,#1482,#1064,.T.);
#1933=EDGE_CURVE('',#1489,#1488,#1065,.T.);
#1934=EDGE_CURVE('',#1489,#1490,#1066,.T.);
#1935=EDGE_CURVE('',#1490,#1483,#1067,.T.);
#1936=EDGE_CURVE('',#1491,#1492,#519,.T.);
#1937=EDGE_CURVE('',#1493,#1491,#1068,.T.);
#1938=EDGE_CURVE('',#1492,#1493,#1069,.T.);
#1939=EDGE_CURVE('',#1492,#1486,#520,.T.);
#1940=EDGE_CURVE('',#1487,#1492,#1070,.T.);
#1941=EDGE_CURVE('',#1486,#1480,#521,.T.);
#1942=EDGE_CURVE('',#1480,#1484,#522,.T.);
#1943=EDGE_CURVE('',#1484,#1490,#523,.T.);
#1944=EDGE_CURVE('',#1490,#1494,#524,.T.);
#1945=EDGE_CURVE('',#1491,#1489,#1071,.T.);
#1946=EDGE_CURVE('',#1494,#1491,#525,.T.);
#1947=EDGE_CURVE('',#1485,#1495,#1072,.T.);
#1948=EDGE_CURVE('',#1495,#1493,#1073,.T.);
#1949=EDGE_CURVE('',#1495,#1488,#1074,.T.);
#1950=EDGE_CURVE('',#1496,#1496,#526,.T.);
#1951=EDGE_CURVE('',#1496,#1497,#527,.T.);
#1952=EDGE_CURVE('',#1497,#1497,#528,.T.);
#1953=EDGE_CURVE('',#1497,#1498,#1075,.T.);
#1954=EDGE_CURVE('',#1498,#1498,#529,.T.);
#1955=EDGE_CURVE('',#1498,#1499,#530,.T.);
#1956=EDGE_CURVE('',#1499,#1499,#531,.T.);
#1957=EDGE_CURVE('',#1500,#1500,#532,.T.);
#1958=EDGE_CURVE('',#1501,#1502,#533,.T.);
#1959=EDGE_CURVE('',#1502,#1500,#534,.T.);
#1960=EDGE_CURVE('',#1502,#1501,#535,.T.);
#1961=EDGE_CURVE('',#1501,#1503,#1076,.T.);
#1962=EDGE_CURVE('',#1504,#1503,#94,.T.);
#1963=EDGE_CURVE('',#1503,#1504,#95,.T.);
#1964=EDGE_CURVE('',#1505,#1504,#96,.T.);
#1965=EDGE_CURVE('',#1505,#1505,#97,.T.);
#1966=EDGE_CURVE('',#1506,#1506,#536,.T.);
#1967=EDGE_CURVE('',#1506,#1507,#1077,.T.);
#1968=EDGE_CURVE('',#1507,#1507,#537,.T.);
#1969=EDGE_CURVE('',#1508,#1509,#98,.T.);
#1970=EDGE_CURVE('',#1509,#1508,#99,.T.);
#1971=EDGE_CURVE('',#1509,#1494,#1078,.T.);
#1972=EDGE_CURVE('',#1510,#1510,#538,.T.);
#1973=EDGE_CURVE('',#1510,#1511,#1079,.T.);
#1974=EDGE_CURVE('',#1511,#1511,#539,.T.);
#1975=EDGE_CURVE('',#1512,#1512,#540,.T.);
#1976=EDGE_CURVE('',#1513,#1513,#541,.T.);
#1977=EDGE_CURVE('',#1513,#1514,#1080,.T.);
#1978=EDGE_CURVE('',#1514,#1514,#542,.T.);
#1979=EDGE_CURVE('',#1515,#1515,#543,.T.);
#1980=EDGE_CURVE('',#1515,#1512,#1081,.T.);
#1981=EDGE_CURVE('',#1516,#1517,#544,.T.);
#1982=EDGE_CURVE('',#1517,#1518,#1082,.T.);
#1983=EDGE_CURVE('',#1518,#1519,#545,.T.);
#1984=EDGE_CURVE('',#1519,#1516,#1083,.T.);
#1985=EDGE_CURVE('',#1520,#1521,#546,.T.);
#1986=EDGE_CURVE('',#1521,#1519,#547,.T.);
#1987=EDGE_CURVE('',#1518,#1520,#548,.T.);
#1988=EDGE_CURVE('',#1522,#1523,#549,.T.);
#1989=EDGE_CURVE('',#1523,#1521,#1084,.T.);
#1990=EDGE_CURVE('',#1520,#1522,#1085,.T.);
#1991=EDGE_CURVE('',#1519,#1524,#1086,.T.);
#1992=EDGE_CURVE('',#1525,#1524,#1087,.T.);
#1993=EDGE_CURVE('',#1516,#1525,#1088,.T.);
#1994=EDGE_CURVE('',#1521,#1526,#1089,.T.);
#1995=EDGE_CURVE('',#1524,#1526,#550,.T.);
#1996=EDGE_CURVE('',#1523,#1527,#1090,.T.);
#1997=EDGE_CURVE('',#1526,#1527,#1091,.T.);
#1998=EDGE_CURVE('',#1527,#1528,#551,.T.);
#1999=EDGE_CURVE('',#1528,#1529,#1092,.T.);
#2000=EDGE_CURVE('',#1529,#1526,#552,.T.);
#2001=EDGE_CURVE('',#1530,#1524,#553,.T.);
#2002=EDGE_CURVE('',#1529,#1530,#554,.T.);
#2003=EDGE_CURVE('',#1531,#1525,#555,.T.);
#2004=EDGE_CURVE('',#1530,#1531,#1093,.T.);
#2005=EDGE_CURVE('',#1531,#1528,#1094,.T.);
#2006=EDGE_CURVE('',#1517,#1522,#1095,.T.);
#2007=EDGE_CURVE('',#1532,#1533,#1096,.T.);
#2008=EDGE_CURVE('',#1534,#1533,#1097,.T.);
#2009=EDGE_CURVE('',#1535,#1534,#1098,.T.);
#2010=EDGE_CURVE('',#1535,#1532,#1099,.T.);
#2011=EDGE_CURVE('',#1536,#1537,#556,.T.);
#2012=EDGE_CURVE('',#1537,#1538,#1100,.T.);
#2013=EDGE_CURVE('',#1538,#1539,#557,.T.);
#2014=EDGE_CURVE('',#1536,#1539,#1101,.T.);
#2015=EDGE_CURVE('',#1539,#1532,#1102,.T.);
#2016=EDGE_CURVE('',#1535,#1536,#1103,.T.);
#2017=EDGE_CURVE('',#1540,#1537,#558,.T.);
#2018=EDGE_CURVE('',#1540,#1541,#1104,.T.);
#2019=EDGE_CURVE('',#1538,#1541,#559,.T.);
#2020=EDGE_CURVE('',#1534,#1540,#1105,.T.);
#2021=EDGE_CURVE('',#1541,#1533,#1106,.T.);
#2022=EDGE_CURVE('',#1542,#1542,#560,.T.);
#2023=EDGE_CURVE('',#1543,#1544,#1107,.T.);
#2024=EDGE_CURVE('',#1545,#1543,#100,.T.);
#2025=EDGE_CURVE('',#1545,#1544,#561,.T.);
#2026=EDGE_CURVE('',#1546,#1547,#1108,.T.);
#2027=EDGE_CURVE('',#1548,#1546,#101,.T.);
#2028=EDGE_CURVE('',#1543,#1548,#102,.T.);
#2029=EDGE_CURVE('',#1544,#1549,#562,.T.);
#2030=EDGE_CURVE('',#1549,#1550,#103,.T.);
#2031=EDGE_CURVE('',#1550,#1547,#104,.T.);
#2032=EDGE_CURVE('',#1551,#1552,#1109,.T.);
#2033=EDGE_CURVE('',#1553,#1551,#105,.T.);
#2034=EDGE_CURVE('',#1546,#1553,#106,.T.);
#2035=EDGE_CURVE('',#1547,#1554,#107,.T.);
#2036=EDGE_CURVE('',#1554,#1552,#108,.T.);
#2037=EDGE_CURVE('',#1555,#1556,#1110,.T.);
#2038=EDGE_CURVE('',#1557,#1555,#109,.T.);
#2039=EDGE_CURVE('',#1551,#1557,#110,.T.);
#2040=EDGE_CURVE('',#1552,#1558,#111,.T.);
#2041=EDGE_CURVE('',#1558,#1556,#112,.T.);
#2042=EDGE_CURVE('',#1559,#1560,#1111,.T.);
#2043=EDGE_CURVE('',#1561,#1559,#113,.T.);
#2044=EDGE_CURVE('',#1555,#1561,#114,.T.);
#2045=EDGE_CURVE('',#1556,#1562,#115,.T.);
#2046=EDGE_CURVE('',#1562,#1560,#116,.T.);
#2047=EDGE_CURVE('',#1563,#1564,#1112,.T.);
#2048=EDGE_CURVE('',#1565,#1563,#117,.T.);
#2049=EDGE_CURVE('',#1559,#1565,#118,.T.);
#2050=EDGE_CURVE('',#1560,#1566,#119,.T.);
#2051=EDGE_CURVE('',#1566,#1564,#120,.T.);
#2052=EDGE_CURVE('',#1567,#1568,#1113,.T.);
#2053=EDGE_CURVE('',#1569,#1567,#121,.T.);
#2054=EDGE_CURVE('',#1563,#1569,#122,.T.);
#2055=EDGE_CURVE('',#1564,#1570,#123,.T.);
#2056=EDGE_CURVE('',#1570,#1568,#124,.T.);
#2057=EDGE_CURVE('',#1571,#1572,#1114,.T.);
#2058=EDGE_CURVE('',#1573,#1571,#125,.T.);
#2059=EDGE_CURVE('',#1574,#1573,#126,.T.);
#2060=EDGE_CURVE('',#1575,#1574,#563,.F.);
#2061=EDGE_CURVE('',#1572,#1575,#127,.F.);
#2062=EDGE_CURVE('',#1576,#1577,#1115,.T.);
#2063=EDGE_CURVE('',#1578,#1576,#128,.F.);
#2064=EDGE_CURVE('',#1571,#1578,#129,.T.);
#2065=EDGE_CURVE('',#1577,#1572,#130,.F.);
#2066=EDGE_CURVE('',#1579,#1580,#1116,.T.);
#2067=EDGE_CURVE('',#1576,#1579,#131,.F.);
#2068=EDGE_CURVE('',#1580,#1577,#132,.F.);
#2069=EDGE_CURVE('',#1581,#1582,#1117,.T.);
#2070=EDGE_CURVE('',#1583,#1581,#133,.F.);
#2071=EDGE_CURVE('',#1579,#1583,#134,.F.);
#2072=EDGE_CURVE('',#1582,#1580,#135,.F.);
#2073=EDGE_CURVE('',#1584,#1585,#1118,.T.);
#2074=EDGE_CURVE('',#1581,#1584,#136,.F.);
#2075=EDGE_CURVE('',#1585,#1582,#137,.F.);
#2076=EDGE_CURVE('',#1586,#1587,#1119,.T.);
#2077=EDGE_CURVE('',#1588,#1586,#138,.T.);
#2078=EDGE_CURVE('',#1584,#1588,#139,.F.);
#2079=EDGE_CURVE('',#1587,#1585,#140,.F.);
#2080=EDGE_CURVE('',#1589,#1587,#141,.F.);
#2081=EDGE_CURVE('',#1589,#1590,#564,.F.);
#2082=EDGE_CURVE('',#1586,#1590,#142,.T.);
#2083=EDGE_CURVE('',#1568,#1591,#143,.T.);
#2084=EDGE_CURVE('',#1591,#1592,#144,.T.);
#2085=EDGE_CURVE('',#1592,#1593,#565,.T.);
#2086=EDGE_CURVE('',#1594,#1593,#145,.T.);
#2087=EDGE_CURVE('',#1567,#1594,#146,.T.);
#2088=EDGE_CURVE('',#1593,#1595,#147,.T.);
#2089=EDGE_CURVE('',#1595,#1589,#148,.T.);
#2090=EDGE_CURVE('',#1575,#1545,#149,.T.);
#2091=EDGE_CURVE('',#1590,#1592,#150,.T.);
#2092=EDGE_CURVE('',#1549,#1574,#151,.T.);
#2093=EDGE_CURVE('',#1596,#1597,#1120,.T.);
#2094=EDGE_CURVE('',#1598,#1596,#1121,.T.);
#2095=EDGE_CURVE('',#1599,#1598,#1122,.T.);
#2096=EDGE_CURVE('',#1600,#1599,#1123,.T.);
#2097=EDGE_CURVE('',#1601,#1600,#1124,.T.);
#2098=EDGE_CURVE('',#1597,#1601,#1125,.T.);
#2099=EDGE_CURVE('',#1602,#1603,#1126,.T.);
#2100=EDGE_CURVE('',#1602,#1598,#1127,.T.);
#2101=EDGE_CURVE('',#1603,#1596,#1128,.T.);
#2102=EDGE_CURVE('',#1604,#1602,#1129,.T.);
#2103=EDGE_CURVE('',#1604,#1599,#1130,.T.);
#2104=EDGE_CURVE('',#1605,#1604,#1131,.T.);
#2105=EDGE_CURVE('',#1605,#1600,#1132,.T.);
#2106=EDGE_CURVE('',#1606,#1605,#1133,.T.);
#2107=EDGE_CURVE('',#1606,#1601,#1134,.T.);
#2108=EDGE_CURVE('',#1607,#1606,#1135,.T.);
#2109=EDGE_CURVE('',#1607,#1597,#1136,.T.);
#2110=EDGE_CURVE('',#1603,#1607,#1137,.T.);
#2111=EDGE_CURVE('',#1608,#1609,#1138,.T.);
#2112=EDGE_CURVE('',#1610,#1608,#152,.T.);
#2113=EDGE_CURVE('',#1611,#1610,#566,.T.);
#2114=EDGE_CURVE('',#1611,#1609,#153,.T.);
#2115=EDGE_CURVE('',#1612,#1613,#1139,.T.);
#2116=EDGE_CURVE('',#1614,#1612,#154,.F.);
#2117=EDGE_CURVE('',#1608,#1614,#155,.T.);
#2118=EDGE_CURVE('',#1609,#1615,#156,.T.);
#2119=EDGE_CURVE('',#1615,#1613,#157,.T.);
#2120=EDGE_CURVE('',#1616,#1617,#1140,.T.);
#2121=EDGE_CURVE('',#1612,#1616,#158,.F.);
#2122=EDGE_CURVE('',#1613,#1617,#159,.T.);
#2123=EDGE_CURVE('',#1618,#1619,#1141,.T.);
#2124=EDGE_CURVE('',#1620,#1618,#160,.F.);
#2125=EDGE_CURVE('',#1616,#1620,#161,.F.);
#2126=EDGE_CURVE('',#1617,#1621,#162,.T.);
#2127=EDGE_CURVE('',#1621,#1619,#163,.T.);
#2128=EDGE_CURVE('',#1622,#1623,#1142,.T.);
#2129=EDGE_CURVE('',#1618,#1622,#164,.F.);
#2130=EDGE_CURVE('',#1619,#1624,#165,.T.);
#2131=EDGE_CURVE('',#1624,#1623,#166,.T.);
#2132=EDGE_CURVE('',#1625,#1626,#1143,.T.);
#2133=EDGE_CURVE('',#1627,#1625,#167,.F.);
#2134=EDGE_CURVE('',#1622,#1627,#168,.F.);
#2135=EDGE_CURVE('',#1623,#1626,#169,.T.);
#2136=EDGE_CURVE('',#1628,#1629,#1144,.T.);
#2137=EDGE_CURVE('',#1625,#1628,#170,.F.);
#2138=EDGE_CURVE('',#1626,#1630,#171,.T.);
#2139=EDGE_CURVE('',#1630,#1629,#172,.T.);
#2140=EDGE_CURVE('',#1631,#1632,#1145,.T.);
#2141=EDGE_CURVE('',#1633,#1631,#173,.F.);
#2142=EDGE_CURVE('',#1628,#1633,#174,.F.);
#2143=EDGE_CURVE('',#1629,#1632,#175,.T.);
#2144=EDGE_CURVE('',#1634,#1635,#1146,.T.);
#2145=EDGE_CURVE('',#1631,#1634,#176,.F.);
#2146=EDGE_CURVE('',#1632,#1636,#177,.T.);
#2147=EDGE_CURVE('',#1636,#1635,#178,.T.);
#2148=EDGE_CURVE('',#1637,#1638,#1147,.T.);
#2149=EDGE_CURVE('',#1639,#1637,#179,.F.);
#2150=EDGE_CURVE('',#1634,#1639,#180,.F.);
#2151=EDGE_CURVE('',#1635,#1638,#181,.T.);
#2152=EDGE_CURVE('',#1640,#1641,#1148,.T.);
#2153=EDGE_CURVE('',#1637,#1640,#182,.F.);
#2154=EDGE_CURVE('',#1638,#1642,#183,.T.);
#2155=EDGE_CURVE('',#1642,#1641,#184,.T.);
#2156=EDGE_CURVE('',#1643,#1644,#1149,.T.);
#2157=EDGE_CURVE('',#1645,#1643,#185,.T.);
#2158=EDGE_CURVE('',#1640,#1645,#186,.F.);
#2159=EDGE_CURVE('',#1641,#1644,#187,.T.);
#2160=EDGE_CURVE('',#1646,#1647,#1150,.T.);
#2161=EDGE_CURVE('',#1648,#1646,#188,.F.);
#2162=EDGE_CURVE('',#1643,#1648,#189,.T.);
#2163=EDGE_CURVE('',#1644,#1649,#190,.T.);
#2164=EDGE_CURVE('',#1649,#1647,#191,.T.);
#2165=EDGE_CURVE('',#1650,#1651,#1151,.T.);
#2166=EDGE_CURVE('',#1646,#1650,#192,.F.);
#2167=EDGE_CURVE('',#1647,#1651,#193,.T.);
#2168=EDGE_CURVE('',#1652,#1653,#1152,.T.);
#2169=EDGE_CURVE('',#1654,#1652,#194,.F.);
#2170=EDGE_CURVE('',#1650,#1654,#195,.F.);
#2171=EDGE_CURVE('',#1651,#1655,#196,.T.);
#2172=EDGE_CURVE('',#1655,#1653,#197,.T.);
#2173=EDGE_CURVE('',#1656,#1657,#1153,.T.);
#2174=EDGE_CURVE('',#1652,#1656,#198,.F.);
#2175=EDGE_CURVE('',#1653,#1657,#199,.T.);
#2176=EDGE_CURVE('',#1658,#1659,#1154,.T.);
#2177=EDGE_CURVE('',#1660,#1658,#200,.F.);
#2178=EDGE_CURVE('',#1656,#1660,#201,.F.);
#2179=EDGE_CURVE('',#1657,#1661,#202,.T.);
#2180=EDGE_CURVE('',#1661,#1659,#203,.T.);
#2181=EDGE_CURVE('',#1662,#1663,#1155,.T.);
#2182=EDGE_CURVE('',#1658,#1662,#204,.F.);
#2183=EDGE_CURVE('',#1659,#1664,#205,.T.);
#2184=EDGE_CURVE('',#1664,#1663,#206,.T.);
#2185=EDGE_CURVE('',#1665,#1666,#1156,.T.);
#2186=EDGE_CURVE('',#1667,#1665,#207,.F.);
#2187=EDGE_CURVE('',#1662,#1667,#208,.F.);
#2188=EDGE_CURVE('',#1663,#1666,#209,.T.);
#2189=EDGE_CURVE('',#1668,#1669,#1157,.T.);
#2190=EDGE_CURVE('',#1665,#1668,#210,.F.);
#2191=EDGE_CURVE('',#1666,#1670,#211,.T.);
#2192=EDGE_CURVE('',#1670,#1669,#212,.T.);
#2193=EDGE_CURVE('',#1671,#1672,#1158,.T.);
#2194=EDGE_CURVE('',#1673,#1671,#213,.F.);
#2195=EDGE_CURVE('',#1668,#1673,#214,.F.);
#2196=EDGE_CURVE('',#1669,#1672,#215,.T.);
#2197=EDGE_CURVE('',#1674,#1675,#1159,.T.);
#2198=EDGE_CURVE('',#1671,#1674,#216,.F.);
#2199=EDGE_CURVE('',#1672,#1676,#217,.T.);
#2200=EDGE_CURVE('',#1676,#1675,#218,.T.);
#2201=EDGE_CURVE('',#1677,#1678,#1160,.T.);
#2202=EDGE_CURVE('',#1679,#1677,#219,.F.);
#2203=EDGE_CURVE('',#1674,#1679,#220,.F.);
#2204=EDGE_CURVE('',#1675,#1678,#221,.T.);
#2205=EDGE_CURVE('',#1680,#1681,#1161,.T.);
#2206=EDGE_CURVE('',#1677,#1680,#222,.F.);
#2207=EDGE_CURVE('',#1678,#1682,#223,.T.);
#2208=EDGE_CURVE('',#1682,#1681,#224,.T.);
#2209=EDGE_CURVE('',#1683,#1684,#1162,.T.);
#2210=EDGE_CURVE('',#1685,#1683,#225,.T.);
#2211=EDGE_CURVE('',#1680,#1685,#226,.F.);
#2212=EDGE_CURVE('',#1681,#1684,#227,.T.);
#2213=EDGE_CURVE('',#1686,#1687,#1163,.T.);
#2214=EDGE_CURVE('',#1688,#1686,#228,.F.);
#2215=EDGE_CURVE('',#1683,#1688,#229,.T.);
#2216=EDGE_CURVE('',#1684,#1689,#230,.T.);
#2217=EDGE_CURVE('',#1689,#1687,#231,.T.);
#2218=EDGE_CURVE('',#1690,#1691,#1164,.T.);
#2219=EDGE_CURVE('',#1686,#1690,#232,.F.);
#2220=EDGE_CURVE('',#1687,#1691,#233,.T.);
#2221=EDGE_CURVE('',#1692,#1693,#1165,.T.);
#2222=EDGE_CURVE('',#1694,#1692,#234,.T.);
#2223=EDGE_CURVE('',#1690,#1694,#235,.F.);
#2224=EDGE_CURVE('',#1691,#1695,#236,.T.);
#2225=EDGE_CURVE('',#1695,#1693,#237,.F.);
#2226=EDGE_CURVE('',#1696,#1697,#238,.T.);
#2227=EDGE_CURVE('',#1698,#1697,#567,.T.);
#2228=EDGE_CURVE('',#1698,#1699,#239,.T.);
#2229=EDGE_CURVE('',#1699,#1700,#240,.T.);
#2230=EDGE_CURVE('',#1700,#1701,#241,.T.);
#2231=EDGE_CURVE('',#1701,#1702,#242,.T.);
#2232=EDGE_CURVE('',#1702,#1703,#243,.T.);
#2233=EDGE_CURVE('',#1703,#1704,#244,.T.);
#2234=EDGE_CURVE('',#1704,#1705,#245,.T.);
#2235=EDGE_CURVE('',#1705,#1706,#246,.T.);
#2236=EDGE_CURVE('',#1706,#1707,#247,.T.);
#2237=EDGE_CURVE('',#1707,#1708,#248,.T.);
#2238=EDGE_CURVE('',#1708,#1709,#249,.T.);
#2239=EDGE_CURVE('',#1709,#1710,#250,.T.);
#2240=EDGE_CURVE('',#1710,#1711,#251,.T.);
#2241=EDGE_CURVE('',#1711,#1712,#252,.T.);
#2242=EDGE_CURVE('',#1712,#1713,#253,.T.);
#2243=EDGE_CURVE('',#1713,#1714,#254,.T.);
#2244=EDGE_CURVE('',#1714,#1715,#255,.T.);
#2245=EDGE_CURVE('',#1715,#1716,#256,.T.);
#2246=EDGE_CURVE('',#1716,#1717,#257,.T.);
#2247=EDGE_CURVE('',#1717,#1718,#258,.T.);
#2248=EDGE_CURVE('',#1718,#1719,#259,.T.);
#2249=EDGE_CURVE('',#1719,#1720,#260,.T.);
#2250=EDGE_CURVE('',#1720,#1721,#261,.T.);
#2251=EDGE_CURVE('',#1721,#1722,#262,.T.);
#2252=EDGE_CURVE('',#1722,#1723,#263,.T.);
#2253=EDGE_CURVE('',#1723,#1724,#264,.T.);
#2254=EDGE_CURVE('',#1724,#1725,#265,.T.);
#2255=EDGE_CURVE('',#1725,#1726,#266,.T.);
#2256=EDGE_CURVE('',#1726,#1727,#267,.T.);
#2257=EDGE_CURVE('',#1728,#1727,#568,.F.);
#2258=EDGE_CURVE('',#1728,#1729,#268,.T.);
#2259=EDGE_CURVE('',#1729,#1730,#269,.T.);
#2260=EDGE_CURVE('',#1730,#1731,#270,.T.);
#2261=EDGE_CURVE('',#1731,#1732,#271,.T.);
#2262=EDGE_CURVE('',#1732,#1733,#272,.T.);
#2263=EDGE_CURVE('',#1733,#1734,#273,.T.);
#2264=EDGE_CURVE('',#1734,#1735,#274,.T.);
#2265=EDGE_CURVE('',#1735,#1736,#275,.T.);
#2266=EDGE_CURVE('',#1736,#1737,#276,.T.);
#2267=EDGE_CURVE('',#1737,#1738,#277,.T.);
#2268=EDGE_CURVE('',#1738,#1739,#278,.T.);
#2269=EDGE_CURVE('',#1739,#1740,#279,.T.);
#2270=EDGE_CURVE('',#1740,#1741,#280,.T.);
#2271=EDGE_CURVE('',#1741,#1742,#281,.T.);
#2272=EDGE_CURVE('',#1742,#1743,#282,.T.);
#2273=EDGE_CURVE('',#1743,#1744,#283,.T.);
#2274=EDGE_CURVE('',#1744,#1745,#284,.T.);
#2275=EDGE_CURVE('',#1745,#1746,#285,.T.);
#2276=EDGE_CURVE('',#1746,#1747,#286,.T.);
#2277=EDGE_CURVE('',#1747,#1748,#287,.T.);
#2278=EDGE_CURVE('',#1748,#1749,#288,.T.);
#2279=EDGE_CURVE('',#1749,#1750,#289,.T.);
#2280=EDGE_CURVE('',#1750,#1751,#290,.T.);
#2281=EDGE_CURVE('',#1751,#1752,#291,.T.);
#2282=EDGE_CURVE('',#1752,#1753,#292,.T.);
#2283=EDGE_CURVE('',#1753,#1754,#293,.T.);
#2284=EDGE_CURVE('',#1754,#1755,#294,.T.);
#2285=EDGE_CURVE('',#1755,#1696,#295,.T.);
#2286=EDGE_CURVE('',#1693,#1756,#296,.F.);
#2287=EDGE_CURVE('',#1757,#1756,#569,.T.);
#2288=EDGE_CURVE('',#1758,#1757,#297,.T.);
#2289=EDGE_CURVE('',#1692,#1758,#298,.T.);
#2290=EDGE_CURVE('',#1727,#1757,#299,.T.);
#2291=EDGE_CURVE('',#1610,#1698,#300,.T.);
#2292=EDGE_CURVE('',#1759,#1728,#301,.T.);
#2293=EDGE_CURVE('',#1756,#1759,#302,.T.);
#2294=EDGE_CURVE('',#1697,#1611,#303,.T.);
#2295=EDGE_CURVE('',#1760,#1760,#570,.T.);
#2296=EDGE_CURVE('',#1761,#1761,#571,.T.);
#2297=EDGE_CURVE('',#1761,#1762,#1166,.T.);
#2298=EDGE_CURVE('',#1762,#1762,#572,.T.);
#2299=EDGE_CURVE('',#1763,#1764,#1167,.T.);
#2300=EDGE_CURVE('',#1764,#1765,#1168,.T.);
#2301=EDGE_CURVE('',#1765,#1766,#1169,.T.);
#2302=EDGE_CURVE('',#1766,#1767,#1170,.T.);
#2303=EDGE_CURVE('',#1767,#1768,#1171,.T.);
#2304=EDGE_CURVE('',#1768,#1763,#1172,.T.);
#2305=EDGE_CURVE('',#1769,#1764,#1173,.T.);
#2306=EDGE_CURVE('',#1770,#1769,#1174,.T.);
#2307=EDGE_CURVE('',#1770,#1765,#1175,.T.);
#2308=EDGE_CURVE('',#1771,#1770,#1176,.T.);
#2309=EDGE_CURVE('',#1771,#1766,#1177,.T.);
#2310=EDGE_CURVE('',#1772,#1771,#1178,.T.);
#2311=EDGE_CURVE('',#1772,#1767,#1179,.T.);
#2312=EDGE_CURVE('',#1773,#1772,#1180,.T.);
#2313=EDGE_CURVE('',#1773,#1768,#1181,.T.);
#2314=EDGE_CURVE('',#1774,#1773,#1182,.T.);
#2315=EDGE_CURVE('',#1763,#1774,#1183,.T.);
#2316=EDGE_CURVE('',#1769,#1774,#1184,.T.);
#2317=EDGE_CURVE('',#1775,#1776,#1185,.T.);
#2318=EDGE_CURVE('',#1777,#1776,#304,.T.);
#2319=EDGE_CURVE('',#1778,#1777,#573,.T.);
#2320=EDGE_CURVE('',#1775,#1778,#305,.T.);
#2321=EDGE_CURVE('',#1779,#1780,#1186,.T.);
#2322=EDGE_CURVE('',#1781,#1779,#306,.T.);
#2323=EDGE_CURVE('',#1782,#1781,#574,.T.);
#2324=EDGE_CURVE('',#1780,#1782,#307,.T.);
#2325=EDGE_CURVE('',#1783,#1784,#1187,.T.);
#2326=EDGE_CURVE('',#1784,#1785,#308,.T.);
#2327=EDGE_CURVE('',#1786,#1785,#575,.T.);
#2328=EDGE_CURVE('',#1787,#1786,#309,.T.);
#2329=EDGE_CURVE('',#1783,#1787,#310,.T.);
#2330=EDGE_CURVE('',#1788,#1789,#1188,.T.);
#2331=EDGE_CURVE('',#1789,#1790,#311,.F.);
#2332=EDGE_CURVE('',#1790,#1784,#312,.T.);
#2333=EDGE_CURVE('',#1788,#1783,#313,.T.);
#2334=EDGE_CURVE('',#1791,#1792,#1189,.T.);
#2335=EDGE_CURVE('',#1793,#1791,#576,.T.);
#2336=EDGE_CURVE('',#1793,#1792,#314,.F.);
#2337=EDGE_CURVE('',#1781,#1793,#315,.T.);
#2338=EDGE_CURVE('',#1779,#1775,#316,.T.);
#2339=EDGE_CURVE('',#1785,#1778,#317,.T.);
#2340=EDGE_CURVE('',#1792,#1789,#318,.F.);
#2341=EDGE_CURVE('',#1794,#1788,#319,.T.);
#2342=EDGE_CURVE('',#1795,#1794,#320,.T.);
#2343=EDGE_CURVE('',#1791,#1795,#577,.T.);
#2344=EDGE_CURVE('',#1776,#1780,#321,.T.);
#2345=EDGE_CURVE('',#1795,#1782,#322,.T.);
#2346=EDGE_CURVE('',#1777,#1786,#323,.T.);
#2347=EDGE_CURVE('',#1796,#1797,#578,.T.);
#2348=EDGE_CURVE('',#1797,#1798,#579,.T.);
#2349=EDGE_CURVE('',#1798,#1799,#580,.T.);
#2350=EDGE_CURVE('',#1799,#1796,#581,.T.);
#2351=EDGE_CURVE('',#1800,#1801,#582,.T.);
#2352=EDGE_CURVE('',#1801,#1799,#1190,.T.);
#2353=EDGE_CURVE('',#1798,#1800,#1191,.T.);
#2354=EDGE_CURVE('',#1802,#1803,#583,.T.);
#2355=EDGE_CURVE('',#1803,#1801,#584,.T.);
#2356=EDGE_CURVE('',#1800,#1802,#585,.T.);
#2357=EDGE_CURVE('',#1804,#1805,#586,.T.);
#2358=EDGE_CURVE('',#1805,#1803,#1192,.T.);
#2359=EDGE_CURVE('',#1802,#1804,#1193,.T.);
#2360=EDGE_CURVE('',#1806,#1807,#587,.T.);
#2361=EDGE_CURVE('',#1807,#1805,#588,.T.);
#2362=EDGE_CURVE('',#1804,#1806,#589,.T.);
#2363=EDGE_CURVE('',#1808,#1809,#590,.T.);
#2364=EDGE_CURVE('',#1809,#1807,#1194,.T.);
#2365=EDGE_CURVE('',#1806,#1808,#1195,.T.);
#2366=EDGE_CURVE('',#1810,#1811,#591,.T.);
#2367=EDGE_CURVE('',#1811,#1809,#592,.T.);
#2368=EDGE_CURVE('',#1808,#1810,#593,.T.);
#2369=EDGE_CURVE('',#1812,#1813,#594,.T.);
#2370=EDGE_CURVE('',#1813,#1811,#1196,.T.);
#2371=EDGE_CURVE('',#1810,#1812,#1197,.T.);
#2372=EDGE_CURVE('',#1814,#1815,#595,.T.);
#2373=EDGE_CURVE('',#1815,#1813,#596,.T.);
#2374=EDGE_CURVE('',#1812,#1814,#597,.T.);
#2375=EDGE_CURVE('',#1816,#1817,#598,.T.);
#2376=EDGE_CURVE('',#1817,#1815,#1198,.T.);
#2377=EDGE_CURVE('',#1814,#1816,#1199,.T.);
#2378=EDGE_CURVE('',#1818,#1819,#599,.T.);
#2379=EDGE_CURVE('',#1819,#1817,#600,.T.);
#2380=EDGE_CURVE('',#1816,#1818,#601,.T.);
#2381=EDGE_CURVE('',#1820,#1821,#602,.T.);
#2382=EDGE_CURVE('',#1821,#1819,#1200,.T.);
#2383=EDGE_CURVE('',#1818,#1820,#1201,.T.);
#2384=EDGE_CURVE('',#1822,#1823,#603,.T.);
#2385=EDGE_CURVE('',#1823,#1821,#604,.T.);
#2386=EDGE_CURVE('',#1820,#1822,#605,.T.);
#2387=EDGE_CURVE('',#1822,#1797,#1202,.T.);
#2388=EDGE_CURVE('',#1796,#1823,#1203,.T.);
#2389=EDGE_CURVE('',#1808,#1824,#1204,.T.);
#2390=EDGE_CURVE('',#1825,#1824,#606,.T.);
#2391=EDGE_CURVE('',#1825,#1810,#1205,.T.);
#2392=EDGE_CURVE('',#1826,#1806,#1206,.T.);
#2393=EDGE_CURVE('',#1824,#1826,#1207,.T.);
#2394=EDGE_CURVE('',#1804,#1827,#1208,.T.);
#2395=EDGE_CURVE('',#1826,#1827,#607,.T.);
#2396=EDGE_CURVE('',#1828,#1822,#1209,.T.);
#2397=EDGE_CURVE('',#1829,#1828,#1210,.T.);
#2398=EDGE_CURVE('',#1830,#1829,#608,.T.);
#2399=EDGE_CURVE('',#1831,#1830,#1211,.T.);
#2400=EDGE_CURVE('',#1832,#1831,#609,.T.);
#2401=EDGE_CURVE('',#1827,#1832,#1212,.T.);
#2402=EDGE_CURVE('',#1819,#1796,#1213,.T.);
#2403=EDGE_CURVE('',#1815,#1801,#1214,.T.);
#2404=EDGE_CURVE('',#1803,#1813,#1215,.T.);
#2405=EDGE_CURVE('',#1799,#1817,#1216,.T.);
#2406=EDGE_CURVE('',#1833,#1834,#610,.T.);
#2407=EDGE_CURVE('',#1834,#1835,#611,.T.);
#2408=EDGE_CURVE('',#1835,#1836,#612,.T.);
#2409=EDGE_CURVE('',#1836,#1833,#613,.T.);
#2410=EDGE_CURVE('',#1837,#1838,#614,.T.);
#2411=EDGE_CURVE('',#1838,#1836,#1217,.T.);
#2412=EDGE_CURVE('',#1835,#1837,#1218,.T.);
#2413=EDGE_CURVE('',#1839,#1840,#615,.T.);
#2414=EDGE_CURVE('',#1840,#1838,#616,.T.);
#2415=EDGE_CURVE('',#1837,#1839,#617,.T.);
#2416=EDGE_CURVE('',#1825,#1841,#618,.T.);
#2417=EDGE_CURVE('',#1841,#1840,#1219,.T.);
#2418=EDGE_CURVE('',#1839,#1825,#1220,.T.);
#2419=EDGE_CURVE('',#1824,#1842,#619,.T.);
#2420=EDGE_CURVE('',#1842,#1841,#620,.T.);
#2421=EDGE_CURVE('',#1826,#1843,#621,.T.);
#2422=EDGE_CURVE('',#1843,#1842,#1221,.T.);
#2423=EDGE_CURVE('',#1827,#1844,#622,.T.);
#2424=EDGE_CURVE('',#1844,#1843,#623,.T.);
#2425=EDGE_CURVE('',#1832,#1845,#624,.T.);
#2426=EDGE_CURVE('',#1845,#1844,#1222,.T.);
#2427=EDGE_CURVE('',#1831,#1846,#625,.T.);
#2428=EDGE_CURVE('',#1846,#1845,#626,.T.);
#2429=EDGE_CURVE('',#1830,#1847,#627,.T.);
#2430=EDGE_CURVE('',#1847,#1846,#1223,.T.);
#2431=EDGE_CURVE('',#1829,#1848,#628,.T.);
#2432=EDGE_CURVE('',#1848,#1847,#629,.T.);
#2433=EDGE_CURVE('',#1828,#1849,#630,.T.);
#2434=EDGE_CURVE('',#1849,#1848,#1224,.T.);
#2435=EDGE_CURVE('',#1850,#1851,#631,.T.);
#2436=EDGE_CURVE('',#1851,#1849,#632,.T.);
#2437=EDGE_CURVE('',#1828,#1850,#633,.T.);
#2438=EDGE_CURVE('',#1850,#1834,#1225,.T.);
#2439=EDGE_CURVE('',#1833,#1851,#1226,.T.);
#2440=EDGE_CURVE('',#1848,#1833,#1227,.T.);
#2441=EDGE_CURVE('',#1846,#1838,#1228,.T.);
#2442=EDGE_CURVE('',#1840,#1845,#1229,.T.);
#2443=EDGE_CURVE('',#1836,#1847,#1230,.T.);
#2444=EDGE_CURVE('',#1820,#1850,#1231,.T.);
#2445=EDGE_CURVE('',#1852,#1853,#1232,.T.);
#2446=EDGE_CURVE('',#1853,#1854,#324,.T.);
#2447=EDGE_CURVE('',#1855,#1854,#634,.T.);
#2448=EDGE_CURVE('',#1852,#1855,#325,.T.);
#2449=EDGE_CURVE('',#1856,#1857,#1233,.T.);
#2450=EDGE_CURVE('',#1857,#1858,#326,.T.);
#2451=EDGE_CURVE('',#1858,#1853,#327,.T.);
#2452=EDGE_CURVE('',#1859,#1852,#328,.T.);
#2453=EDGE_CURVE('',#1856,#1859,#329,.T.);
#2454=EDGE_CURVE('',#1860,#1861,#1234,.T.);
#2455=EDGE_CURVE('',#1861,#1862,#330,.T.);
#2456=EDGE_CURVE('',#1862,#1857,#331,.T.);
#2457=EDGE_CURVE('',#1863,#1856,#332,.T.);
#2458=EDGE_CURVE('',#1860,#1863,#333,.T.);
#2459=EDGE_CURVE('',#1864,#1865,#1235,.T.);
#2460=EDGE_CURVE('',#1865,#1866,#334,.T.);
#2461=EDGE_CURVE('',#1866,#1861,#335,.T.);
#2462=EDGE_CURVE('',#1867,#1860,#336,.T.);
#2463=EDGE_CURVE('',#1864,#1867,#337,.T.);
#2464=EDGE_CURVE('',#1868,#1869,#1236,.T.);
#2465=EDGE_CURVE('',#1869,#1870,#338,.T.);
#2466=EDGE_CURVE('',#1870,#1865,#339,.T.);
#2467=EDGE_CURVE('',#1871,#1864,#340,.T.);
#2468=EDGE_CURVE('',#1868,#1871,#341,.T.);
#2469=EDGE_CURVE('',#1872,#1873,#1237,.T.);
#2470=EDGE_CURVE('',#1873,#1874,#342,.T.);
#2471=EDGE_CURVE('',#1874,#1869,#343,.T.);
#2472=EDGE_CURVE('',#1875,#1868,#344,.T.);
#2473=EDGE_CURVE('',#1872,#1875,#345,.T.);
#2474=EDGE_CURVE('',#1876,#1877,#1238,.T.);
#2475=EDGE_CURVE('',#1878,#1876,#346,.T.);
#2476=EDGE_CURVE('',#1879,#1878,#347,.T.);
#2477=EDGE_CURVE('',#1880,#1879,#635,.T.);
#2478=EDGE_CURVE('',#1880,#1881,#348,.T.);
#2479=EDGE_CURVE('',#1881,#1877,#349,.T.);
#2480=EDGE_CURVE('',#1882,#1883,#1239,.T.);
#2481=EDGE_CURVE('',#1883,#1884,#350,.T.);
#2482=EDGE_CURVE('',#1885,#1884,#636,.F.);
#2483=EDGE_CURVE('',#1885,#1882,#351,.T.);
#2484=EDGE_CURVE('',#1886,#1887,#1240,.T.);
#2485=EDGE_CURVE('',#1887,#1888,#352,.T.);
#2486=EDGE_CURVE('',#1888,#1883,#353,.T.);
#2487=EDGE_CURVE('',#1882,#1886,#354,.T.);
#2488=EDGE_CURVE('',#1889,#1890,#1241,.T.);
#2489=EDGE_CURVE('',#1890,#1891,#355,.T.);
#2490=EDGE_CURVE('',#1891,#1887,#356,.T.);
#2491=EDGE_CURVE('',#1886,#1889,#357,.T.);
#2492=EDGE_CURVE('',#1892,#1893,#1242,.T.);
#2493=EDGE_CURVE('',#1893,#1890,#358,.T.);
#2494=EDGE_CURVE('',#1889,#1892,#359,.T.);
#2495=EDGE_CURVE('',#1894,#1895,#1243,.T.);
#2496=EDGE_CURVE('',#1895,#1896,#360,.T.);
#2497=EDGE_CURVE('',#1896,#1893,#361,.T.);
#2498=EDGE_CURVE('',#1892,#1894,#362,.T.);
#2499=EDGE_CURVE('',#1897,#1898,#1244,.T.);
#2500=EDGE_CURVE('',#1898,#1895,#363,.T.);
#2501=EDGE_CURVE('',#1894,#1897,#364,.T.);
#2502=EDGE_CURVE('',#1899,#1900,#1245,.T.);
#2503=EDGE_CURVE('',#1899,#1901,#365,.T.);
#2504=EDGE_CURVE('',#1901,#1902,#637,.F.);
#2505=EDGE_CURVE('',#1902,#1900,#366,.T.);
#2506=EDGE_CURVE('',#1900,#1903,#367,.T.);
#2507=EDGE_CURVE('',#1903,#1898,#368,.T.);
#2508=EDGE_CURVE('',#1897,#1899,#369,.T.);
#2509=EDGE_CURVE('',#1877,#1904,#370,.T.);
#2510=EDGE_CURVE('',#1904,#1873,#371,.T.);
#2511=EDGE_CURVE('',#1905,#1872,#372,.T.);
#2512=EDGE_CURVE('',#1876,#1905,#373,.T.);
#2513=EDGE_CURVE('',#1854,#1906,#374,.T.);
#2514=EDGE_CURVE('',#1901,#1880,#375,.T.);
#2515=EDGE_CURVE('',#1906,#1885,#376,.T.);
#2516=EDGE_CURVE('',#1884,#1855,#377,.T.);
#2517=EDGE_CURVE('',#1879,#1902,#378,.T.);
#2518=EDGE_CURVE('',#1907,#1908,#1246,.T.);
#2519=EDGE_CURVE('',#1908,#1909,#1247,.T.);
#2520=EDGE_CURVE('',#1909,#1910,#1248,.T.);
#2521=EDGE_CURVE('',#1910,#1911,#1249,.T.);
#2522=EDGE_CURVE('',#1911,#1912,#1250,.T.);
#2523=EDGE_CURVE('',#1912,#1907,#1251,.T.);
#2524=EDGE_CURVE('',#1913,#1914,#1252,.T.);
#2525=EDGE_CURVE('',#1914,#1907,#1253,.T.);
#2526=EDGE_CURVE('',#1913,#1912,#1254,.T.);
#2527=EDGE_CURVE('',#1915,#1913,#1255,.T.);
#2528=EDGE_CURVE('',#1915,#1911,#1256,.T.);
#2529=EDGE_CURVE('',#1916,#1915,#1257,.T.);
#2530=EDGE_CURVE('',#1916,#1910,#1258,.T.);
#2531=EDGE_CURVE('',#1917,#1916,#1259,.T.);
#2532=EDGE_CURVE('',#1917,#1909,#1260,.T.);
#2533=EDGE_CURVE('',#1918,#1917,#1261,.T.);
#2534=EDGE_CURVE('',#1918,#1908,#1262,.T.);
#2535=EDGE_CURVE('',#1914,#1918,#1263,.T.);
#2536=ORIENTED_EDGE('',*,*,#1919,.F.);
#2537=ORIENTED_EDGE('',*,*,#1920,.F.);
#2538=ORIENTED_EDGE('',*,*,#1921,.T.);
#2539=ORIENTED_EDGE('',*,*,#1922,.T.);
#2540=ORIENTED_EDGE('',*,*,#1923,.T.);
#2541=ORIENTED_EDGE('',*,*,#1924,.F.);
#2542=ORIENTED_EDGE('',*,*,#1925,.F.);
#2543=ORIENTED_EDGE('',*,*,#1926,.T.);
#2544=ORIENTED_EDGE('',*,*,#1927,.T.);
#2545=ORIENTED_EDGE('',*,*,#1920,.T.);
#2546=ORIENTED_EDGE('',*,*,#1928,.F.);
#2547=ORIENTED_EDGE('',*,*,#1923,.F.);
#2548=ORIENTED_EDGE('',*,*,#1929,.T.);
#2549=ORIENTED_EDGE('',*,*,#1930,.T.);
#2550=ORIENTED_EDGE('',*,*,#1931,.T.);
#2551=ORIENTED_EDGE('',*,*,#1932,.F.);
#2552=ORIENTED_EDGE('',*,*,#1933,.F.);
#2553=ORIENTED_EDGE('',*,*,#1934,.T.);
#2554=ORIENTED_EDGE('',*,*,#1935,.T.);
#2555=ORIENTED_EDGE('',*,*,#1925,.T.);
#2556=ORIENTED_EDGE('',*,*,#1936,.F.);
#2557=ORIENTED_EDGE('',*,*,#1937,.F.);
#2558=ORIENTED_EDGE('',*,*,#1938,.F.);
#2559=ORIENTED_EDGE('',*,*,#1939,.F.);
#2560=ORIENTED_EDGE('',*,*,#1940,.F.);
#2561=ORIENTED_EDGE('',*,*,#1930,.F.);
#2562=ORIENTED_EDGE('',*,*,#1941,.F.);
#2563=ORIENTED_EDGE('',*,*,#1929,.F.);
#2564=ORIENTED_EDGE('',*,*,#1922,.F.);
#2565=ORIENTED_EDGE('',*,*,#1942,.F.);
#2566=ORIENTED_EDGE('',*,*,#1921,.F.);
#2567=ORIENTED_EDGE('',*,*,#1927,.F.);
#2568=ORIENTED_EDGE('',*,*,#1943,.F.);
#2569=ORIENTED_EDGE('',*,*,#1926,.F.);
#2570=ORIENTED_EDGE('',*,*,#1935,.F.);
#2571=ORIENTED_EDGE('',*,*,#1944,.F.);
#2572=ORIENTED_EDGE('',*,*,#1934,.F.);
#2573=ORIENTED_EDGE('',*,*,#1945,.F.);
#2574=ORIENTED_EDGE('',*,*,#1946,.F.);
#2575=ORIENTED_EDGE('',*,*,#1947,.F.);
#2576=ORIENTED_EDGE('',*,*,#1931,.F.);
#2577=ORIENTED_EDGE('',*,*,#1940,.T.);
#2578=ORIENTED_EDGE('',*,*,#1938,.T.);
#2579=ORIENTED_EDGE('',*,*,#1948,.F.);
#2580=ORIENTED_EDGE('',*,*,#1949,.F.);
#2581=ORIENTED_EDGE('',*,*,#1948,.T.);
#2582=ORIENTED_EDGE('',*,*,#1937,.T.);
#2583=ORIENTED_EDGE('',*,*,#1945,.T.);
#2584=ORIENTED_EDGE('',*,*,#1933,.T.);
#2585=ORIENTED_EDGE('',*,*,#1950,.T.);
#2586=ORIENTED_EDGE('',*,*,#1951,.T.);
#2587=ORIENTED_EDGE('',*,*,#1952,.T.);
#2588=ORIENTED_EDGE('',*,*,#1951,.F.);
#2589=ORIENTED_EDGE('',*,*,#1952,.F.);
#2590=ORIENTED_EDGE('',*,*,#1953,.T.);
#2591=ORIENTED_EDGE('',*,*,#1954,.F.);
#2592=ORIENTED_EDGE('',*,*,#1953,.F.);
#2593=ORIENTED_EDGE('',*,*,#1950,.F.);
#2594=ORIENTED_EDGE('',*,*,#1949,.T.);
#2595=ORIENTED_EDGE('',*,*,#1932,.T.);
#2596=ORIENTED_EDGE('',*,*,#1924,.T.);
#2597=ORIENTED_EDGE('',*,*,#1919,.T.);
#2598=ORIENTED_EDGE('',*,*,#1928,.T.);
#2599=ORIENTED_EDGE('',*,*,#1947,.T.);
#2600=ORIENTED_EDGE('',*,*,#1954,.T.);
#2601=ORIENTED_EDGE('',*,*,#1955,.T.);
#2602=ORIENTED_EDGE('',*,*,#1956,.T.);
#2603=ORIENTED_EDGE('',*,*,#1955,.F.);
#2604=ORIENTED_EDGE('',*,*,#1956,.F.);
#2605=ORIENTED_EDGE('',*,*,#1957,.F.);
#2606=ORIENTED_EDGE('',*,*,#1958,.T.);
#2607=ORIENTED_EDGE('',*,*,#1959,.T.);
#2608=ORIENTED_EDGE('',*,*,#1957,.T.);
#2609=ORIENTED_EDGE('',*,*,#1959,.F.);
#2610=ORIENTED_EDGE('',*,*,#1960,.T.);
#2611=ORIENTED_EDGE('',*,*,#1958,.F.);
#2612=ORIENTED_EDGE('',*,*,#1961,.T.);
#2613=ORIENTED_EDGE('',*,*,#1962,.F.);
#2614=ORIENTED_EDGE('',*,*,#1963,.F.);
#2615=ORIENTED_EDGE('',*,*,#1961,.F.);
#2616=ORIENTED_EDGE('',*,*,#1960,.F.);
#2617=ORIENTED_EDGE('',*,*,#1964,.T.);
#2618=ORIENTED_EDGE('',*,*,#1962,.T.);
#2619=ORIENTED_EDGE('',*,*,#1963,.T.);
#2620=ORIENTED_EDGE('',*,*,#1964,.F.);
#2621=ORIENTED_EDGE('',*,*,#1965,.T.);
#2622=ORIENTED_EDGE('',*,*,#1966,.F.);
#2623=ORIENTED_EDGE('',*,*,#1967,.T.);
#2624=ORIENTED_EDGE('',*,*,#1968,.F.);
#2625=ORIENTED_EDGE('',*,*,#1967,.F.);
#2626=ORIENTED_EDGE('',*,*,#1965,.F.);
#2627=ORIENTED_EDGE('',*,*,#1969,.F.);
#2628=ORIENTED_EDGE('',*,*,#1970,.F.);
#2629=ORIENTED_EDGE('',*,*,#1971,.T.);
#2630=ORIENTED_EDGE('',*,*,#1946,.T.);
#2631=ORIENTED_EDGE('',*,*,#1936,.T.);
#2632=ORIENTED_EDGE('',*,*,#1939,.T.);
#2633=ORIENTED_EDGE('',*,*,#1941,.T.);
#2634=ORIENTED_EDGE('',*,*,#1942,.T.);
#2635=ORIENTED_EDGE('',*,*,#1943,.T.);
#2636=ORIENTED_EDGE('',*,*,#1944,.T.);
#2637=ORIENTED_EDGE('',*,*,#1971,.F.);
#2638=ORIENTED_EDGE('',*,*,#1972,.F.);
#2639=ORIENTED_EDGE('',*,*,#1973,.T.);
#2640=ORIENTED_EDGE('',*,*,#1974,.T.);
#2641=ORIENTED_EDGE('',*,*,#1973,.F.);
#2642=ORIENTED_EDGE('',*,*,#1974,.F.);
#2643=ORIENTED_EDGE('',*,*,#1975,.F.);
#2644=ORIENTED_EDGE('',*,*,#1976,.F.);
#2645=ORIENTED_EDGE('',*,*,#1977,.T.);
#2646=ORIENTED_EDGE('',*,*,#1978,.F.);
#2647=ORIENTED_EDGE('',*,*,#1977,.F.);
#2648=ORIENTED_EDGE('',*,*,#1976,.T.);
#2649=ORIENTED_EDGE('',*,*,#1979,.T.);
#2650=ORIENTED_EDGE('',*,*,#1979,.F.);
#2651=ORIENTED_EDGE('',*,*,#1980,.T.);
#2652=ORIENTED_EDGE('',*,*,#1975,.T.);
#2653=ORIENTED_EDGE('',*,*,#1980,.F.);
#2654=ORIENTED_EDGE('',*,*,#1969,.T.);
#2655=ORIENTED_EDGE('',*,*,#1970,.T.);
#2656=ORIENTED_EDGE('',*,*,#1968,.T.);
#2657=ORIENTED_EDGE('',*,*,#1978,.T.);
#2658=ORIENTED_EDGE('',*,*,#1966,.T.);
#2659=ORIENTED_EDGE('',*,*,#1972,.T.);
#2660=ORIENTED_EDGE('',*,*,#1981,.T.);
#2661=ORIENTED_EDGE('',*,*,#1982,.T.);
#2662=ORIENTED_EDGE('',*,*,#1983,.T.);
#2663=ORIENTED_EDGE('',*,*,#1984,.T.);
#2664=ORIENTED_EDGE('',*,*,#1985,.T.);
#2665=ORIENTED_EDGE('',*,*,#1986,.T.);
#2666=ORIENTED_EDGE('',*,*,#1983,.F.);
#2667=ORIENTED_EDGE('',*,*,#1987,.T.);
#2668=ORIENTED_EDGE('',*,*,#1988,.T.);
#2669=ORIENTED_EDGE('',*,*,#1989,.T.);
#2670=ORIENTED_EDGE('',*,*,#1985,.F.);
#2671=ORIENTED_EDGE('',*,*,#1990,.T.);
#2672=ORIENTED_EDGE('',*,*,#1984,.F.);
#2673=ORIENTED_EDGE('',*,*,#1991,.T.);
#2674=ORIENTED_EDGE('',*,*,#1992,.F.);
#2675=ORIENTED_EDGE('',*,*,#1993,.F.);
#2676=ORIENTED_EDGE('',*,*,#1986,.F.);
#2677=ORIENTED_EDGE('',*,*,#1994,.T.);
#2678=ORIENTED_EDGE('',*,*,#1995,.F.);
#2679=ORIENTED_EDGE('',*,*,#1991,.F.);
#2680=ORIENTED_EDGE('',*,*,#1989,.F.);
#2681=ORIENTED_EDGE('',*,*,#1996,.T.);
#2682=ORIENTED_EDGE('',*,*,#1997,.F.);
#2683=ORIENTED_EDGE('',*,*,#1994,.F.);
#2684=ORIENTED_EDGE('',*,*,#1998,.T.);
#2685=ORIENTED_EDGE('',*,*,#1999,.T.);
#2686=ORIENTED_EDGE('',*,*,#2000,.T.);
#2687=ORIENTED_EDGE('',*,*,#1997,.T.);
#2688=ORIENTED_EDGE('',*,*,#2001,.T.);
#2689=ORIENTED_EDGE('',*,*,#1995,.T.);
#2690=ORIENTED_EDGE('',*,*,#2000,.F.);
#2691=ORIENTED_EDGE('',*,*,#2002,.T.);
#2692=ORIENTED_EDGE('',*,*,#2003,.T.);
#2693=ORIENTED_EDGE('',*,*,#1992,.T.);
#2694=ORIENTED_EDGE('',*,*,#2001,.F.);
#2695=ORIENTED_EDGE('',*,*,#2004,.T.);
#2696=ORIENTED_EDGE('',*,*,#2004,.F.);
#2697=ORIENTED_EDGE('',*,*,#2002,.F.);
#2698=ORIENTED_EDGE('',*,*,#1999,.F.);
#2699=ORIENTED_EDGE('',*,*,#2005,.F.);
#2700=ORIENTED_EDGE('',*,*,#1981,.F.);
#2701=ORIENTED_EDGE('',*,*,#1993,.T.);
#2702=ORIENTED_EDGE('',*,*,#2003,.F.);
#2703=ORIENTED_EDGE('',*,*,#2005,.T.);
#2704=ORIENTED_EDGE('',*,*,#1998,.F.);
#2705=ORIENTED_EDGE('',*,*,#1996,.F.);
#2706=ORIENTED_EDGE('',*,*,#1988,.F.);
#2707=ORIENTED_EDGE('',*,*,#2006,.F.);
#2708=ORIENTED_EDGE('',*,*,#2007,.T.);
#2709=ORIENTED_EDGE('',*,*,#2008,.F.);
#2710=ORIENTED_EDGE('',*,*,#2009,.F.);
#2711=ORIENTED_EDGE('',*,*,#2010,.T.);
#2712=ORIENTED_EDGE('',*,*,#2011,.T.);
#2713=ORIENTED_EDGE('',*,*,#2012,.T.);
#2714=ORIENTED_EDGE('',*,*,#2013,.T.);
#2715=ORIENTED_EDGE('',*,*,#2014,.F.);
#2716=ORIENTED_EDGE('',*,*,#2014,.T.);
#2717=ORIENTED_EDGE('',*,*,#2015,.T.);
#2718=ORIENTED_EDGE('',*,*,#2010,.F.);
#2719=ORIENTED_EDGE('',*,*,#2016,.T.);
#2720=ORIENTED_EDGE('',*,*,#2017,.F.);
#2721=ORIENTED_EDGE('',*,*,#2018,.T.);
#2722=ORIENTED_EDGE('',*,*,#2019,.F.);
#2723=ORIENTED_EDGE('',*,*,#2012,.F.);
#2724=ORIENTED_EDGE('',*,*,#2017,.T.);
#2725=ORIENTED_EDGE('',*,*,#2011,.F.);
#2726=ORIENTED_EDGE('',*,*,#2016,.F.);
#2727=ORIENTED_EDGE('',*,*,#2009,.T.);
#2728=ORIENTED_EDGE('',*,*,#2020,.T.);
#2729=ORIENTED_EDGE('',*,*,#2018,.F.);
#2730=ORIENTED_EDGE('',*,*,#2020,.F.);
#2731=ORIENTED_EDGE('',*,*,#2008,.T.);
#2732=ORIENTED_EDGE('',*,*,#2021,.F.);
#2733=ORIENTED_EDGE('',*,*,#2019,.T.);
#2734=ORIENTED_EDGE('',*,*,#2021,.T.);
#2735=ORIENTED_EDGE('',*,*,#2007,.F.);
#2736=ORIENTED_EDGE('',*,*,#2015,.F.);
#2737=ORIENTED_EDGE('',*,*,#2013,.F.);
#2738=ORIENTED_EDGE('',*,*,#1982,.F.);
#2739=ORIENTED_EDGE('',*,*,#2006,.T.);
#2740=ORIENTED_EDGE('',*,*,#1990,.F.);
#2741=ORIENTED_EDGE('',*,*,#1987,.F.);
#2742=ORIENTED_EDGE('',*,*,#2022,.F.);
#2743=ORIENTED_EDGE('',*,*,#2022,.T.);
#2744=ORIENTED_EDGE('',*,*,#2023,.F.);
#2745=ORIENTED_EDGE('',*,*,#2024,.F.);
#2746=ORIENTED_EDGE('',*,*,#2025,.T.);
#2747=ORIENTED_EDGE('',*,*,#2026,.F.);
#2748=ORIENTED_EDGE('',*,*,#2027,.F.);
#2749=ORIENTED_EDGE('',*,*,#2028,.F.);
#2750=ORIENTED_EDGE('',*,*,#2023,.T.);
#2751=ORIENTED_EDGE('',*,*,#2029,.T.);
#2752=ORIENTED_EDGE('',*,*,#2030,.T.);
#2753=ORIENTED_EDGE('',*,*,#2031,.T.);
#2754=ORIENTED_EDGE('',*,*,#2032,.F.);
#2755=ORIENTED_EDGE('',*,*,#2033,.F.);
#2756=ORIENTED_EDGE('',*,*,#2034,.F.);
#2757=ORIENTED_EDGE('',*,*,#2026,.T.);
#2758=ORIENTED_EDGE('',*,*,#2035,.T.);
#2759=ORIENTED_EDGE('',*,*,#2036,.T.);
#2760=ORIENTED_EDGE('',*,*,#2037,.F.);
#2761=ORIENTED_EDGE('',*,*,#2038,.F.);
#2762=ORIENTED_EDGE('',*,*,#2039,.F.);
#2763=ORIENTED_EDGE('',*,*,#2032,.T.);
#2764=ORIENTED_EDGE('',*,*,#2040,.T.);
#2765=ORIENTED_EDGE('',*,*,#2041,.T.);
#2766=ORIENTED_EDGE('',*,*,#2042,.F.);
#2767=ORIENTED_EDGE('',*,*,#2043,.F.);
#2768=ORIENTED_EDGE('',*,*,#2044,.F.);
#2769=ORIENTED_EDGE('',*,*,#2037,.T.);
#2770=ORIENTED_EDGE('',*,*,#2045,.T.);
#2771=ORIENTED_EDGE('',*,*,#2046,.T.);
#2772=ORIENTED_EDGE('',*,*,#2047,.F.);
#2773=ORIENTED_EDGE('',*,*,#2048,.F.);
#2774=ORIENTED_EDGE('',*,*,#2049,.F.);
#2775=ORIENTED_EDGE('',*,*,#2042,.T.);
#2776=ORIENTED_EDGE('',*,*,#2050,.T.);
#2777=ORIENTED_EDGE('',*,*,#2051,.T.);
#2778=ORIENTED_EDGE('',*,*,#2052,.F.);
#2779=ORIENTED_EDGE('',*,*,#2053,.F.);
#2780=ORIENTED_EDGE('',*,*,#2054,.F.);
#2781=ORIENTED_EDGE('',*,*,#2047,.T.);
#2782=ORIENTED_EDGE('',*,*,#2055,.T.);
#2783=ORIENTED_EDGE('',*,*,#2056,.T.);
#2784=ORIENTED_EDGE('',*,*,#2057,.F.);
#2785=ORIENTED_EDGE('',*,*,#2058,.F.);
#2786=ORIENTED_EDGE('',*,*,#2059,.F.);
#2787=ORIENTED_EDGE('',*,*,#2060,.F.);
#2788=ORIENTED_EDGE('',*,*,#2061,.F.);
#2789=ORIENTED_EDGE('',*,*,#2062,.F.);
#2790=ORIENTED_EDGE('',*,*,#2063,.F.);
#2791=ORIENTED_EDGE('',*,*,#2064,.F.);
#2792=ORIENTED_EDGE('',*,*,#2057,.T.);
#2793=ORIENTED_EDGE('',*,*,#2065,.F.);
#2794=ORIENTED_EDGE('',*,*,#2066,.F.);
#2795=ORIENTED_EDGE('',*,*,#2067,.F.);
#2796=ORIENTED_EDGE('',*,*,#2062,.T.);
#2797=ORIENTED_EDGE('',*,*,#2068,.F.);
#2798=ORIENTED_EDGE('',*,*,#2069,.F.);
#2799=ORIENTED_EDGE('',*,*,#2070,.F.);
#2800=ORIENTED_EDGE('',*,*,#2071,.F.);
#2801=ORIENTED_EDGE('',*,*,#2066,.T.);
#2802=ORIENTED_EDGE('',*,*,#2072,.F.);
#2803=ORIENTED_EDGE('',*,*,#2073,.F.);
#2804=ORIENTED_EDGE('',*,*,#2074,.F.);
#2805=ORIENTED_EDGE('',*,*,#2069,.T.);
#2806=ORIENTED_EDGE('',*,*,#2075,.F.);
#2807=ORIENTED_EDGE('',*,*,#2076,.F.);
#2808=ORIENTED_EDGE('',*,*,#2077,.F.);
#2809=ORIENTED_EDGE('',*,*,#2078,.F.);
#2810=ORIENTED_EDGE('',*,*,#2073,.T.);
#2811=ORIENTED_EDGE('',*,*,#2079,.F.);
#2812=ORIENTED_EDGE('',*,*,#2076,.T.);
#2813=ORIENTED_EDGE('',*,*,#2080,.F.);
#2814=ORIENTED_EDGE('',*,*,#2081,.T.);
#2815=ORIENTED_EDGE('',*,*,#2082,.F.);
#2816=ORIENTED_EDGE('',*,*,#2052,.T.);
#2817=ORIENTED_EDGE('',*,*,#2083,.T.);
#2818=ORIENTED_EDGE('',*,*,#2084,.T.);
#2819=ORIENTED_EDGE('',*,*,#2085,.T.);
#2820=ORIENTED_EDGE('',*,*,#2086,.F.);
#2821=ORIENTED_EDGE('',*,*,#2087,.F.);
#2822=ORIENTED_EDGE('',*,*,#2088,.T.);
#2823=ORIENTED_EDGE('',*,*,#2089,.T.);
#2824=ORIENTED_EDGE('',*,*,#2080,.T.);
#2825=ORIENTED_EDGE('',*,*,#2079,.T.);
#2826=ORIENTED_EDGE('',*,*,#2075,.T.);
#2827=ORIENTED_EDGE('',*,*,#2072,.T.);
#2828=ORIENTED_EDGE('',*,*,#2068,.T.);
#2829=ORIENTED_EDGE('',*,*,#2065,.T.);
#2830=ORIENTED_EDGE('',*,*,#2061,.T.);
#2831=ORIENTED_EDGE('',*,*,#2090,.T.);
#2832=ORIENTED_EDGE('',*,*,#2024,.T.);
#2833=ORIENTED_EDGE('',*,*,#2028,.T.);
#2834=ORIENTED_EDGE('',*,*,#2027,.T.);
#2835=ORIENTED_EDGE('',*,*,#2034,.T.);
#2836=ORIENTED_EDGE('',*,*,#2033,.T.);
#2837=ORIENTED_EDGE('',*,*,#2039,.T.);
#2838=ORIENTED_EDGE('',*,*,#2038,.T.);
#2839=ORIENTED_EDGE('',*,*,#2044,.T.);
#2840=ORIENTED_EDGE('',*,*,#2043,.T.);
#2841=ORIENTED_EDGE('',*,*,#2049,.T.);
#2842=ORIENTED_EDGE('',*,*,#2048,.T.);
#2843=ORIENTED_EDGE('',*,*,#2054,.T.);
#2844=ORIENTED_EDGE('',*,*,#2053,.T.);
#2845=ORIENTED_EDGE('',*,*,#2087,.T.);
#2846=ORIENTED_EDGE('',*,*,#2086,.T.);
#2847=ORIENTED_EDGE('',*,*,#2091,.T.);
#2848=ORIENTED_EDGE('',*,*,#2084,.F.);
#2849=ORIENTED_EDGE('',*,*,#2083,.F.);
#2850=ORIENTED_EDGE('',*,*,#2056,.F.);
#2851=ORIENTED_EDGE('',*,*,#2055,.F.);
#2852=ORIENTED_EDGE('',*,*,#2051,.F.);
#2853=ORIENTED_EDGE('',*,*,#2050,.F.);
#2854=ORIENTED_EDGE('',*,*,#2046,.F.);
#2855=ORIENTED_EDGE('',*,*,#2045,.F.);
#2856=ORIENTED_EDGE('',*,*,#2041,.F.);
#2857=ORIENTED_EDGE('',*,*,#2040,.F.);
#2858=ORIENTED_EDGE('',*,*,#2036,.F.);
#2859=ORIENTED_EDGE('',*,*,#2035,.F.);
#2860=ORIENTED_EDGE('',*,*,#2031,.F.);
#2861=ORIENTED_EDGE('',*,*,#2030,.F.);
#2862=ORIENTED_EDGE('',*,*,#2092,.T.);
#2863=ORIENTED_EDGE('',*,*,#2059,.T.);
#2864=ORIENTED_EDGE('',*,*,#2058,.T.);
#2865=ORIENTED_EDGE('',*,*,#2064,.T.);
#2866=ORIENTED_EDGE('',*,*,#2063,.T.);
#2867=ORIENTED_EDGE('',*,*,#2067,.T.);
#2868=ORIENTED_EDGE('',*,*,#2071,.T.);
#2869=ORIENTED_EDGE('',*,*,#2070,.T.);
#2870=ORIENTED_EDGE('',*,*,#2074,.T.);
#2871=ORIENTED_EDGE('',*,*,#2078,.T.);
#2872=ORIENTED_EDGE('',*,*,#2077,.T.);
#2873=ORIENTED_EDGE('',*,*,#2082,.T.);
#2874=ORIENTED_EDGE('',*,*,#2093,.F.);
#2875=ORIENTED_EDGE('',*,*,#2094,.F.);
#2876=ORIENTED_EDGE('',*,*,#2095,.F.);
#2877=ORIENTED_EDGE('',*,*,#2096,.F.);
#2878=ORIENTED_EDGE('',*,*,#2097,.F.);
#2879=ORIENTED_EDGE('',*,*,#2098,.F.);
#2880=ORIENTED_EDGE('',*,*,#2091,.F.);
#2881=ORIENTED_EDGE('',*,*,#2081,.F.);
#2882=ORIENTED_EDGE('',*,*,#2089,.F.);
#2883=ORIENTED_EDGE('',*,*,#2088,.F.);
#2884=ORIENTED_EDGE('',*,*,#2085,.F.);
#2885=ORIENTED_EDGE('',*,*,#2099,.F.);
#2886=ORIENTED_EDGE('',*,*,#2100,.T.);
#2887=ORIENTED_EDGE('',*,*,#2094,.T.);
#2888=ORIENTED_EDGE('',*,*,#2101,.F.);
#2889=ORIENTED_EDGE('',*,*,#2102,.F.);
#2890=ORIENTED_EDGE('',*,*,#2103,.T.);
#2891=ORIENTED_EDGE('',*,*,#2095,.T.);
#2892=ORIENTED_EDGE('',*,*,#2100,.F.);
#2893=ORIENTED_EDGE('',*,*,#2104,.F.);
#2894=ORIENTED_EDGE('',*,*,#2105,.T.);
#2895=ORIENTED_EDGE('',*,*,#2096,.T.);
#2896=ORIENTED_EDGE('',*,*,#2103,.F.);
#2897=ORIENTED_EDGE('',*,*,#2106,.F.);
#2898=ORIENTED_EDGE('',*,*,#2107,.T.);
#2899=ORIENTED_EDGE('',*,*,#2097,.T.);
#2900=ORIENTED_EDGE('',*,*,#2105,.F.);
#2901=ORIENTED_EDGE('',*,*,#2108,.F.);
#2902=ORIENTED_EDGE('',*,*,#2109,.T.);
#2903=ORIENTED_EDGE('',*,*,#2098,.T.);
#2904=ORIENTED_EDGE('',*,*,#2107,.F.);
#2905=ORIENTED_EDGE('',*,*,#2110,.F.);
#2906=ORIENTED_EDGE('',*,*,#2101,.T.);
#2907=ORIENTED_EDGE('',*,*,#2093,.T.);
#2908=ORIENTED_EDGE('',*,*,#2109,.F.);
#2909=ORIENTED_EDGE('',*,*,#2110,.T.);
#2910=ORIENTED_EDGE('',*,*,#2108,.T.);
#2911=ORIENTED_EDGE('',*,*,#2106,.T.);
#2912=ORIENTED_EDGE('',*,*,#2104,.T.);
#2913=ORIENTED_EDGE('',*,*,#2102,.T.);
#2914=ORIENTED_EDGE('',*,*,#2099,.T.);
#2915=ORIENTED_EDGE('',*,*,#2092,.F.);
#2916=ORIENTED_EDGE('',*,*,#2029,.F.);
#2917=ORIENTED_EDGE('',*,*,#2025,.F.);
#2918=ORIENTED_EDGE('',*,*,#2090,.F.);
#2919=ORIENTED_EDGE('',*,*,#2060,.T.);
#2920=ORIENTED_EDGE('',*,*,#2111,.F.);
#2921=ORIENTED_EDGE('',*,*,#2112,.F.);
#2922=ORIENTED_EDGE('',*,*,#2113,.F.);
#2923=ORIENTED_EDGE('',*,*,#2114,.T.);
#2924=ORIENTED_EDGE('',*,*,#2115,.F.);
#2925=ORIENTED_EDGE('',*,*,#2116,.F.);
#2926=ORIENTED_EDGE('',*,*,#2117,.F.);
#2927=ORIENTED_EDGE('',*,*,#2111,.T.);
#2928=ORIENTED_EDGE('',*,*,#2118,.T.);
#2929=ORIENTED_EDGE('',*,*,#2119,.T.);
#2930=ORIENTED_EDGE('',*,*,#2120,.F.);
#2931=ORIENTED_EDGE('',*,*,#2121,.F.);
#2932=ORIENTED_EDGE('',*,*,#2115,.T.);
#2933=ORIENTED_EDGE('',*,*,#2122,.T.);
#2934=ORIENTED_EDGE('',*,*,#2123,.F.);
#2935=ORIENTED_EDGE('',*,*,#2124,.F.);
#2936=ORIENTED_EDGE('',*,*,#2125,.F.);
#2937=ORIENTED_EDGE('',*,*,#2120,.T.);
#2938=ORIENTED_EDGE('',*,*,#2126,.T.);
#2939=ORIENTED_EDGE('',*,*,#2127,.T.);
#2940=ORIENTED_EDGE('',*,*,#2128,.F.);
#2941=ORIENTED_EDGE('',*,*,#2129,.F.);
#2942=ORIENTED_EDGE('',*,*,#2123,.T.);
#2943=ORIENTED_EDGE('',*,*,#2130,.T.);
#2944=ORIENTED_EDGE('',*,*,#2131,.T.);
#2945=ORIENTED_EDGE('',*,*,#2132,.F.);
#2946=ORIENTED_EDGE('',*,*,#2133,.F.);
#2947=ORIENTED_EDGE('',*,*,#2134,.F.);
#2948=ORIENTED_EDGE('',*,*,#2128,.T.);
#2949=ORIENTED_EDGE('',*,*,#2135,.T.);
#2950=ORIENTED_EDGE('',*,*,#2136,.F.);
#2951=ORIENTED_EDGE('',*,*,#2137,.F.);
#2952=ORIENTED_EDGE('',*,*,#2132,.T.);
#2953=ORIENTED_EDGE('',*,*,#2138,.T.);
#2954=ORIENTED_EDGE('',*,*,#2139,.T.);
#2955=ORIENTED_EDGE('',*,*,#2140,.F.);
#2956=ORIENTED_EDGE('',*,*,#2141,.F.);
#2957=ORIENTED_EDGE('',*,*,#2142,.F.);
#2958=ORIENTED_EDGE('',*,*,#2136,.T.);
#2959=ORIENTED_EDGE('',*,*,#2143,.T.);
#2960=ORIENTED_EDGE('',*,*,#2144,.F.);
#2961=ORIENTED_EDGE('',*,*,#2145,.F.);
#2962=ORIENTED_EDGE('',*,*,#2140,.T.);
#2963=ORIENTED_EDGE('',*,*,#2146,.T.);
#2964=ORIENTED_EDGE('',*,*,#2147,.T.);
#2965=ORIENTED_EDGE('',*,*,#2148,.F.);
#2966=ORIENTED_EDGE('',*,*,#2149,.F.);
#2967=ORIENTED_EDGE('',*,*,#2150,.F.);
#2968=ORIENTED_EDGE('',*,*,#2144,.T.);
#2969=ORIENTED_EDGE('',*,*,#2151,.T.);
#2970=ORIENTED_EDGE('',*,*,#2152,.F.);
#2971=ORIENTED_EDGE('',*,*,#2153,.F.);
#2972=ORIENTED_EDGE('',*,*,#2148,.T.);
#2973=ORIENTED_EDGE('',*,*,#2154,.T.);
#2974=ORIENTED_EDGE('',*,*,#2155,.T.);
#2975=ORIENTED_EDGE('',*,*,#2156,.F.);
#2976=ORIENTED_EDGE('',*,*,#2157,.F.);
#2977=ORIENTED_EDGE('',*,*,#2158,.F.);
#2978=ORIENTED_EDGE('',*,*,#2152,.T.);
#2979=ORIENTED_EDGE('',*,*,#2159,.T.);
#2980=ORIENTED_EDGE('',*,*,#2160,.F.);
#2981=ORIENTED_EDGE('',*,*,#2161,.F.);
#2982=ORIENTED_EDGE('',*,*,#2162,.F.);
#2983=ORIENTED_EDGE('',*,*,#2156,.T.);
#2984=ORIENTED_EDGE('',*,*,#2163,.T.);
#2985=ORIENTED_EDGE('',*,*,#2164,.T.);
#2986=ORIENTED_EDGE('',*,*,#2165,.F.);
#2987=ORIENTED_EDGE('',*,*,#2166,.F.);
#2988=ORIENTED_EDGE('',*,*,#2160,.T.);
#2989=ORIENTED_EDGE('',*,*,#2167,.T.);
#2990=ORIENTED_EDGE('',*,*,#2168,.F.);
#2991=ORIENTED_EDGE('',*,*,#2169,.F.);
#2992=ORIENTED_EDGE('',*,*,#2170,.F.);
#2993=ORIENTED_EDGE('',*,*,#2165,.T.);
#2994=ORIENTED_EDGE('',*,*,#2171,.T.);
#2995=ORIENTED_EDGE('',*,*,#2172,.T.);
#2996=ORIENTED_EDGE('',*,*,#2173,.F.);
#2997=ORIENTED_EDGE('',*,*,#2174,.F.);
#2998=ORIENTED_EDGE('',*,*,#2168,.T.);
#2999=ORIENTED_EDGE('',*,*,#2175,.T.);
#3000=ORIENTED_EDGE('',*,*,#2176,.F.);
#3001=ORIENTED_EDGE('',*,*,#2177,.F.);
#3002=ORIENTED_EDGE('',*,*,#2178,.F.);
#3003=ORIENTED_EDGE('',*,*,#2173,.T.);
#3004=ORIENTED_EDGE('',*,*,#2179,.T.);
#3005=ORIENTED_EDGE('',*,*,#2180,.T.);
#3006=ORIENTED_EDGE('',*,*,#2181,.F.);
#3007=ORIENTED_EDGE('',*,*,#2182,.F.);
#3008=ORIENTED_EDGE('',*,*,#2176,.T.);
#3009=ORIENTED_EDGE('',*,*,#2183,.T.);
#3010=ORIENTED_EDGE('',*,*,#2184,.T.);
#3011=ORIENTED_EDGE('',*,*,#2185,.F.);
#3012=ORIENTED_EDGE('',*,*,#2186,.F.);
#3013=ORIENTED_EDGE('',*,*,#2187,.F.);
#3014=ORIENTED_EDGE('',*,*,#2181,.T.);
#3015=ORIENTED_EDGE('',*,*,#2188,.T.);
#3016=ORIENTED_EDGE('',*,*,#2189,.F.);
#3017=ORIENTED_EDGE('',*,*,#2190,.F.);
#3018=ORIENTED_EDGE('',*,*,#2185,.T.);
#3019=ORIENTED_EDGE('',*,*,#2191,.T.);
#3020=ORIENTED_EDGE('',*,*,#2192,.T.);
#3021=ORIENTED_EDGE('',*,*,#2193,.F.);
#3022=ORIENTED_EDGE('',*,*,#2194,.F.);
#3023=ORIENTED_EDGE('',*,*,#2195,.F.);
#3024=ORIENTED_EDGE('',*,*,#2189,.T.);
#3025=ORIENTED_EDGE('',*,*,#2196,.T.);
#3026=ORIENTED_EDGE('',*,*,#2197,.F.);
#3027=ORIENTED_EDGE('',*,*,#2198,.F.);
#3028=ORIENTED_EDGE('',*,*,#2193,.T.);
#3029=ORIENTED_EDGE('',*,*,#2199,.T.);
#3030=ORIENTED_EDGE('',*,*,#2200,.T.);
#3031=ORIENTED_EDGE('',*,*,#2201,.F.);
#3032=ORIENTED_EDGE('',*,*,#2202,.F.);
#3033=ORIENTED_EDGE('',*,*,#2203,.F.);
#3034=ORIENTED_EDGE('',*,*,#2197,.T.);
#3035=ORIENTED_EDGE('',*,*,#2204,.T.);
#3036=ORIENTED_EDGE('',*,*,#2205,.F.);
#3037=ORIENTED_EDGE('',*,*,#2206,.F.);
#3038=ORIENTED_EDGE('',*,*,#2201,.T.);
#3039=ORIENTED_EDGE('',*,*,#2207,.T.);
#3040=ORIENTED_EDGE('',*,*,#2208,.T.);
#3041=ORIENTED_EDGE('',*,*,#2209,.F.);
#3042=ORIENTED_EDGE('',*,*,#2210,.F.);
#3043=ORIENTED_EDGE('',*,*,#2211,.F.);
#3044=ORIENTED_EDGE('',*,*,#2205,.T.);
#3045=ORIENTED_EDGE('',*,*,#2212,.T.);
#3046=ORIENTED_EDGE('',*,*,#2213,.F.);
#3047=ORIENTED_EDGE('',*,*,#2214,.F.);
#3048=ORIENTED_EDGE('',*,*,#2215,.F.);
#3049=ORIENTED_EDGE('',*,*,#2209,.T.);
#3050=ORIENTED_EDGE('',*,*,#2216,.T.);
#3051=ORIENTED_EDGE('',*,*,#2217,.T.);
#3052=ORIENTED_EDGE('',*,*,#2218,.F.);
#3053=ORIENTED_EDGE('',*,*,#2219,.F.);
#3054=ORIENTED_EDGE('',*,*,#2213,.T.);
#3055=ORIENTED_EDGE('',*,*,#2220,.T.);
#3056=ORIENTED_EDGE('',*,*,#2221,.F.);
#3057=ORIENTED_EDGE('',*,*,#2222,.F.);
#3058=ORIENTED_EDGE('',*,*,#2223,.F.);
#3059=ORIENTED_EDGE('',*,*,#2218,.T.);
#3060=ORIENTED_EDGE('',*,*,#2224,.T.);
#3061=ORIENTED_EDGE('',*,*,#2225,.T.);
#3062=ORIENTED_EDGE('',*,*,#2226,.T.);
#3063=ORIENTED_EDGE('',*,*,#2227,.F.);
#3064=ORIENTED_EDGE('',*,*,#2228,.T.);
#3065=ORIENTED_EDGE('',*,*,#2229,.T.);
#3066=ORIENTED_EDGE('',*,*,#2230,.T.);
#3067=ORIENTED_EDGE('',*,*,#2231,.T.);
#3068=ORIENTED_EDGE('',*,*,#2232,.T.);
#3069=ORIENTED_EDGE('',*,*,#2233,.T.);
#3070=ORIENTED_EDGE('',*,*,#2234,.T.);
#3071=ORIENTED_EDGE('',*,*,#2235,.T.);
#3072=ORIENTED_EDGE('',*,*,#2236,.T.);
#3073=ORIENTED_EDGE('',*,*,#2237,.T.);
#3074=ORIENTED_EDGE('',*,*,#2238,.T.);
#3075=ORIENTED_EDGE('',*,*,#2239,.T.);
#3076=ORIENTED_EDGE('',*,*,#2240,.T.);
#3077=ORIENTED_EDGE('',*,*,#2241,.T.);
#3078=ORIENTED_EDGE('',*,*,#2242,.T.);
#3079=ORIENTED_EDGE('',*,*,#2243,.T.);
#3080=ORIENTED_EDGE('',*,*,#2244,.T.);
#3081=ORIENTED_EDGE('',*,*,#2245,.T.);
#3082=ORIENTED_EDGE('',*,*,#2246,.T.);
#3083=ORIENTED_EDGE('',*,*,#2247,.T.);
#3084=ORIENTED_EDGE('',*,*,#2248,.T.);
#3085=ORIENTED_EDGE('',*,*,#2249,.T.);
#3086=ORIENTED_EDGE('',*,*,#2250,.T.);
#3087=ORIENTED_EDGE('',*,*,#2251,.T.);
#3088=ORIENTED_EDGE('',*,*,#2252,.T.);
#3089=ORIENTED_EDGE('',*,*,#2253,.T.);
#3090=ORIENTED_EDGE('',*,*,#2254,.T.);
#3091=ORIENTED_EDGE('',*,*,#2255,.T.);
#3092=ORIENTED_EDGE('',*,*,#2256,.T.);
#3093=ORIENTED_EDGE('',*,*,#2257,.F.);
#3094=ORIENTED_EDGE('',*,*,#2258,.T.);
#3095=ORIENTED_EDGE('',*,*,#2259,.T.);
#3096=ORIENTED_EDGE('',*,*,#2260,.T.);
#3097=ORIENTED_EDGE('',*,*,#2261,.T.);
#3098=ORIENTED_EDGE('',*,*,#2262,.T.);
#3099=ORIENTED_EDGE('',*,*,#2263,.T.);
#3100=ORIENTED_EDGE('',*,*,#2264,.T.);
#3101=ORIENTED_EDGE('',*,*,#2265,.T.);
#3102=ORIENTED_EDGE('',*,*,#2266,.T.);
#3103=ORIENTED_EDGE('',*,*,#2267,.T.);
#3104=ORIENTED_EDGE('',*,*,#2268,.T.);
#3105=ORIENTED_EDGE('',*,*,#2269,.T.);
#3106=ORIENTED_EDGE('',*,*,#2270,.T.);
#3107=ORIENTED_EDGE('',*,*,#2271,.T.);
#3108=ORIENTED_EDGE('',*,*,#2272,.T.);
#3109=ORIENTED_EDGE('',*,*,#2273,.T.);
#3110=ORIENTED_EDGE('',*,*,#2274,.T.);
#3111=ORIENTED_EDGE('',*,*,#2275,.T.);
#3112=ORIENTED_EDGE('',*,*,#2276,.T.);
#3113=ORIENTED_EDGE('',*,*,#2277,.T.);
#3114=ORIENTED_EDGE('',*,*,#2278,.T.);
#3115=ORIENTED_EDGE('',*,*,#2279,.T.);
#3116=ORIENTED_EDGE('',*,*,#2280,.T.);
#3117=ORIENTED_EDGE('',*,*,#2281,.T.);
#3118=ORIENTED_EDGE('',*,*,#2282,.T.);
#3119=ORIENTED_EDGE('',*,*,#2283,.T.);
#3120=ORIENTED_EDGE('',*,*,#2284,.T.);
#3121=ORIENTED_EDGE('',*,*,#2285,.T.);
#3122=ORIENTED_EDGE('',*,*,#2221,.T.);
#3123=ORIENTED_EDGE('',*,*,#2286,.T.);
#3124=ORIENTED_EDGE('',*,*,#2287,.F.);
#3125=ORIENTED_EDGE('',*,*,#2288,.F.);
#3126=ORIENTED_EDGE('',*,*,#2289,.F.);
#3127=ORIENTED_EDGE('',*,*,#2290,.F.);
#3128=ORIENTED_EDGE('',*,*,#2256,.F.);
#3129=ORIENTED_EDGE('',*,*,#2255,.F.);
#3130=ORIENTED_EDGE('',*,*,#2254,.F.);
#3131=ORIENTED_EDGE('',*,*,#2253,.F.);
#3132=ORIENTED_EDGE('',*,*,#2252,.F.);
#3133=ORIENTED_EDGE('',*,*,#2251,.F.);
#3134=ORIENTED_EDGE('',*,*,#2250,.F.);
#3135=ORIENTED_EDGE('',*,*,#2249,.F.);
#3136=ORIENTED_EDGE('',*,*,#2248,.F.);
#3137=ORIENTED_EDGE('',*,*,#2247,.F.);
#3138=ORIENTED_EDGE('',*,*,#2246,.F.);
#3139=ORIENTED_EDGE('',*,*,#2245,.F.);
#3140=ORIENTED_EDGE('',*,*,#2244,.F.);
#3141=ORIENTED_EDGE('',*,*,#2243,.F.);
#3142=ORIENTED_EDGE('',*,*,#2242,.F.);
#3143=ORIENTED_EDGE('',*,*,#2241,.F.);
#3144=ORIENTED_EDGE('',*,*,#2240,.F.);
#3145=ORIENTED_EDGE('',*,*,#2239,.F.);
#3146=ORIENTED_EDGE('',*,*,#2238,.F.);
#3147=ORIENTED_EDGE('',*,*,#2237,.F.);
#3148=ORIENTED_EDGE('',*,*,#2236,.F.);
#3149=ORIENTED_EDGE('',*,*,#2235,.F.);
#3150=ORIENTED_EDGE('',*,*,#2234,.F.);
#3151=ORIENTED_EDGE('',*,*,#2233,.F.);
#3152=ORIENTED_EDGE('',*,*,#2232,.F.);
#3153=ORIENTED_EDGE('',*,*,#2231,.F.);
#3154=ORIENTED_EDGE('',*,*,#2230,.F.);
#3155=ORIENTED_EDGE('',*,*,#2229,.F.);
#3156=ORIENTED_EDGE('',*,*,#2228,.F.);
#3157=ORIENTED_EDGE('',*,*,#2291,.F.);
#3158=ORIENTED_EDGE('',*,*,#2112,.T.);
#3159=ORIENTED_EDGE('',*,*,#2117,.T.);
#3160=ORIENTED_EDGE('',*,*,#2116,.T.);
#3161=ORIENTED_EDGE('',*,*,#2121,.T.);
#3162=ORIENTED_EDGE('',*,*,#2125,.T.);
#3163=ORIENTED_EDGE('',*,*,#2124,.T.);
#3164=ORIENTED_EDGE('',*,*,#2129,.T.);
#3165=ORIENTED_EDGE('',*,*,#2134,.T.);
#3166=ORIENTED_EDGE('',*,*,#2133,.T.);
#3167=ORIENTED_EDGE('',*,*,#2137,.T.);
#3168=ORIENTED_EDGE('',*,*,#2142,.T.);
#3169=ORIENTED_EDGE('',*,*,#2141,.T.);
#3170=ORIENTED_EDGE('',*,*,#2145,.T.);
#3171=ORIENTED_EDGE('',*,*,#2150,.T.);
#3172=ORIENTED_EDGE('',*,*,#2149,.T.);
#3173=ORIENTED_EDGE('',*,*,#2153,.T.);
#3174=ORIENTED_EDGE('',*,*,#2158,.T.);
#3175=ORIENTED_EDGE('',*,*,#2157,.T.);
#3176=ORIENTED_EDGE('',*,*,#2162,.T.);
#3177=ORIENTED_EDGE('',*,*,#2161,.T.);
#3178=ORIENTED_EDGE('',*,*,#2166,.T.);
#3179=ORIENTED_EDGE('',*,*,#2170,.T.);
#3180=ORIENTED_EDGE('',*,*,#2169,.T.);
#3181=ORIENTED_EDGE('',*,*,#2174,.T.);
#3182=ORIENTED_EDGE('',*,*,#2178,.T.);
#3183=ORIENTED_EDGE('',*,*,#2177,.T.);
#3184=ORIENTED_EDGE('',*,*,#2182,.T.);
#3185=ORIENTED_EDGE('',*,*,#2187,.T.);
#3186=ORIENTED_EDGE('',*,*,#2186,.T.);
#3187=ORIENTED_EDGE('',*,*,#2190,.T.);
#3188=ORIENTED_EDGE('',*,*,#2195,.T.);
#3189=ORIENTED_EDGE('',*,*,#2194,.T.);
#3190=ORIENTED_EDGE('',*,*,#2198,.T.);
#3191=ORIENTED_EDGE('',*,*,#2203,.T.);
#3192=ORIENTED_EDGE('',*,*,#2202,.T.);
#3193=ORIENTED_EDGE('',*,*,#2206,.T.);
#3194=ORIENTED_EDGE('',*,*,#2211,.T.);
#3195=ORIENTED_EDGE('',*,*,#2210,.T.);
#3196=ORIENTED_EDGE('',*,*,#2215,.T.);
#3197=ORIENTED_EDGE('',*,*,#2214,.T.);
#3198=ORIENTED_EDGE('',*,*,#2219,.T.);
#3199=ORIENTED_EDGE('',*,*,#2223,.T.);
#3200=ORIENTED_EDGE('',*,*,#2222,.T.);
#3201=ORIENTED_EDGE('',*,*,#2289,.T.);
#3202=ORIENTED_EDGE('',*,*,#2288,.T.);
#3203=ORIENTED_EDGE('',*,*,#2292,.F.);
#3204=ORIENTED_EDGE('',*,*,#2293,.F.);
#3205=ORIENTED_EDGE('',*,*,#2286,.F.);
#3206=ORIENTED_EDGE('',*,*,#2225,.F.);
#3207=ORIENTED_EDGE('',*,*,#2224,.F.);
#3208=ORIENTED_EDGE('',*,*,#2220,.F.);
#3209=ORIENTED_EDGE('',*,*,#2217,.F.);
#3210=ORIENTED_EDGE('',*,*,#2216,.F.);
#3211=ORIENTED_EDGE('',*,*,#2212,.F.);
#3212=ORIENTED_EDGE('',*,*,#2208,.F.);
#3213=ORIENTED_EDGE('',*,*,#2207,.F.);
#3214=ORIENTED_EDGE('',*,*,#2204,.F.);
#3215=ORIENTED_EDGE('',*,*,#2200,.F.);
#3216=ORIENTED_EDGE('',*,*,#2199,.F.);
#3217=ORIENTED_EDGE('',*,*,#2196,.F.);
#3218=ORIENTED_EDGE('',*,*,#2192,.F.);
#3219=ORIENTED_EDGE('',*,*,#2191,.F.);
#3220=ORIENTED_EDGE('',*,*,#2188,.F.);
#3221=ORIENTED_EDGE('',*,*,#2184,.F.);
#3222=ORIENTED_EDGE('',*,*,#2183,.F.);
#3223=ORIENTED_EDGE('',*,*,#2180,.F.);
#3224=ORIENTED_EDGE('',*,*,#2179,.F.);
#3225=ORIENTED_EDGE('',*,*,#2175,.F.);
#3226=ORIENTED_EDGE('',*,*,#2172,.F.);
#3227=ORIENTED_EDGE('',*,*,#2171,.F.);
#3228=ORIENTED_EDGE('',*,*,#2167,.F.);
#3229=ORIENTED_EDGE('',*,*,#2164,.F.);
#3230=ORIENTED_EDGE('',*,*,#2163,.F.);
#3231=ORIENTED_EDGE('',*,*,#2159,.F.);
#3232=ORIENTED_EDGE('',*,*,#2155,.F.);
#3233=ORIENTED_EDGE('',*,*,#2154,.F.);
#3234=ORIENTED_EDGE('',*,*,#2151,.F.);
#3235=ORIENTED_EDGE('',*,*,#2147,.F.);
#3236=ORIENTED_EDGE('',*,*,#2146,.F.);
#3237=ORIENTED_EDGE('',*,*,#2143,.F.);
#3238=ORIENTED_EDGE('',*,*,#2139,.F.);
#3239=ORIENTED_EDGE('',*,*,#2138,.F.);
#3240=ORIENTED_EDGE('',*,*,#2135,.F.);
#3241=ORIENTED_EDGE('',*,*,#2131,.F.);
#3242=ORIENTED_EDGE('',*,*,#2130,.F.);
#3243=ORIENTED_EDGE('',*,*,#2127,.F.);
#3244=ORIENTED_EDGE('',*,*,#2126,.F.);
#3245=ORIENTED_EDGE('',*,*,#2122,.F.);
#3246=ORIENTED_EDGE('',*,*,#2119,.F.);
#3247=ORIENTED_EDGE('',*,*,#2118,.F.);
#3248=ORIENTED_EDGE('',*,*,#2114,.F.);
#3249=ORIENTED_EDGE('',*,*,#2294,.F.);
#3250=ORIENTED_EDGE('',*,*,#2226,.F.);
#3251=ORIENTED_EDGE('',*,*,#2285,.F.);
#3252=ORIENTED_EDGE('',*,*,#2284,.F.);
#3253=ORIENTED_EDGE('',*,*,#2283,.F.);
#3254=ORIENTED_EDGE('',*,*,#2282,.F.);
#3255=ORIENTED_EDGE('',*,*,#2281,.F.);
#3256=ORIENTED_EDGE('',*,*,#2280,.F.);
#3257=ORIENTED_EDGE('',*,*,#2279,.F.);
#3258=ORIENTED_EDGE('',*,*,#2278,.F.);
#3259=ORIENTED_EDGE('',*,*,#2277,.F.);
#3260=ORIENTED_EDGE('',*,*,#2276,.F.);
#3261=ORIENTED_EDGE('',*,*,#2275,.F.);
#3262=ORIENTED_EDGE('',*,*,#2274,.F.);
#3263=ORIENTED_EDGE('',*,*,#2273,.F.);
#3264=ORIENTED_EDGE('',*,*,#2272,.F.);
#3265=ORIENTED_EDGE('',*,*,#2271,.F.);
#3266=ORIENTED_EDGE('',*,*,#2270,.F.);
#3267=ORIENTED_EDGE('',*,*,#2269,.F.);
#3268=ORIENTED_EDGE('',*,*,#2268,.F.);
#3269=ORIENTED_EDGE('',*,*,#2267,.F.);
#3270=ORIENTED_EDGE('',*,*,#2266,.F.);
#3271=ORIENTED_EDGE('',*,*,#2265,.F.);
#3272=ORIENTED_EDGE('',*,*,#2264,.F.);
#3273=ORIENTED_EDGE('',*,*,#2263,.F.);
#3274=ORIENTED_EDGE('',*,*,#2262,.F.);
#3275=ORIENTED_EDGE('',*,*,#2261,.F.);
#3276=ORIENTED_EDGE('',*,*,#2260,.F.);
#3277=ORIENTED_EDGE('',*,*,#2259,.F.);
#3278=ORIENTED_EDGE('',*,*,#2258,.F.);
#3279=ORIENTED_EDGE('',*,*,#2290,.T.);
#3280=ORIENTED_EDGE('',*,*,#2287,.T.);
#3281=ORIENTED_EDGE('',*,*,#2293,.T.);
#3282=ORIENTED_EDGE('',*,*,#2292,.T.);
#3283=ORIENTED_EDGE('',*,*,#2257,.T.);
#3284=ORIENTED_EDGE('',*,*,#2291,.T.);
#3285=ORIENTED_EDGE('',*,*,#2227,.T.);
#3286=ORIENTED_EDGE('',*,*,#2294,.T.);
#3287=ORIENTED_EDGE('',*,*,#2113,.T.);
#3288=ORIENTED_EDGE('',*,*,#2295,.T.);
#3289=ORIENTED_EDGE('',*,*,#2295,.F.);
#3290=ORIENTED_EDGE('',*,*,#2296,.F.);
#3291=ORIENTED_EDGE('',*,*,#2297,.T.);
#3292=ORIENTED_EDGE('',*,*,#2298,.F.);
#3293=ORIENTED_EDGE('',*,*,#2297,.F.);
#3294=ORIENTED_EDGE('',*,*,#2299,.T.);
#3295=ORIENTED_EDGE('',*,*,#2300,.T.);
#3296=ORIENTED_EDGE('',*,*,#2301,.T.);
#3297=ORIENTED_EDGE('',*,*,#2302,.T.);
#3298=ORIENTED_EDGE('',*,*,#2303,.T.);
#3299=ORIENTED_EDGE('',*,*,#2304,.T.);
#3300=ORIENTED_EDGE('',*,*,#2298,.T.);
#3301=ORIENTED_EDGE('',*,*,#2305,.F.);
#3302=ORIENTED_EDGE('',*,*,#2306,.F.);
#3303=ORIENTED_EDGE('',*,*,#2307,.T.);
#3304=ORIENTED_EDGE('',*,*,#2300,.F.);
#3305=ORIENTED_EDGE('',*,*,#2307,.F.);
#3306=ORIENTED_EDGE('',*,*,#2308,.F.);
#3307=ORIENTED_EDGE('',*,*,#2309,.T.);
#3308=ORIENTED_EDGE('',*,*,#2301,.F.);
#3309=ORIENTED_EDGE('',*,*,#2309,.F.);
#3310=ORIENTED_EDGE('',*,*,#2310,.F.);
#3311=ORIENTED_EDGE('',*,*,#2311,.T.);
#3312=ORIENTED_EDGE('',*,*,#2302,.F.);
#3313=ORIENTED_EDGE('',*,*,#2311,.F.);
#3314=ORIENTED_EDGE('',*,*,#2312,.F.);
#3315=ORIENTED_EDGE('',*,*,#2313,.T.);
#3316=ORIENTED_EDGE('',*,*,#2303,.F.);
#3317=ORIENTED_EDGE('',*,*,#2313,.F.);
#3318=ORIENTED_EDGE('',*,*,#2314,.F.);
#3319=ORIENTED_EDGE('',*,*,#2315,.F.);
#3320=ORIENTED_EDGE('',*,*,#2304,.F.);
#3321=ORIENTED_EDGE('',*,*,#2315,.T.);
#3322=ORIENTED_EDGE('',*,*,#2316,.F.);
#3323=ORIENTED_EDGE('',*,*,#2305,.T.);
#3324=ORIENTED_EDGE('',*,*,#2299,.F.);
#3325=ORIENTED_EDGE('',*,*,#2316,.T.);
#3326=ORIENTED_EDGE('',*,*,#2314,.T.);
#3327=ORIENTED_EDGE('',*,*,#2312,.T.);
#3328=ORIENTED_EDGE('',*,*,#2310,.T.);
#3329=ORIENTED_EDGE('',*,*,#2308,.T.);
#3330=ORIENTED_EDGE('',*,*,#2306,.T.);
#3331=ORIENTED_EDGE('',*,*,#2296,.T.);
#3332=ORIENTED_EDGE('',*,*,#2317,.T.);
#3333=ORIENTED_EDGE('',*,*,#2318,.F.);
#3334=ORIENTED_EDGE('',*,*,#2319,.F.);
#3335=ORIENTED_EDGE('',*,*,#2320,.F.);
#3336=ORIENTED_EDGE('',*,*,#2321,.F.);
#3337=ORIENTED_EDGE('',*,*,#2322,.F.);
#3338=ORIENTED_EDGE('',*,*,#2323,.F.);
#3339=ORIENTED_EDGE('',*,*,#2324,.F.);
#3340=ORIENTED_EDGE('',*,*,#2325,.T.);
#3341=ORIENTED_EDGE('',*,*,#2326,.T.);
#3342=ORIENTED_EDGE('',*,*,#2327,.F.);
#3343=ORIENTED_EDGE('',*,*,#2328,.F.);
#3344=ORIENTED_EDGE('',*,*,#2329,.F.);
#3345=ORIENTED_EDGE('',*,*,#2330,.T.);
#3346=ORIENTED_EDGE('',*,*,#2331,.T.);
#3347=ORIENTED_EDGE('',*,*,#2332,.T.);
#3348=ORIENTED_EDGE('',*,*,#2325,.F.);
#3349=ORIENTED_EDGE('',*,*,#2333,.F.);
#3350=ORIENTED_EDGE('',*,*,#2334,.F.);
#3351=ORIENTED_EDGE('',*,*,#2335,.F.);
#3352=ORIENTED_EDGE('',*,*,#2336,.T.);
#3353=ORIENTED_EDGE('',*,*,#2337,.F.);
#3354=ORIENTED_EDGE('',*,*,#2322,.T.);
#3355=ORIENTED_EDGE('',*,*,#2338,.T.);
#3356=ORIENTED_EDGE('',*,*,#2320,.T.);
#3357=ORIENTED_EDGE('',*,*,#2339,.F.);
#3358=ORIENTED_EDGE('',*,*,#2326,.F.);
#3359=ORIENTED_EDGE('',*,*,#2332,.F.);
#3360=ORIENTED_EDGE('',*,*,#2331,.F.);
#3361=ORIENTED_EDGE('',*,*,#2340,.F.);
#3362=ORIENTED_EDGE('',*,*,#2336,.F.);
#3363=ORIENTED_EDGE('',*,*,#2334,.T.);
#3364=ORIENTED_EDGE('',*,*,#2340,.T.);
#3365=ORIENTED_EDGE('',*,*,#2330,.F.);
#3366=ORIENTED_EDGE('',*,*,#2341,.F.);
#3367=ORIENTED_EDGE('',*,*,#2342,.F.);
#3368=ORIENTED_EDGE('',*,*,#2343,.F.);
#3369=ORIENTED_EDGE('',*,*,#2321,.T.);
#3370=ORIENTED_EDGE('',*,*,#2344,.F.);
#3371=ORIENTED_EDGE('',*,*,#2317,.F.);
#3372=ORIENTED_EDGE('',*,*,#2338,.F.);
#3373=ORIENTED_EDGE('',*,*,#2345,.F.);
#3374=ORIENTED_EDGE('',*,*,#2342,.T.);
#3375=ORIENTED_EDGE('',*,*,#2341,.T.);
#3376=ORIENTED_EDGE('',*,*,#2333,.T.);
#3377=ORIENTED_EDGE('',*,*,#2329,.T.);
#3378=ORIENTED_EDGE('',*,*,#2328,.T.);
#3379=ORIENTED_EDGE('',*,*,#2346,.F.);
#3380=ORIENTED_EDGE('',*,*,#2318,.T.);
#3381=ORIENTED_EDGE('',*,*,#2344,.T.);
#3382=ORIENTED_EDGE('',*,*,#2324,.T.);
#3383=ORIENTED_EDGE('',*,*,#2347,.T.);
#3384=ORIENTED_EDGE('',*,*,#2348,.T.);
#3385=ORIENTED_EDGE('',*,*,#2349,.T.);
#3386=ORIENTED_EDGE('',*,*,#2350,.T.);
#3387=ORIENTED_EDGE('',*,*,#2351,.T.);
#3388=ORIENTED_EDGE('',*,*,#2352,.T.);
#3389=ORIENTED_EDGE('',*,*,#2349,.F.);
#3390=ORIENTED_EDGE('',*,*,#2353,.T.);
#3391=ORIENTED_EDGE('',*,*,#2354,.T.);
#3392=ORIENTED_EDGE('',*,*,#2355,.T.);
#3393=ORIENTED_EDGE('',*,*,#2351,.F.);
#3394=ORIENTED_EDGE('',*,*,#2356,.T.);
#3395=ORIENTED_EDGE('',*,*,#2357,.T.);
#3396=ORIENTED_EDGE('',*,*,#2358,.T.);
#3397=ORIENTED_EDGE('',*,*,#2354,.F.);
#3398=ORIENTED_EDGE('',*,*,#2359,.T.);
#3399=ORIENTED_EDGE('',*,*,#2360,.T.);
#3400=ORIENTED_EDGE('',*,*,#2361,.T.);
#3401=ORIENTED_EDGE('',*,*,#2357,.F.);
#3402=ORIENTED_EDGE('',*,*,#2362,.T.);
#3403=ORIENTED_EDGE('',*,*,#2363,.T.);
#3404=ORIENTED_EDGE('',*,*,#2364,.T.);
#3405=ORIENTED_EDGE('',*,*,#2360,.F.);
#3406=ORIENTED_EDGE('',*,*,#2365,.T.);
#3407=ORIENTED_EDGE('',*,*,#2366,.T.);
#3408=ORIENTED_EDGE('',*,*,#2367,.T.);
#3409=ORIENTED_EDGE('',*,*,#2363,.F.);
#3410=ORIENTED_EDGE('',*,*,#2368,.T.);
#3411=ORIENTED_EDGE('',*,*,#2369,.T.);
#3412=ORIENTED_EDGE('',*,*,#2370,.T.);
#3413=ORIENTED_EDGE('',*,*,#2366,.F.);
#3414=ORIENTED_EDGE('',*,*,#2371,.T.);
#3415=ORIENTED_EDGE('',*,*,#2372,.T.);
#3416=ORIENTED_EDGE('',*,*,#2373,.T.);
#3417=ORIENTED_EDGE('',*,*,#2369,.F.);
#3418=ORIENTED_EDGE('',*,*,#2374,.T.);
#3419=ORIENTED_EDGE('',*,*,#2375,.T.);
#3420=ORIENTED_EDGE('',*,*,#2376,.T.);
#3421=ORIENTED_EDGE('',*,*,#2372,.F.);
#3422=ORIENTED_EDGE('',*,*,#2377,.T.);
#3423=ORIENTED_EDGE('',*,*,#2378,.T.);
#3424=ORIENTED_EDGE('',*,*,#2379,.T.);
#3425=ORIENTED_EDGE('',*,*,#2375,.F.);
#3426=ORIENTED_EDGE('',*,*,#2380,.T.);
#3427=ORIENTED_EDGE('',*,*,#2381,.T.);
#3428=ORIENTED_EDGE('',*,*,#2382,.T.);
#3429=ORIENTED_EDGE('',*,*,#2378,.F.);
#3430=ORIENTED_EDGE('',*,*,#2383,.T.);
#3431=ORIENTED_EDGE('',*,*,#2384,.T.);
#3432=ORIENTED_EDGE('',*,*,#2385,.T.);
#3433=ORIENTED_EDGE('',*,*,#2381,.F.);
#3434=ORIENTED_EDGE('',*,*,#2386,.T.);
#3435=ORIENTED_EDGE('',*,*,#2384,.F.);
#3436=ORIENTED_EDGE('',*,*,#2387,.T.);
#3437=ORIENTED_EDGE('',*,*,#2347,.F.);
#3438=ORIENTED_EDGE('',*,*,#2388,.T.);
#3439=ORIENTED_EDGE('',*,*,#2368,.F.);
#3440=ORIENTED_EDGE('',*,*,#2389,.T.);
#3441=ORIENTED_EDGE('',*,*,#2390,.F.);
#3442=ORIENTED_EDGE('',*,*,#2391,.T.);
#3443=ORIENTED_EDGE('',*,*,#2365,.F.);
#3444=ORIENTED_EDGE('',*,*,#2392,.F.);
#3445=ORIENTED_EDGE('',*,*,#2393,.F.);
#3446=ORIENTED_EDGE('',*,*,#2389,.F.);
#3447=ORIENTED_EDGE('',*,*,#2362,.F.);
#3448=ORIENTED_EDGE('',*,*,#2394,.T.);
#3449=ORIENTED_EDGE('',*,*,#2395,.F.);
#3450=ORIENTED_EDGE('',*,*,#2392,.T.);
#3451=ORIENTED_EDGE('',*,*,#2359,.F.);
#3452=ORIENTED_EDGE('',*,*,#2356,.F.);
#3453=ORIENTED_EDGE('',*,*,#2353,.F.);
#3454=ORIENTED_EDGE('',*,*,#2348,.F.);
#3455=ORIENTED_EDGE('',*,*,#2387,.F.);
#3456=ORIENTED_EDGE('',*,*,#2396,.F.);
#3457=ORIENTED_EDGE('',*,*,#2397,.F.);
#3458=ORIENTED_EDGE('',*,*,#2398,.F.);
#3459=ORIENTED_EDGE('',*,*,#2399,.F.);
#3460=ORIENTED_EDGE('',*,*,#2400,.F.);
#3461=ORIENTED_EDGE('',*,*,#2401,.F.);
#3462=ORIENTED_EDGE('',*,*,#2394,.F.);
#3463=ORIENTED_EDGE('',*,*,#2382,.F.);
#3464=ORIENTED_EDGE('',*,*,#2385,.F.);
#3465=ORIENTED_EDGE('',*,*,#2388,.F.);
#3466=ORIENTED_EDGE('',*,*,#2402,.F.);
#3467=ORIENTED_EDGE('',*,*,#2373,.F.);
#3468=ORIENTED_EDGE('',*,*,#2403,.T.);
#3469=ORIENTED_EDGE('',*,*,#2355,.F.);
#3470=ORIENTED_EDGE('',*,*,#2404,.T.);
#3471=ORIENTED_EDGE('',*,*,#2376,.F.);
#3472=ORIENTED_EDGE('',*,*,#2405,.F.);
#3473=ORIENTED_EDGE('',*,*,#2352,.F.);
#3474=ORIENTED_EDGE('',*,*,#2403,.F.);
#3475=ORIENTED_EDGE('',*,*,#2379,.F.);
#3476=ORIENTED_EDGE('',*,*,#2402,.T.);
#3477=ORIENTED_EDGE('',*,*,#2350,.F.);
#3478=ORIENTED_EDGE('',*,*,#2405,.T.);
#3479=ORIENTED_EDGE('',*,*,#2406,.T.);
#3480=ORIENTED_EDGE('',*,*,#2407,.T.);
#3481=ORIENTED_EDGE('',*,*,#2408,.T.);
#3482=ORIENTED_EDGE('',*,*,#2409,.T.);
#3483=ORIENTED_EDGE('',*,*,#2410,.T.);
#3484=ORIENTED_EDGE('',*,*,#2411,.T.);
#3485=ORIENTED_EDGE('',*,*,#2408,.F.);
#3486=ORIENTED_EDGE('',*,*,#2412,.T.);
#3487=ORIENTED_EDGE('',*,*,#2413,.T.);
#3488=ORIENTED_EDGE('',*,*,#2414,.T.);
#3489=ORIENTED_EDGE('',*,*,#2410,.F.);
#3490=ORIENTED_EDGE('',*,*,#2415,.T.);
#3491=ORIENTED_EDGE('',*,*,#2416,.T.);
#3492=ORIENTED_EDGE('',*,*,#2417,.T.);
#3493=ORIENTED_EDGE('',*,*,#2413,.F.);
#3494=ORIENTED_EDGE('',*,*,#2418,.T.);
#3495=ORIENTED_EDGE('',*,*,#2419,.T.);
#3496=ORIENTED_EDGE('',*,*,#2420,.T.);
#3497=ORIENTED_EDGE('',*,*,#2416,.F.);
#3498=ORIENTED_EDGE('',*,*,#2390,.T.);
#3499=ORIENTED_EDGE('',*,*,#2421,.T.);
#3500=ORIENTED_EDGE('',*,*,#2422,.T.);
#3501=ORIENTED_EDGE('',*,*,#2419,.F.);
#3502=ORIENTED_EDGE('',*,*,#2393,.T.);
#3503=ORIENTED_EDGE('',*,*,#2423,.T.);
#3504=ORIENTED_EDGE('',*,*,#2424,.T.);
#3505=ORIENTED_EDGE('',*,*,#2421,.F.);
#3506=ORIENTED_EDGE('',*,*,#2395,.T.);
#3507=ORIENTED_EDGE('',*,*,#2425,.T.);
#3508=ORIENTED_EDGE('',*,*,#2426,.T.);
#3509=ORIENTED_EDGE('',*,*,#2423,.F.);
#3510=ORIENTED_EDGE('',*,*,#2401,.T.);
#3511=ORIENTED_EDGE('',*,*,#2427,.T.);
#3512=ORIENTED_EDGE('',*,*,#2428,.T.);
#3513=ORIENTED_EDGE('',*,*,#2425,.F.);
#3514=ORIENTED_EDGE('',*,*,#2400,.T.);
#3515=ORIENTED_EDGE('',*,*,#2429,.T.);
#3516=ORIENTED_EDGE('',*,*,#2430,.T.);
#3517=ORIENTED_EDGE('',*,*,#2427,.F.);
#3518=ORIENTED_EDGE('',*,*,#2399,.T.);
#3519=ORIENTED_EDGE('',*,*,#2431,.T.);
#3520=ORIENTED_EDGE('',*,*,#2432,.T.);
#3521=ORIENTED_EDGE('',*,*,#2429,.F.);
#3522=ORIENTED_EDGE('',*,*,#2398,.T.);
#3523=ORIENTED_EDGE('',*,*,#2433,.T.);
#3524=ORIENTED_EDGE('',*,*,#2434,.T.);
#3525=ORIENTED_EDGE('',*,*,#2431,.F.);
#3526=ORIENTED_EDGE('',*,*,#2397,.T.);
#3527=ORIENTED_EDGE('',*,*,#2435,.T.);
#3528=ORIENTED_EDGE('',*,*,#2436,.T.);
#3529=ORIENTED_EDGE('',*,*,#2433,.F.);
#3530=ORIENTED_EDGE('',*,*,#2437,.T.);
#3531=ORIENTED_EDGE('',*,*,#2435,.F.);
#3532=ORIENTED_EDGE('',*,*,#2438,.T.);
#3533=ORIENTED_EDGE('',*,*,#2406,.F.);
#3534=ORIENTED_EDGE('',*,*,#2439,.T.);
#3535=ORIENTED_EDGE('',*,*,#2434,.F.);
#3536=ORIENTED_EDGE('',*,*,#2436,.F.);
#3537=ORIENTED_EDGE('',*,*,#2439,.F.);
#3538=ORIENTED_EDGE('',*,*,#2440,.F.);
#3539=ORIENTED_EDGE('',*,*,#2428,.F.);
#3540=ORIENTED_EDGE('',*,*,#2441,.T.);
#3541=ORIENTED_EDGE('',*,*,#2414,.F.);
#3542=ORIENTED_EDGE('',*,*,#2442,.T.);
#3543=ORIENTED_EDGE('',*,*,#2430,.F.);
#3544=ORIENTED_EDGE('',*,*,#2443,.F.);
#3545=ORIENTED_EDGE('',*,*,#2411,.F.);
#3546=ORIENTED_EDGE('',*,*,#2441,.F.);
#3547=ORIENTED_EDGE('',*,*,#2432,.F.);
#3548=ORIENTED_EDGE('',*,*,#2440,.T.);
#3549=ORIENTED_EDGE('',*,*,#2409,.F.);
#3550=ORIENTED_EDGE('',*,*,#2443,.T.);
#3551=ORIENTED_EDGE('',*,*,#2371,.F.);
#3552=ORIENTED_EDGE('',*,*,#2391,.F.);
#3553=ORIENTED_EDGE('',*,*,#2418,.F.);
#3554=ORIENTED_EDGE('',*,*,#2415,.F.);
#3555=ORIENTED_EDGE('',*,*,#2412,.F.);
#3556=ORIENTED_EDGE('',*,*,#2407,.F.);
#3557=ORIENTED_EDGE('',*,*,#2438,.F.);
#3558=ORIENTED_EDGE('',*,*,#2444,.F.);
#3559=ORIENTED_EDGE('',*,*,#2383,.F.);
#3560=ORIENTED_EDGE('',*,*,#2380,.F.);
#3561=ORIENTED_EDGE('',*,*,#2377,.F.);
#3562=ORIENTED_EDGE('',*,*,#2374,.F.);
#3563=ORIENTED_EDGE('',*,*,#2386,.F.);
#3564=ORIENTED_EDGE('',*,*,#2444,.T.);
#3565=ORIENTED_EDGE('',*,*,#2437,.F.);
#3566=ORIENTED_EDGE('',*,*,#2396,.T.);
#3567=ORIENTED_EDGE('',*,*,#2370,.F.);
#3568=ORIENTED_EDGE('',*,*,#2404,.F.);
#3569=ORIENTED_EDGE('',*,*,#2358,.F.);
#3570=ORIENTED_EDGE('',*,*,#2361,.F.);
#3571=ORIENTED_EDGE('',*,*,#2364,.F.);
#3572=ORIENTED_EDGE('',*,*,#2367,.F.);
#3573=ORIENTED_EDGE('',*,*,#2345,.T.);
#3574=ORIENTED_EDGE('',*,*,#2323,.T.);
#3575=ORIENTED_EDGE('',*,*,#2337,.T.);
#3576=ORIENTED_EDGE('',*,*,#2335,.T.);
#3577=ORIENTED_EDGE('',*,*,#2343,.T.);
#3578=ORIENTED_EDGE('',*,*,#2426,.F.);
#3579=ORIENTED_EDGE('',*,*,#2442,.F.);
#3580=ORIENTED_EDGE('',*,*,#2417,.F.);
#3581=ORIENTED_EDGE('',*,*,#2420,.F.);
#3582=ORIENTED_EDGE('',*,*,#2422,.F.);
#3583=ORIENTED_EDGE('',*,*,#2424,.F.);
#3584=ORIENTED_EDGE('',*,*,#2346,.T.);
#3585=ORIENTED_EDGE('',*,*,#2327,.T.);
#3586=ORIENTED_EDGE('',*,*,#2339,.T.);
#3587=ORIENTED_EDGE('',*,*,#2319,.T.);
#3588=ORIENTED_EDGE('',*,*,#2445,.T.);
#3589=ORIENTED_EDGE('',*,*,#2446,.T.);
#3590=ORIENTED_EDGE('',*,*,#2447,.F.);
#3591=ORIENTED_EDGE('',*,*,#2448,.F.);
#3592=ORIENTED_EDGE('',*,*,#2449,.T.);
#3593=ORIENTED_EDGE('',*,*,#2450,.T.);
#3594=ORIENTED_EDGE('',*,*,#2451,.T.);
#3595=ORIENTED_EDGE('',*,*,#2445,.F.);
#3596=ORIENTED_EDGE('',*,*,#2452,.F.);
#3597=ORIENTED_EDGE('',*,*,#2453,.F.);
#3598=ORIENTED_EDGE('',*,*,#2454,.T.);
#3599=ORIENTED_EDGE('',*,*,#2455,.T.);
#3600=ORIENTED_EDGE('',*,*,#2456,.T.);
#3601=ORIENTED_EDGE('',*,*,#2449,.F.);
#3602=ORIENTED_EDGE('',*,*,#2457,.F.);
#3603=ORIENTED_EDGE('',*,*,#2458,.F.);
#3604=ORIENTED_EDGE('',*,*,#2459,.T.);
#3605=ORIENTED_EDGE('',*,*,#2460,.T.);
#3606=ORIENTED_EDGE('',*,*,#2461,.T.);
#3607=ORIENTED_EDGE('',*,*,#2454,.F.);
#3608=ORIENTED_EDGE('',*,*,#2462,.F.);
#3609=ORIENTED_EDGE('',*,*,#2463,.F.);
#3610=ORIENTED_EDGE('',*,*,#2464,.T.);
#3611=ORIENTED_EDGE('',*,*,#2465,.T.);
#3612=ORIENTED_EDGE('',*,*,#2466,.T.);
#3613=ORIENTED_EDGE('',*,*,#2459,.F.);
#3614=ORIENTED_EDGE('',*,*,#2467,.F.);
#3615=ORIENTED_EDGE('',*,*,#2468,.F.);
#3616=ORIENTED_EDGE('',*,*,#2469,.T.);
#3617=ORIENTED_EDGE('',*,*,#2470,.T.);
#3618=ORIENTED_EDGE('',*,*,#2471,.T.);
#3619=ORIENTED_EDGE('',*,*,#2464,.F.);
#3620=ORIENTED_EDGE('',*,*,#2472,.F.);
#3621=ORIENTED_EDGE('',*,*,#2473,.F.);
#3622=ORIENTED_EDGE('',*,*,#2474,.F.);
#3623=ORIENTED_EDGE('',*,*,#2475,.F.);
#3624=ORIENTED_EDGE('',*,*,#2476,.F.);
#3625=ORIENTED_EDGE('',*,*,#2477,.F.);
#3626=ORIENTED_EDGE('',*,*,#2478,.T.);
#3627=ORIENTED_EDGE('',*,*,#2479,.T.);
#3628=ORIENTED_EDGE('',*,*,#2480,.T.);
#3629=ORIENTED_EDGE('',*,*,#2481,.T.);
#3630=ORIENTED_EDGE('',*,*,#2482,.F.);
#3631=ORIENTED_EDGE('',*,*,#2483,.T.);
#3632=ORIENTED_EDGE('',*,*,#2484,.T.);
#3633=ORIENTED_EDGE('',*,*,#2485,.T.);
#3634=ORIENTED_EDGE('',*,*,#2486,.T.);
#3635=ORIENTED_EDGE('',*,*,#2480,.F.);
#3636=ORIENTED_EDGE('',*,*,#2487,.T.);
#3637=ORIENTED_EDGE('',*,*,#2488,.T.);
#3638=ORIENTED_EDGE('',*,*,#2489,.T.);
#3639=ORIENTED_EDGE('',*,*,#2490,.T.);
#3640=ORIENTED_EDGE('',*,*,#2484,.F.);
#3641=ORIENTED_EDGE('',*,*,#2491,.T.);
#3642=ORIENTED_EDGE('',*,*,#2492,.T.);
#3643=ORIENTED_EDGE('',*,*,#2493,.T.);
#3644=ORIENTED_EDGE('',*,*,#2488,.F.);
#3645=ORIENTED_EDGE('',*,*,#2494,.T.);
#3646=ORIENTED_EDGE('',*,*,#2495,.T.);
#3647=ORIENTED_EDGE('',*,*,#2496,.T.);
#3648=ORIENTED_EDGE('',*,*,#2497,.T.);
#3649=ORIENTED_EDGE('',*,*,#2492,.F.);
#3650=ORIENTED_EDGE('',*,*,#2498,.T.);
#3651=ORIENTED_EDGE('',*,*,#2499,.T.);
#3652=ORIENTED_EDGE('',*,*,#2500,.T.);
#3653=ORIENTED_EDGE('',*,*,#2495,.F.);
#3654=ORIENTED_EDGE('',*,*,#2501,.T.);
#3655=ORIENTED_EDGE('',*,*,#2502,.F.);
#3656=ORIENTED_EDGE('',*,*,#2503,.T.);
#3657=ORIENTED_EDGE('',*,*,#2504,.T.);
#3658=ORIENTED_EDGE('',*,*,#2505,.T.);
#3659=ORIENTED_EDGE('',*,*,#2502,.T.);
#3660=ORIENTED_EDGE('',*,*,#2506,.T.);
#3661=ORIENTED_EDGE('',*,*,#2507,.T.);
#3662=ORIENTED_EDGE('',*,*,#2499,.F.);
#3663=ORIENTED_EDGE('',*,*,#2508,.T.);
#3664=ORIENTED_EDGE('',*,*,#2474,.T.);
#3665=ORIENTED_EDGE('',*,*,#2509,.T.);
#3666=ORIENTED_EDGE('',*,*,#2510,.T.);
#3667=ORIENTED_EDGE('',*,*,#2469,.F.);
#3668=ORIENTED_EDGE('',*,*,#2511,.F.);
#3669=ORIENTED_EDGE('',*,*,#2512,.F.);
#3670=ORIENTED_EDGE('',*,*,#2513,.F.);
#3671=ORIENTED_EDGE('',*,*,#2446,.F.);
#3672=ORIENTED_EDGE('',*,*,#2451,.F.);
#3673=ORIENTED_EDGE('',*,*,#2450,.F.);
#3674=ORIENTED_EDGE('',*,*,#2456,.F.);
#3675=ORIENTED_EDGE('',*,*,#2455,.F.);
#3676=ORIENTED_EDGE('',*,*,#2461,.F.);
#3677=ORIENTED_EDGE('',*,*,#2460,.F.);
#3678=ORIENTED_EDGE('',*,*,#2466,.F.);
#3679=ORIENTED_EDGE('',*,*,#2465,.F.);
#3680=ORIENTED_EDGE('',*,*,#2471,.F.);
#3681=ORIENTED_EDGE('',*,*,#2470,.F.);
#3682=ORIENTED_EDGE('',*,*,#2510,.F.);
#3683=ORIENTED_EDGE('',*,*,#2509,.F.);
#3684=ORIENTED_EDGE('',*,*,#2479,.F.);
#3685=ORIENTED_EDGE('',*,*,#2478,.F.);
#3686=ORIENTED_EDGE('',*,*,#2514,.F.);
#3687=ORIENTED_EDGE('',*,*,#2503,.F.);
#3688=ORIENTED_EDGE('',*,*,#2508,.F.);
#3689=ORIENTED_EDGE('',*,*,#2501,.F.);
#3690=ORIENTED_EDGE('',*,*,#2498,.F.);
#3691=ORIENTED_EDGE('',*,*,#2494,.F.);
#3692=ORIENTED_EDGE('',*,*,#2491,.F.);
#3693=ORIENTED_EDGE('',*,*,#2487,.F.);
#3694=ORIENTED_EDGE('',*,*,#2483,.F.);
#3695=ORIENTED_EDGE('',*,*,#2515,.F.);
#3696=ORIENTED_EDGE('',*,*,#2516,.F.);
#3697=ORIENTED_EDGE('',*,*,#2481,.F.);
#3698=ORIENTED_EDGE('',*,*,#2486,.F.);
#3699=ORIENTED_EDGE('',*,*,#2485,.F.);
#3700=ORIENTED_EDGE('',*,*,#2490,.F.);
#3701=ORIENTED_EDGE('',*,*,#2489,.F.);
#3702=ORIENTED_EDGE('',*,*,#2493,.F.);
#3703=ORIENTED_EDGE('',*,*,#2497,.F.);
#3704=ORIENTED_EDGE('',*,*,#2496,.F.);
#3705=ORIENTED_EDGE('',*,*,#2500,.F.);
#3706=ORIENTED_EDGE('',*,*,#2507,.F.);
#3707=ORIENTED_EDGE('',*,*,#2506,.F.);
#3708=ORIENTED_EDGE('',*,*,#2505,.F.);
#3709=ORIENTED_EDGE('',*,*,#2517,.F.);
#3710=ORIENTED_EDGE('',*,*,#2476,.T.);
#3711=ORIENTED_EDGE('',*,*,#2475,.T.);
#3712=ORIENTED_EDGE('',*,*,#2512,.T.);
#3713=ORIENTED_EDGE('',*,*,#2511,.T.);
#3714=ORIENTED_EDGE('',*,*,#2473,.T.);
#3715=ORIENTED_EDGE('',*,*,#2472,.T.);
#3716=ORIENTED_EDGE('',*,*,#2468,.T.);
#3717=ORIENTED_EDGE('',*,*,#2467,.T.);
#3718=ORIENTED_EDGE('',*,*,#2463,.T.);
#3719=ORIENTED_EDGE('',*,*,#2462,.T.);
#3720=ORIENTED_EDGE('',*,*,#2458,.T.);
#3721=ORIENTED_EDGE('',*,*,#2457,.T.);
#3722=ORIENTED_EDGE('',*,*,#2453,.T.);
#3723=ORIENTED_EDGE('',*,*,#2452,.T.);
#3724=ORIENTED_EDGE('',*,*,#2448,.T.);
#3725=ORIENTED_EDGE('',*,*,#2518,.T.);
#3726=ORIENTED_EDGE('',*,*,#2519,.T.);
#3727=ORIENTED_EDGE('',*,*,#2520,.T.);
#3728=ORIENTED_EDGE('',*,*,#2521,.T.);
#3729=ORIENTED_EDGE('',*,*,#2522,.T.);
#3730=ORIENTED_EDGE('',*,*,#2523,.T.);
#3731=ORIENTED_EDGE('',*,*,#2516,.T.);
#3732=ORIENTED_EDGE('',*,*,#2447,.T.);
#3733=ORIENTED_EDGE('',*,*,#2513,.T.);
#3734=ORIENTED_EDGE('',*,*,#2515,.T.);
#3735=ORIENTED_EDGE('',*,*,#2482,.T.);
#3736=ORIENTED_EDGE('',*,*,#2524,.T.);
#3737=ORIENTED_EDGE('',*,*,#2525,.T.);
#3738=ORIENTED_EDGE('',*,*,#2523,.F.);
#3739=ORIENTED_EDGE('',*,*,#2526,.F.);
#3740=ORIENTED_EDGE('',*,*,#2527,.T.);
#3741=ORIENTED_EDGE('',*,*,#2526,.T.);
#3742=ORIENTED_EDGE('',*,*,#2522,.F.);
#3743=ORIENTED_EDGE('',*,*,#2528,.F.);
#3744=ORIENTED_EDGE('',*,*,#2529,.T.);
#3745=ORIENTED_EDGE('',*,*,#2528,.T.);
#3746=ORIENTED_EDGE('',*,*,#2521,.F.);
#3747=ORIENTED_EDGE('',*,*,#2530,.F.);
#3748=ORIENTED_EDGE('',*,*,#2531,.T.);
#3749=ORIENTED_EDGE('',*,*,#2530,.T.);
#3750=ORIENTED_EDGE('',*,*,#2520,.F.);
#3751=ORIENTED_EDGE('',*,*,#2532,.F.);
#3752=ORIENTED_EDGE('',*,*,#2533,.T.);
#3753=ORIENTED_EDGE('',*,*,#2532,.T.);
#3754=ORIENTED_EDGE('',*,*,#2519,.F.);
#3755=ORIENTED_EDGE('',*,*,#2534,.F.);
#3756=ORIENTED_EDGE('',*,*,#2535,.T.);
#3757=ORIENTED_EDGE('',*,*,#2534,.T.);
#3758=ORIENTED_EDGE('',*,*,#2518,.F.);
#3759=ORIENTED_EDGE('',*,*,#2525,.F.);
#3760=ORIENTED_EDGE('',*,*,#2535,.F.);
#3761=ORIENTED_EDGE('',*,*,#2524,.F.);
#3762=ORIENTED_EDGE('',*,*,#2527,.F.);
#3763=ORIENTED_EDGE('',*,*,#2529,.F.);
#3764=ORIENTED_EDGE('',*,*,#2531,.F.);
#3765=ORIENTED_EDGE('',*,*,#2533,.F.);
#3766=ORIENTED_EDGE('',*,*,#2517,.T.);
#3767=ORIENTED_EDGE('',*,*,#2504,.F.);
#3768=ORIENTED_EDGE('',*,*,#2514,.T.);
#3769=ORIENTED_EDGE('',*,*,#2477,.T.);
#3770=PLANE('',#4143);
#3771=PLANE('',#4144);
#3772=PLANE('',#4145);
#3773=PLANE('',#4146);
#3774=PLANE('',#4147);
#3775=PLANE('',#4149);
#3776=PLANE('',#4151);
#3777=PLANE('',#4153);
#3778=PLANE('',#4155);
#3779=PLANE('',#4157);
#3780=PLANE('',#4160);
#3781=PLANE('',#4161);
#3782=PLANE('',#4168);
#3783=PLANE('',#4172);
#3784=PLANE('',#4186);
#3785=PLANE('',#4191);
#3786=PLANE('',#4194);
#3787=PLANE('',#4195);
#3788=PLANE('',#4206);
#3789=PLANE('',#4209);
#3790=PLANE('',#4218);
#3791=PLANE('',#4219);
#3792=PLANE('',#4223);
#3793=PLANE('',#4227);
#3794=PLANE('',#4228);
#3795=PLANE('',#4229);
#3796=PLANE('',#4230);
#3797=PLANE('',#4232);
#3798=PLANE('',#4256);
#3799=PLANE('',#4257);
#3800=PLANE('',#4258);
#3801=PLANE('',#4259);
#3802=PLANE('',#4260);
#3803=PLANE('',#4261);
#3804=PLANE('',#4262);
#3805=PLANE('',#4263);
#3806=PLANE('',#4299);
#3807=PLANE('',#4300);
#3808=PLANE('',#4302);
#3809=PLANE('',#4309);
#3810=PLANE('',#4310);
#3811=PLANE('',#4311);
#3812=PLANE('',#4312);
#3813=PLANE('',#4313);
#3814=PLANE('',#4314);
#3815=PLANE('',#4315);
#3816=PLANE('',#4316);
#3817=PLANE('',#4374);
#3818=PLANE('',#4377);
#3819=PLANE('',#4380);
#3820=PLANE('',#4382);
#3821=PLANE('',#4422);
#3822=PLANE('',#4424);
#3823=PLANE('',#4426);
#3824=PLANE('',#4428);
#3825=PLANE('',#4429);
#3826=PLANE('',#4451);
#3827=PLANE('',#4452);
#3828=PLANE('',#4453);
#3829=PLANE('',#4454);
#3830=PLANE('',#4455);
#3831=PLANE('',#4456);
#3832=PLANE('',#4457);
#3833=PLANE('',#4458);
#3834=ADVANCED_FACE('',(#638),#3770,.F.);
#3835=ADVANCED_FACE('',(#639),#3771,.F.);
#3836=ADVANCED_FACE('',(#640),#3772,.F.);
#3837=ADVANCED_FACE('',(#641),#3773,.F.);
#3838=ADVANCED_FACE('',(#642),#3774,.F.);
#3839=ADVANCED_FACE('',(#643),#3775,.F.);
#3840=ADVANCED_FACE('',(#644),#3776,.F.);
#3841=ADVANCED_FACE('',(#645),#3777,.F.);
#3842=ADVANCED_FACE('',(#646),#3778,.F.);
#3843=ADVANCED_FACE('',(#647),#3779,.F.);
#3844=ADVANCED_FACE('',(#648),#3780,.F.);
#3845=ADVANCED_FACE('',(#649),#3781,.F.);
#3846=ADVANCED_FACE('',(#650),#500,.T.);
#3847=ADVANCED_FACE('',(#651),#396,.T.);
#3848=ADVANCED_FACE('',(#652,#379),#3782,.T.);
#3849=ADVANCED_FACE('',(#653),#501,.T.);
#3850=ADVANCED_FACE('',(#654,#380),#3783,.F.);
#3851=ADVANCED_FACE('',(#655),#502,.F.);
#3852=ADVANCED_FACE('',(#656),#397,.T.);
#3853=ADVANCED_FACE('',(#657),#85,.T.);
#3854=ADVANCED_FACE('',(#658,#381),#398,.T.);
#3855=ADVANCED_FACE('',(#659),#399,.F.);
#3856=ADVANCED_FACE('',(#660),#400,.T.);
#3857=ADVANCED_FACE('',(#661,#382),#3784,.F.);
#3858=ADVANCED_FACE('',(#662),#401,.T.);
#3859=ADVANCED_FACE('',(#663,#383),#3785,.T.);
#3860=ADVANCED_FACE('',(#664,#384),#402,.F.);
#3861=ADVANCED_FACE('',(#665,#385),#3786,.F.);
#3862=ADVANCED_FACE('',(#666,#386),#3787,.T.);
#3863=ADVANCED_FACE('',(#667),#403,.T.);
#3864=ADVANCED_FACE('',(#668),#503,.T.);
#3865=ADVANCED_FACE('',(#669),#404,.T.);
#3866=ADVANCED_FACE('',(#670),#3788,.F.);
#3867=ADVANCED_FACE('',(#671),#405,.T.);
#3868=ADVANCED_FACE('',(#672),#3789,.T.);
#3869=ADVANCED_FACE('',(#673),#406,.T.);
#3870=ADVANCED_FACE('',(#674),#504,.T.);
#3871=ADVANCED_FACE('',(#675),#407,.T.);
#3872=ADVANCED_FACE('',(#676),#3790,.T.);
#3873=ADVANCED_FACE('',(#677,#387),#3791,.T.);
#3874=ADVANCED_FACE('',(#678),#408,.F.);
#3875=ADVANCED_FACE('',(#679),#3792,.F.);
#3876=ADVANCED_FACE('',(#680),#409,.F.);
#3877=ADVANCED_FACE('',(#681),#3793,.T.);
#3878=ADVANCED_FACE('',(#682),#3794,.T.);
#3879=ADVANCED_FACE('',(#683),#3795,.T.);
#3880=ADVANCED_FACE('',(#684),#3796,.T.);
#3881=ADVANCED_FACE('',(#685),#3797,.T.);
#3882=ADVANCED_FACE('',(#686),#47,.T.);
#3883=ADVANCED_FACE('',(#687),#410,.F.);
#3884=ADVANCED_FACE('',(#688),#411,.F.);
#3885=ADVANCED_FACE('',(#689),#412,.F.);
#3886=ADVANCED_FACE('',(#690),#413,.F.);
#3887=ADVANCED_FACE('',(#691),#414,.F.);
#3888=ADVANCED_FACE('',(#692),#415,.F.);
#3889=ADVANCED_FACE('',(#693),#416,.F.);
#3890=ADVANCED_FACE('',(#694),#417,.F.);
#3891=ADVANCED_FACE('',(#695),#418,.F.);
#3892=ADVANCED_FACE('',(#696),#419,.F.);
#3893=ADVANCED_FACE('',(#697),#420,.F.);
#3894=ADVANCED_FACE('',(#698),#421,.F.);
#3895=ADVANCED_FACE('',(#699),#422,.F.);
#3896=ADVANCED_FACE('',(#700),#423,.F.);
#3897=ADVANCED_FACE('',(#701),#424,.F.);
#3898=ADVANCED_FACE('',(#702),#86,.T.);
#3899=ADVANCED_FACE('',(#703),#87,.T.);
#3900=ADVANCED_FACE('',(#704,#388),#3798,.F.);
#3901=ADVANCED_FACE('',(#705),#3799,.F.);
#3902=ADVANCED_FACE('',(#706),#3800,.F.);
#3903=ADVANCED_FACE('',(#707),#3801,.F.);
#3904=ADVANCED_FACE('',(#708),#3802,.F.);
#3905=ADVANCED_FACE('',(#709),#3803,.F.);
#3906=ADVANCED_FACE('',(#710),#3804,.F.);
#3907=ADVANCED_FACE('',(#711,#389),#3805,.T.);
#3908=ADVANCED_FACE('',(#712),#425,.T.);
#3909=ADVANCED_FACE('',(#713),#426,.T.);
#3910=ADVANCED_FACE('',(#714),#427,.T.);
#3911=ADVANCED_FACE('',(#715),#428,.T.);
#3912=ADVANCED_FACE('',(#716),#429,.T.);
#3913=ADVANCED_FACE('',(#717),#430,.T.);
#3914=ADVANCED_FACE('',(#718),#431,.T.);
#3915=ADVANCED_FACE('',(#719),#432,.T.);
#3916=ADVANCED_FACE('',(#720),#433,.T.);
#3917=ADVANCED_FACE('',(#721),#434,.T.);
#3918=ADVANCED_FACE('',(#722),#435,.T.);
#3919=ADVANCED_FACE('',(#723),#436,.T.);
#3920=ADVANCED_FACE('',(#724),#437,.T.);
#3921=ADVANCED_FACE('',(#725),#438,.T.);
#3922=ADVANCED_FACE('',(#726),#439,.T.);
#3923=ADVANCED_FACE('',(#727),#440,.T.);
#3924=ADVANCED_FACE('',(#728),#441,.T.);
#3925=ADVANCED_FACE('',(#729),#442,.T.);
#3926=ADVANCED_FACE('',(#730),#443,.T.);
#3927=ADVANCED_FACE('',(#731),#444,.T.);
#3928=ADVANCED_FACE('',(#732),#445,.T.);
#3929=ADVANCED_FACE('',(#733),#446,.T.);
#3930=ADVANCED_FACE('',(#734),#447,.T.);
#3931=ADVANCED_FACE('',(#735),#448,.T.);
#3932=ADVANCED_FACE('',(#736),#449,.T.);
#3933=ADVANCED_FACE('',(#737),#450,.T.);
#3934=ADVANCED_FACE('',(#738),#451,.T.);
#3935=ADVANCED_FACE('',(#739),#452,.T.);
#3936=ADVANCED_FACE('',(#740),#453,.T.);
#3937=ADVANCED_FACE('',(#741),#454,.T.);
#3938=ADVANCED_FACE('',(#742),#88,.F.);
#3939=ADVANCED_FACE('',(#743),#89,.F.);
#3940=ADVANCED_FACE('',(#744),#3806,.T.);
#3941=ADVANCED_FACE('',(#745),#3807,.F.);
#3942=ADVANCED_FACE('',(#746),#3808,.T.);
#3943=ADVANCED_FACE('',(#747),#48,.T.);
#3944=ADVANCED_FACE('',(#748),#455,.F.);
#3945=ADVANCED_FACE('',(#749,#390),#3809,.T.);
#3946=ADVANCED_FACE('',(#750),#3810,.T.);
#3947=ADVANCED_FACE('',(#751),#3811,.T.);
#3948=ADVANCED_FACE('',(#752),#3812,.T.);
#3949=ADVANCED_FACE('',(#753),#3813,.T.);
#3950=ADVANCED_FACE('',(#754),#3814,.T.);
#3951=ADVANCED_FACE('',(#755),#3815,.T.);
#3952=ADVANCED_FACE('',(#756,#391),#3816,.T.);
#3953=ADVANCED_FACE('',(#757),#456,.F.);
#3954=ADVANCED_FACE('',(#758),#457,.F.);
#3955=ADVANCED_FACE('',(#759),#458,.F.);
#3956=ADVANCED_FACE('',(#760),#459,.F.);
#3957=ADVANCED_FACE('',(#761),#460,.F.);
#3958=ADVANCED_FACE('',(#762),#90,.T.);
#3959=ADVANCED_FACE('',(#763),#461,.F.);
#3960=ADVANCED_FACE('',(#764),#462,.F.);
#3961=ADVANCED_FACE('',(#765),#91,.T.);
#3962=ADVANCED_FACE('',(#766),#505,.T.);
#3963=ADVANCED_FACE('',(#767),#463,.T.);
#3964=ADVANCED_FACE('',(#768),#506,.T.);
#3965=ADVANCED_FACE('',(#769),#464,.T.);
#3966=ADVANCED_FACE('',(#770),#507,.T.);
#3967=ADVANCED_FACE('',(#771),#465,.T.);
#3968=ADVANCED_FACE('',(#772),#508,.T.);
#3969=ADVANCED_FACE('',(#773),#466,.T.);
#3970=ADVANCED_FACE('',(#774),#509,.T.);
#3971=ADVANCED_FACE('',(#775),#467,.T.);
#3972=ADVANCED_FACE('',(#776),#510,.T.);
#3973=ADVANCED_FACE('',(#777),#468,.T.);
#3974=ADVANCED_FACE('',(#778),#511,.T.);
#3975=ADVANCED_FACE('',(#779),#469,.T.);
#3976=ADVANCED_FACE('',(#780),#470,.T.);
#3977=ADVANCED_FACE('',(#781),#3817,.T.);
#3978=ADVANCED_FACE('',(#782),#471,.T.);
#3979=ADVANCED_FACE('',(#783),#3818,.T.);
#3980=ADVANCED_FACE('',(#784),#3819,.T.);
#3981=ADVANCED_FACE('',(#785),#472,.T.);
#3982=ADVANCED_FACE('',(#786),#3820,.T.);
#3983=ADVANCED_FACE('',(#787),#473,.F.);
#3984=ADVANCED_FACE('',(#788),#512,.T.);
#3985=ADVANCED_FACE('',(#789),#474,.T.);
#3986=ADVANCED_FACE('',(#790),#513,.T.);
#3987=ADVANCED_FACE('',(#791),#475,.T.);
#3988=ADVANCED_FACE('',(#792),#514,.T.);
#3989=ADVANCED_FACE('',(#793),#476,.T.);
#3990=ADVANCED_FACE('',(#794),#515,.T.);
#3991=ADVANCED_FACE('',(#795),#477,.T.);
#3992=ADVANCED_FACE('',(#796),#516,.T.);
#3993=ADVANCED_FACE('',(#797),#478,.T.);
#3994=ADVANCED_FACE('',(#798),#517,.T.);
#3995=ADVANCED_FACE('',(#799),#479,.T.);
#3996=ADVANCED_FACE('',(#800),#518,.T.);
#3997=ADVANCED_FACE('',(#801),#480,.T.);
#3998=ADVANCED_FACE('',(#802),#3821,.T.);
#3999=ADVANCED_FACE('',(#803),#481,.F.);
#4000=ADVANCED_FACE('',(#804),#3822,.T.);
#4001=ADVANCED_FACE('',(#805),#482,.T.);
#4002=ADVANCED_FACE('',(#806),#3823,.T.);
#4003=ADVANCED_FACE('',(#807),#483,.T.);
#4004=ADVANCED_FACE('',(#808,#392),#3824,.T.);
#4005=ADVANCED_FACE('',(#809,#393),#3825,.T.);
#4006=ADVANCED_FACE('',(#810),#484,.F.);
#4007=ADVANCED_FACE('',(#811),#485,.F.);
#4008=ADVANCED_FACE('',(#812),#486,.F.);
#4009=ADVANCED_FACE('',(#813),#487,.F.);
#4010=ADVANCED_FACE('',(#814),#488,.F.);
#4011=ADVANCED_FACE('',(#815),#489,.F.);
#4012=ADVANCED_FACE('',(#816),#490,.F.);
#4013=ADVANCED_FACE('',(#817),#491,.F.);
#4014=ADVANCED_FACE('',(#818),#492,.F.);
#4015=ADVANCED_FACE('',(#819),#493,.F.);
#4016=ADVANCED_FACE('',(#820),#494,.F.);
#4017=ADVANCED_FACE('',(#821),#495,.F.);
#4018=ADVANCED_FACE('',(#822),#496,.F.);
#4019=ADVANCED_FACE('',(#823),#497,.F.);
#4020=ADVANCED_FACE('',(#824),#498,.F.);
#4021=ADVANCED_FACE('',(#825),#499,.F.);
#4022=ADVANCED_FACE('',(#826),#92,.F.);
#4023=ADVANCED_FACE('',(#827),#93,.F.);
#4024=ADVANCED_FACE('',(#828,#394),#3826,.T.);
#4025=ADVANCED_FACE('',(#829),#3827,.T.);
#4026=ADVANCED_FACE('',(#830),#3828,.T.);
#4027=ADVANCED_FACE('',(#831),#3829,.T.);
#4028=ADVANCED_FACE('',(#832),#3830,.T.);
#4029=ADVANCED_FACE('',(#833),#3831,.T.);
#4030=ADVANCED_FACE('',(#834),#3832,.T.);
#4031=ADVANCED_FACE('',(#835,#395),#3833,.F.);
#4032=CLOSED_SHELL('',(#3834,#3835,#3836,#3837,#3838,#3839,#3840,#3841,
#3842,#3843,#3844,#3845,#3846,#3847,#3848,#3849,#3850,#3851,#3852,#3853,
#3854,#3855,#3856,#3857,#3858,#3859,#3860,#3861,#3862));
#4033=CLOSED_SHELL('',(#3863,#3864,#3865,#3866,#3867,#3868,#3869,#3870,
#3871,#3872,#3873,#3874,#3875,#3876,#3877,#3878,#3879,#3880));
#4034=CLOSED_SHELL('',(#3881,#3882));
#4035=CLOSED_SHELL('',(#3883,#3884,#3885,#3886,#3887,#3888,#3889,#3890,
#3891,#3892,#3893,#3894,#3895,#3896,#3897,#3898,#3899,#3900,#3901,#3902,
#3903,#3904,#3905,#3906,#3907));
#4036=CLOSED_SHELL('',(#3908,#3909,#3910,#3911,#3912,#3913,#3914,#3915,
#3916,#3917,#3918,#3919,#3920,#3921,#3922,#3923,#3924,#3925,#3926,#3927,
#3928,#3929,#3930,#3931,#3932,#3933,#3934,#3935,#3936,#3937,#3938,#3939,
#3940,#3941));
#4037=CLOSED_SHELL('',(#3942,#3943));
#4038=CLOSED_SHELL('',(#3944,#3945,#3946,#3947,#3948,#3949,#3950,#3951,
#3952));
#4039=CLOSED_SHELL('',(#3953,#3954,#3955,#3956,#3957,#3958,#3959,#3960,
#3961,#3962,#3963,#3964,#3965,#3966,#3967,#3968,#3969,#3970,#3971,#3972,
#3973,#3974,#3975,#3976,#3977,#3978,#3979,#3980,#3981,#3982,#3983,#3984,
#3985,#3986,#3987,#3988,#3989,#3990,#3991,#3992,#3993,#3994,#3995,#3996,
#3997,#3998,#3999,#4000,#4001,#4002,#4003,#4004,#4005));
#4040=CLOSED_SHELL('',(#4006,#4007,#4008,#4009,#4010,#4011,#4012,#4013,
#4014,#4015,#4016,#4017,#4018,#4019,#4020,#4021,#4022,#4023,#4024,#4025,
#4026,#4027,#4028,#4029,#4030,#4031));
#4041=DERIVED_UNIT_ELEMENT(#4059,1.);
#4042=DERIVED_UNIT_ELEMENT(#42669,-3.);
#4043=DERIVED_UNIT_ELEMENT(#4059,1.);
#4044=DERIVED_UNIT_ELEMENT(#42669,-3.);
#4045=DERIVED_UNIT_ELEMENT(#4059,1.);
#4046=DERIVED_UNIT_ELEMENT(#42669,-3.);
#4047=DERIVED_UNIT_ELEMENT(#4059,1.);
#4048=DERIVED_UNIT_ELEMENT(#42669,-3.);
#4049=DERIVED_UNIT_ELEMENT(#4059,1.);
#4050=DERIVED_UNIT_ELEMENT(#42669,-3.);
#4051=DERIVED_UNIT_ELEMENT(#4059,1.);
#4052=DERIVED_UNIT_ELEMENT(#42669,-3.);
#4053=DERIVED_UNIT_ELEMENT(#4059,1.);
#4054=DERIVED_UNIT_ELEMENT(#42669,-3.);
#4055=DERIVED_UNIT_ELEMENT(#4059,1.);
#4056=DERIVED_UNIT_ELEMENT(#42669,-3.);
#4057=DERIVED_UNIT_ELEMENT(#4059,1.);
#4058=DERIVED_UNIT_ELEMENT(#42669,-3.);
#4059=(
MASS_UNIT()
NAMED_UNIT(*)
SI_UNIT(.KILO.,.GRAM.)
);
#4060=DERIVED_UNIT((#4041,#4042));
#4061=DERIVED_UNIT((#4043,#4044));
#4062=DERIVED_UNIT((#4045,#4046));
#4063=DERIVED_UNIT((#4047,#4048));
#4064=DERIVED_UNIT((#4049,#4050));
#4065=DERIVED_UNIT((#4051,#4052));
#4066=DERIVED_UNIT((#4053,#4054));
#4067=DERIVED_UNIT((#4055,#4056));
#4068=DERIVED_UNIT((#4057,#4058));
#4069=MEASURE_REPRESENTATION_ITEM('density measure',
POSITIVE_RATIO_MEASURE(7850.),#4060);
#4070=MEASURE_REPRESENTATION_ITEM('density measure',
POSITIVE_RATIO_MEASURE(7850.),#4061);
#4071=MEASURE_REPRESENTATION_ITEM('density measure',
POSITIVE_RATIO_MEASURE(7850.),#4062);
#4072=MEASURE_REPRESENTATION_ITEM('density measure',
POSITIVE_RATIO_MEASURE(7850.),#4063);
#4073=MEASURE_REPRESENTATION_ITEM('density measure',
POSITIVE_RATIO_MEASURE(7850.),#4064);
#4074=MEASURE_REPRESENTATION_ITEM('density measure',
POSITIVE_RATIO_MEASURE(7850.),#4065);
#4075=MEASURE_REPRESENTATION_ITEM('density measure',
POSITIVE_RATIO_MEASURE(7850.),#4066);
#4076=MEASURE_REPRESENTATION_ITEM('density measure',
POSITIVE_RATIO_MEASURE(7850.),#4067);
#4077=MEASURE_REPRESENTATION_ITEM('density measure',
POSITIVE_RATIO_MEASURE(7850.),#4068);
#4078=PROPERTY_DEFINITION_REPRESENTATION(#4123,#4096);
#4079=PROPERTY_DEFINITION_REPRESENTATION(#4124,#4097);
#4080=PROPERTY_DEFINITION_REPRESENTATION(#4125,#4098);
#4081=PROPERTY_DEFINITION_REPRESENTATION(#4126,#4099);
#4082=PROPERTY_DEFINITION_REPRESENTATION(#4127,#4100);
#4083=PROPERTY_DEFINITION_REPRESENTATION(#4128,#4101);
#4084=PROPERTY_DEFINITION_REPRESENTATION(#4129,#4102);
#4085=PROPERTY_DEFINITION_REPRESENTATION(#4130,#4103);
#4086=PROPERTY_DEFINITION_REPRESENTATION(#4131,#4104);
#4087=PROPERTY_DEFINITION_REPRESENTATION(#4132,#4105);
#4088=PROPERTY_DEFINITION_REPRESENTATION(#4133,#4106);
#4089=PROPERTY_DEFINITION_REPRESENTATION(#4134,#4107);
#4090=PROPERTY_DEFINITION_REPRESENTATION(#4135,#4108);
#4091=PROPERTY_DEFINITION_REPRESENTATION(#4136,#4109);
#4092=PROPERTY_DEFINITION_REPRESENTATION(#4137,#4110);
#4093=PROPERTY_DEFINITION_REPRESENTATION(#4138,#4111);
#4094=PROPERTY_DEFINITION_REPRESENTATION(#4139,#4112);
#4095=PROPERTY_DEFINITION_REPRESENTATION(#4140,#4113);
#4096=REPRESENTATION('material name',(#4114),#42658);
#4097=REPRESENTATION('density',(#4069),#42658);
#4098=REPRESENTATION('material name',(#4115),#42659);
#4099=REPRESENTATION('density',(#4070),#42659);
#4100=REPRESENTATION('material name',(#4116),#42660);
#4101=REPRESENTATION('density',(#4071),#42660);
#4102=REPRESENTATION('material name',(#4117),#42661);
#4103=REPRESENTATION('density',(#4072),#42661);
#4104=REPRESENTATION('material name',(#4118),#42662);
#4105=REPRESENTATION('density',(#4073),#42662);
#4106=REPRESENTATION('material name',(#4119),#42663);
#4107=REPRESENTATION('density',(#4074),#42663);
#4108=REPRESENTATION('material name',(#4120),#42664);
#4109=REPRESENTATION('density',(#4075),#42664);
#4110=REPRESENTATION('material name',(#4121),#42665);
#4111=REPRESENTATION('density',(#4076),#42665);
#4112=REPRESENTATION('material name',(#4122),#42666);
#4113=REPRESENTATION('density',(#4077),#42666);
#4114=DESCRIPTIVE_REPRESENTATION_ITEM('Steel','Steel');
#4115=DESCRIPTIVE_REPRESENTATION_ITEM('Steel','Steel');
#4116=DESCRIPTIVE_REPRESENTATION_ITEM('Steel','Steel');
#4117=DESCRIPTIVE_REPRESENTATION_ITEM('Steel','Steel');
#4118=DESCRIPTIVE_REPRESENTATION_ITEM('Steel','Steel');
#4119=DESCRIPTIVE_REPRESENTATION_ITEM('Steel','Steel');
#4120=DESCRIPTIVE_REPRESENTATION_ITEM('Steel','Steel');
#4121=DESCRIPTIVE_REPRESENTATION_ITEM('Steel','Steel');
#4122=DESCRIPTIVE_REPRESENTATION_ITEM('Steel','Steel');
#4123=PROPERTY_DEFINITION('material property','material name',#42713);
#4124=PROPERTY_DEFINITION('material property','density of part',#42713);
#4125=PROPERTY_DEFINITION('material property','material name',#42714);
#4126=PROPERTY_DEFINITION('material property','density of part',#42714);
#4127=PROPERTY_DEFINITION('material property','material name',#42715);
#4128=PROPERTY_DEFINITION('material property','density of part',#42715);
#4129=PROPERTY_DEFINITION('material property','material name',#42716);
#4130=PROPERTY_DEFINITION('material property','density of part',#42716);
#4131=PROPERTY_DEFINITION('material property','material name',#42717);
#4132=PROPERTY_DEFINITION('material property','density of part',#42717);
#4133=PROPERTY_DEFINITION('material property','material name',#42718);
#4134=PROPERTY_DEFINITION('material property','density of part',#42718);
#4135=PROPERTY_DEFINITION('material property','material name',#42719);
#4136=PROPERTY_DEFINITION('material property','density of part',#42719);
#4137=PROPERTY_DEFINITION('material property','material name',#42720);
#4138=PROPERTY_DEFINITION('material property','density of part',#42720);
#4139=PROPERTY_DEFINITION('material property','material name',#42721);
#4140=PROPERTY_DEFINITION('material property','density of part',#42721);
#4141=AXIS2_PLACEMENT_3D('',#5335,#4468,#4469);
#4142=AXIS2_PLACEMENT_3D('',#5336,#4470,#4471);
#4143=AXIS2_PLACEMENT_3D('',#5337,#4472,#4473);
#4144=AXIS2_PLACEMENT_3D('',#5348,#4479,#4480);
#4145=AXIS2_PLACEMENT_3D('',#5356,#4485,#4486);
#4146=AXIS2_PLACEMENT_3D('',#5364,#4491,#4492);
#4147=AXIS2_PLACEMENT_3D('',#5372,#4497,#4498);
#4148=AXIS2_PLACEMENT_3D('',#5375,#4499,#4500);
#4149=AXIS2_PLACEMENT_3D('',#5379,#4503,#4504);
#4150=AXIS2_PLACEMENT_3D('',#5380,#4505,#4506);
#4151=AXIS2_PLACEMENT_3D('',#5382,#4508,#4509);
#4152=AXIS2_PLACEMENT_3D('',#5383,#4510,#4511);
#4153=AXIS2_PLACEMENT_3D('',#5384,#4512,#4513);
#4154=AXIS2_PLACEMENT_3D('',#5385,#4514,#4515);
#4155=AXIS2_PLACEMENT_3D('',#5386,#4516,#4517);
#4156=AXIS2_PLACEMENT_3D('',#5387,#4518,#4519);
#4157=AXIS2_PLACEMENT_3D('',#5388,#4520,#4521);
#4158=AXIS2_PLACEMENT_3D('',#5390,#4522,#4523);
#4159=AXIS2_PLACEMENT_3D('',#5392,#4525,#4526);
#4160=AXIS2_PLACEMENT_3D('',#5393,#4527,#4528);
#4161=AXIS2_PLACEMENT_3D('',#5397,#4531,#4532);
#4162=AXIS2_PLACEMENT_3D('',#5399,#4534,#4535);
#4163=AXIS2_PLACEMENT_3D('',#5401,#4536,#4537);
#4164=AXIS2_PLACEMENT_3D('',#5403,#4538,#4539);
#4165=AXIS2_PLACEMENT_3D('',#5404,#4540,#4541);
#4166=AXIS2_PLACEMENT_3D('',#5405,#4542,#4543);
#4167=AXIS2_PLACEMENT_3D('',#5408,#4545,#4546);
#4168=AXIS2_PLACEMENT_3D('',#5409,#4547,#4548);
#4169=AXIS2_PLACEMENT_3D('',#5410,#4549,#4550);
#4170=AXIS2_PLACEMENT_3D('',#5412,#4551,#4552);
#4171=AXIS2_PLACEMENT_3D('',#5413,#4553,#4554);
#4172=AXIS2_PLACEMENT_3D('',#5414,#4555,#4556);
#4173=AXIS2_PLACEMENT_3D('',#5416,#4557,#4558);
#4174=AXIS2_PLACEMENT_3D('',#5417,#4559,#4560);
#4175=AXIS2_PLACEMENT_3D('',#5420,#4561,#4562);
#4176=AXIS2_PLACEMENT_3D('',#5421,#4563,#4564);
#4177=AXIS2_PLACEMENT_3D('',#5422,#4565,#4566);
#4178=AXIS2_PLACEMENT_3D('',#5423,#4567,#4568);
#4179=AXIS2_PLACEMENT_3D('',#5792,#4570,#4571);
#4180=AXIS2_PLACEMENT_3D('',#5794,#4572,#4573);
#4181=AXIS2_PLACEMENT_3D('',#5797,#4575,#4576);
#4182=AXIS2_PLACEMENT_3D('',#5798,#4577,#4578);
#4183=AXIS2_PLACEMENT_3D('',#5838,#4580,#4581);
#4184=AXIS2_PLACEMENT_3D('',#5840,#4582,#4583);
#4185=AXIS2_PLACEMENT_3D('',#5843,#4585,#4586);
#4186=AXIS2_PLACEMENT_3D('',#5844,#4587,#4588);
#4187=AXIS2_PLACEMENT_3D('',#5846,#4589,#4590);
#4188=AXIS2_PLACEMENT_3D('',#5847,#4591,#4592);
#4189=AXIS2_PLACEMENT_3D('',#5849,#4593,#4594);
#4190=AXIS2_PLACEMENT_3D('',#5852,#4596,#4597);
#4191=AXIS2_PLACEMENT_3D('',#5853,#4598,#4599);
#4192=AXIS2_PLACEMENT_3D('',#5855,#4600,#4601);
#4193=AXIS2_PLACEMENT_3D('',#5856,#4602,#4603);
#4194=AXIS2_PLACEMENT_3D('',#5858,#4605,#4606);
#4195=AXIS2_PLACEMENT_3D('',#5859,#4607,#4608);
#4196=AXIS2_PLACEMENT_3D('',#5860,#4609,#4610);
#4197=AXIS2_PLACEMENT_3D('',#5861,#4611,#4612);
#4198=AXIS2_PLACEMENT_3D('',#5864,#4613,#4614);
#4199=AXIS2_PLACEMENT_3D('',#5868,#4616,#4617);
#4200=AXIS2_PLACEMENT_3D('',#5870,#4619,#4620);
#4201=AXIS2_PLACEMENT_3D('',#5873,#4621,#4622);
#4202=AXIS2_PLACEMENT_3D('',#5874,#4623,#4624);
#4203=AXIS2_PLACEMENT_3D('',#5875,#4625,#4626);
#4204=AXIS2_PLACEMENT_3D('',#5876,#4627,#4628);
#4205=AXIS2_PLACEMENT_3D('',#5879,#4629,#4630);
#4206=AXIS2_PLACEMENT_3D('',#5882,#4633,#4634);
#4207=AXIS2_PLACEMENT_3D('',#5888,#4638,#4639);
#4208=AXIS2_PLACEMENT_3D('',#5891,#4641,#4642);
#4209=AXIS2_PLACEMENT_3D('',#5892,#4643,#4644);
#4210=AXIS2_PLACEMENT_3D('',#5896,#4647,#4648);
#4211=AXIS2_PLACEMENT_3D('',#5898,#4649,#4650);
#4212=AXIS2_PLACEMENT_3D('',#5901,#4652,#4653);
#4213=AXIS2_PLACEMENT_3D('',#5902,#4654,#4655);
#4214=AXIS2_PLACEMENT_3D('',#5904,#4656,#4657);
#4215=AXIS2_PLACEMENT_3D('',#5905,#4658,#4659);
#4216=AXIS2_PLACEMENT_3D('',#5906,#4660,#4661);
#4217=AXIS2_PLACEMENT_3D('',#5908,#4662,#4663);
#4218=AXIS2_PLACEMENT_3D('',#5910,#4665,#4666);
#4219=AXIS2_PLACEMENT_3D('',#5912,#4668,#4669);
#4220=AXIS2_PLACEMENT_3D('',#5922,#4675,#4676);
#4221=AXIS2_PLACEMENT_3D('',#5925,#4677,#4678);
#4222=AXIS2_PLACEMENT_3D('',#5929,#4680,#4681);
#4223=AXIS2_PLACEMENT_3D('',#5931,#4683,#4684);
#4224=AXIS2_PLACEMENT_3D('',#5934,#4687,#4688);
#4225=AXIS2_PLACEMENT_3D('',#5936,#4689,#4690);
#4226=AXIS2_PLACEMENT_3D('',#5939,#4692,#4693);
#4227=AXIS2_PLACEMENT_3D('',#5940,#4694,#4695);
#4228=AXIS2_PLACEMENT_3D('',#5942,#4697,#4698);
#4229=AXIS2_PLACEMENT_3D('',#5944,#4700,#4701);
#4230=AXIS2_PLACEMENT_3D('',#5945,#4702,#4703);
#4231=AXIS2_PLACEMENT_3D('',#5946,#4704,#4705);
#4232=AXIS2_PLACEMENT_3D('',#5947,#4706,#4707);
#4233=AXIS2_PLACEMENT_3D('',#5949,#4708,#4709);
#4234=AXIS2_PLACEMENT_3D('',#5950,#4710,#4711);
#4235=AXIS2_PLACEMENT_3D('',#5951,#4712,#4713);
#4236=AXIS2_PLACEMENT_3D('',#5952,#4714,#4715);
#4237=AXIS2_PLACEMENT_3D('',#5964,#4717,#4718);
#4238=AXIS2_PLACEMENT_3D('',#5965,#4719,#4720);
#4239=AXIS2_PLACEMENT_3D('',#6243,#4722,#4723);
#4240=AXIS2_PLACEMENT_3D('',#6264,#4724,#4725);
#4241=AXIS2_PLACEMENT_3D('',#6746,#4727,#4728);
#4242=AXIS2_PLACEMENT_3D('',#7296,#4730,#4731);
#4243=AXIS2_PLACEMENT_3D('',#7663,#4733,#4734);
#4244=AXIS2_PLACEMENT_3D('',#8145,#4736,#4737);
#4245=AXIS2_PLACEMENT_3D('',#8695,#4739,#4740);
#4246=AXIS2_PLACEMENT_3D('',#8944,#4742,#4743);
#4247=AXIS2_PLACEMENT_3D('',#9015,#4744,#4745);
#4248=AXIS2_PLACEMENT_3D('',#9146,#4747,#4748);
#4249=AXIS2_PLACEMENT_3D('',#9348,#4750,#4751);
#4250=AXIS2_PLACEMENT_3D('',#9545,#4753,#4754);
#4251=AXIS2_PLACEMENT_3D('',#9751,#4756,#4757);
#4252=AXIS2_PLACEMENT_3D('',#9964,#4759,#4760);
#4253=AXIS2_PLACEMENT_3D('',#10063,#4761,#4762);
#4254=AXIS2_PLACEMENT_3D('',#10257,#4763,#4764);
#4255=AXIS2_PLACEMENT_3D('',#10346,#4765,#4766);
#4256=AXIS2_PLACEMENT_3D('',#11637,#4767,#4768);
#4257=AXIS2_PLACEMENT_3D('',#11650,#4775,#4776);
#4258=AXIS2_PLACEMENT_3D('',#11656,#4780,#4781);
#4259=AXIS2_PLACEMENT_3D('',#11660,#4784,#4785);
#4260=AXIS2_PLACEMENT_3D('',#11664,#4788,#4789);
#4261=AXIS2_PLACEMENT_3D('',#11668,#4792,#4793);
#4262=AXIS2_PLACEMENT_3D('',#11672,#4796,#4797);
#4263=AXIS2_PLACEMENT_3D('',#11674,#4799,#4800);
#4264=AXIS2_PLACEMENT_3D('',#11675,#4801,#4802);
#4265=AXIS2_PLACEMENT_3D('',#11676,#4803,#4804);
#4266=AXIS2_PLACEMENT_3D('',#11794,#4806,#4807);
#4267=AXIS2_PLACEMENT_3D('',#11865,#4808,#4809);
#4268=AXIS2_PLACEMENT_3D('',#12370,#4811,#4812);
#4269=AXIS2_PLACEMENT_3D('',#12812,#4814,#4815);
#4270=AXIS2_PLACEMENT_3D('',#13200,#4817,#4818);
#4271=AXIS2_PLACEMENT_3D('',#13593,#4820,#4821);
#4272=AXIS2_PLACEMENT_3D('',#14070,#4823,#4824);
#4273=AXIS2_PLACEMENT_3D('',#14565,#4826,#4827);
#4274=AXIS2_PLACEMENT_3D('',#15042,#4829,#4830);
#4275=AXIS2_PLACEMENT_3D('',#15531,#4832,#4833);
#4276=AXIS2_PLACEMENT_3D('',#15988,#4835,#4836);
#4277=AXIS2_PLACEMENT_3D('',#16529,#4838,#4839);
#4278=AXIS2_PLACEMENT_3D('',#16846,#4841,#4842);
#4279=AXIS2_PLACEMENT_3D('',#17274,#4844,#4845);
#4280=AXIS2_PLACEMENT_3D('',#17728,#4847,#4848);
#4281=AXIS2_PLACEMENT_3D('',#18216,#4850,#4851);
#4282=AXIS2_PLACEMENT_3D('',#18660,#4853,#4854);
#4283=AXIS2_PLACEMENT_3D('',#19056,#4856,#4857);
#4284=AXIS2_PLACEMENT_3D('',#19481,#4859,#4860);
#4285=AXIS2_PLACEMENT_3D('',#19942,#4862,#4863);
#4286=AXIS2_PLACEMENT_3D('',#20391,#4865,#4866);
#4287=AXIS2_PLACEMENT_3D('',#20860,#4868,#4869);
#4288=AXIS2_PLACEMENT_3D('',#21305,#4871,#4872);
#4289=AXIS2_PLACEMENT_3D('',#21806,#4874,#4875);
#4290=AXIS2_PLACEMENT_3D('',#22265,#4877,#4878);
#4291=AXIS2_PLACEMENT_3D('',#22567,#4880,#4881);
#4292=AXIS2_PLACEMENT_3D('',#22983,#4883,#4884);
#4293=AXIS2_PLACEMENT_3D('',#23421,#4886,#4887);
#4294=AXIS2_PLACEMENT_3D('',#23919,#4889,#4890);
#4295=AXIS2_PLACEMENT_3D('',#23996,#4891,#4892);
#4296=AXIS2_PLACEMENT_3D('',#27732,#4893,#4894);
#4297=AXIS2_PLACEMENT_3D('',#31498,#4895,#4896);
#4298=AXIS2_PLACEMENT_3D('',#31645,#4897,#4898);
#4299=AXIS2_PLACEMENT_3D('',#33568,#4899,#4900);
#4300=AXIS2_PLACEMENT_3D('',#33569,#4901,#4902);
#4301=AXIS2_PLACEMENT_3D('',#33570,#4903,#4904);
#4302=AXIS2_PLACEMENT_3D('',#33571,#4905,#4906);
#4303=AXIS2_PLACEMENT_3D('',#33573,#4907,#4908);
#4304=AXIS2_PLACEMENT_3D('',#33574,#4909,#4910);
#4305=AXIS2_PLACEMENT_3D('',#33575,#4911,#4912);
#4306=AXIS2_PLACEMENT_3D('',#33576,#4913,#4914);
#4307=AXIS2_PLACEMENT_3D('',#33578,#4915,#4916);
#4308=AXIS2_PLACEMENT_3D('',#33581,#4918,#4919);
#4309=AXIS2_PLACEMENT_3D('',#33582,#4920,#4921);
#4310=AXIS2_PLACEMENT_3D('',#33595,#4928,#4929);
#4311=AXIS2_PLACEMENT_3D('',#33601,#4933,#4934);
#4312=AXIS2_PLACEMENT_3D('',#33605,#4937,#4938);
#4313=AXIS2_PLACEMENT_3D('',#33609,#4941,#4942);
#4314=AXIS2_PLACEMENT_3D('',#33613,#4945,#4946);
#4315=AXIS2_PLACEMENT_3D('',#33617,#4949,#4950);
#4316=AXIS2_PLACEMENT_3D('',#33619,#4952,#4953);
#4317=AXIS2_PLACEMENT_3D('',#33620,#4954,#4955);
#4318=AXIS2_PLACEMENT_3D('',#33621,#4956,#4957);
#4319=AXIS2_PLACEMENT_3D('',#33733,#4959,#4960);
#4320=AXIS2_PLACEMENT_3D('',#33876,#4961,#4962);
#4321=AXIS2_PLACEMENT_3D('',#34057,#4964,#4965);
#4322=AXIS2_PLACEMENT_3D('',#34269,#4966,#4967);
#4323=AXIS2_PLACEMENT_3D('',#34280,#4969,#4970);
#4324=AXIS2_PLACEMENT_3D('',#34410,#4971,#4972);
#4325=AXIS2_PLACEMENT_3D('',#34712,#4974,#4975);
#4326=AXIS2_PLACEMENT_3D('',#34717,#4977,#4978);
#4327=AXIS2_PLACEMENT_3D('',#35730,#4979,#4980);
#4328=AXIS2_PLACEMENT_3D('',#35955,#4981,#4982);
#4329=AXIS2_PLACEMENT_3D('',#35956,#4983,#4984);
#4330=AXIS2_PLACEMENT_3D('',#36719,#4985,#4986);
#4331=AXIS2_PLACEMENT_3D('',#36722,#4987,#4988);
#4332=AXIS2_PLACEMENT_3D('',#36724,#4989,#4990);
#4333=AXIS2_PLACEMENT_3D('',#36726,#4991,#4992);
#4334=AXIS2_PLACEMENT_3D('',#36727,#4993,#4994);
#4335=AXIS2_PLACEMENT_3D('',#36728,#4995,#4996);
#4336=AXIS2_PLACEMENT_3D('',#36731,#4997,#4998);
#4337=AXIS2_PLACEMENT_3D('',#36734,#5001,#5002);
#4338=AXIS2_PLACEMENT_3D('',#36737,#5003,#5004);
#4339=AXIS2_PLACEMENT_3D('',#36738,#5005,#5006);
#4340=AXIS2_PLACEMENT_3D('',#36739,#5007,#5008);
#4341=AXIS2_PLACEMENT_3D('',#36740,#5009,#5010);
#4342=AXIS2_PLACEMENT_3D('',#36743,#5011,#5012);
#4343=AXIS2_PLACEMENT_3D('',#36746,#5015,#5016);
#4344=AXIS2_PLACEMENT_3D('',#36749,#5017,#5018);
#4345=AXIS2_PLACEMENT_3D('',#36750,#5019,#5020);
#4346=AXIS2_PLACEMENT_3D('',#36751,#5021,#5022);
#4347=AXIS2_PLACEMENT_3D('',#36752,#5023,#5024);
#4348=AXIS2_PLACEMENT_3D('',#36755,#5025,#5026);
#4349=AXIS2_PLACEMENT_3D('',#36758,#5029,#5030);
#4350=AXIS2_PLACEMENT_3D('',#36761,#5031,#5032);
#4351=AXIS2_PLACEMENT_3D('',#36762,#5033,#5034);
#4352=AXIS2_PLACEMENT_3D('',#36763,#5035,#5036);
#4353=AXIS2_PLACEMENT_3D('',#36764,#5037,#5038);
#4354=AXIS2_PLACEMENT_3D('',#36767,#5039,#5040);
#4355=AXIS2_PLACEMENT_3D('',#36770,#5043,#5044);
#4356=AXIS2_PLACEMENT_3D('',#36773,#5045,#5046);
#4357=AXIS2_PLACEMENT_3D('',#36774,#5047,#5048);
#4358=AXIS2_PLACEMENT_3D('',#36775,#5049,#5050);
#4359=AXIS2_PLACEMENT_3D('',#36776,#5051,#5052);
#4360=AXIS2_PLACEMENT_3D('',#36779,#5053,#5054);
#4361=AXIS2_PLACEMENT_3D('',#36782,#5057,#5058);
#4362=AXIS2_PLACEMENT_3D('',#36785,#5059,#5060);
#4363=AXIS2_PLACEMENT_3D('',#36786,#5061,#5062);
#4364=AXIS2_PLACEMENT_3D('',#36787,#5063,#5064);
#4365=AXIS2_PLACEMENT_3D('',#36788,#5065,#5066);
#4366=AXIS2_PLACEMENT_3D('',#36791,#5067,#5068);
#4367=AXIS2_PLACEMENT_3D('',#36794,#5071,#5072);
#4368=AXIS2_PLACEMENT_3D('',#36797,#5073,#5074);
#4369=AXIS2_PLACEMENT_3D('',#36798,#5075,#5076);
#4370=AXIS2_PLACEMENT_3D('',#36799,#5077,#5078);
#4371=AXIS2_PLACEMENT_3D('',#36800,#5079,#5080);
#4372=AXIS2_PLACEMENT_3D('',#36803,#5083,#5084);
#4373=AXIS2_PLACEMENT_3D('',#36807,#5086,#5087);
#4374=AXIS2_PLACEMENT_3D('',#36809,#5089,#5090);
#4375=AXIS2_PLACEMENT_3D('',#36813,#5093,#5094);
#4376=AXIS2_PLACEMENT_3D('',#36816,#5096,#5097);
#4377=AXIS2_PLACEMENT_3D('',#36817,#5098,#5099);
#4378=AXIS2_PLACEMENT_3D('',#36823,#5102,#5103);
#4379=AXIS2_PLACEMENT_3D('',#36827,#5105,#5106);
#4380=AXIS2_PLACEMENT_3D('',#36829,#5108,#5109);
#4381=AXIS2_PLACEMENT_3D('',#36831,#5111,#5112);
#4382=AXIS2_PLACEMENT_3D('',#36834,#5115,#5116);
#4383=AXIS2_PLACEMENT_3D('',#36836,#5118,#5119);
#4384=AXIS2_PLACEMENT_3D('',#36837,#5120,#5121);
#4385=AXIS2_PLACEMENT_3D('',#36840,#5122,#5123);
#4386=AXIS2_PLACEMENT_3D('',#36842,#5124,#5125);
#4387=AXIS2_PLACEMENT_3D('',#36844,#5126,#5127);
#4388=AXIS2_PLACEMENT_3D('',#36845,#5128,#5129);
#4389=AXIS2_PLACEMENT_3D('',#36846,#5130,#5131);
#4390=AXIS2_PLACEMENT_3D('',#36849,#5132,#5133);
#4391=AXIS2_PLACEMENT_3D('',#36852,#5136,#5137);
#4392=AXIS2_PLACEMENT_3D('',#36855,#5138,#5139);
#4393=AXIS2_PLACEMENT_3D('',#36856,#5140,#5141);
#4394=AXIS2_PLACEMENT_3D('',#36857,#5142,#5143);
#4395=AXIS2_PLACEMENT_3D('',#36858,#5144,#5145);
#4396=AXIS2_PLACEMENT_3D('',#36860,#5146,#5147);
#4397=AXIS2_PLACEMENT_3D('',#36863,#5150,#5151);
#4398=AXIS2_PLACEMENT_3D('',#36865,#5152,#5153);
#4399=AXIS2_PLACEMENT_3D('',#36866,#5154,#5155);
#4400=AXIS2_PLACEMENT_3D('',#36867,#5156,#5157);
#4401=AXIS2_PLACEMENT_3D('',#36869,#5158,#5159);
#4402=AXIS2_PLACEMENT_3D('',#36871,#5161,#5162);
#4403=AXIS2_PLACEMENT_3D('',#36873,#5163,#5164);
#4404=AXIS2_PLACEMENT_3D('',#36874,#5165,#5166);
#4405=AXIS2_PLACEMENT_3D('',#36875,#5167,#5168);
#4406=AXIS2_PLACEMENT_3D('',#36877,#5169,#5170);
#4407=AXIS2_PLACEMENT_3D('',#36879,#5172,#5173);
#4408=AXIS2_PLACEMENT_3D('',#36881,#5174,#5175);
#4409=AXIS2_PLACEMENT_3D('',#36882,#5176,#5177);
#4410=AXIS2_PLACEMENT_3D('',#36883,#5178,#5179);
#4411=AXIS2_PLACEMENT_3D('',#36885,#5180,#5181);
#4412=AXIS2_PLACEMENT_3D('',#36887,#5183,#5184);
#4413=AXIS2_PLACEMENT_3D('',#36889,#5185,#5186);
#4414=AXIS2_PLACEMENT_3D('',#36890,#5187,#5188);
#4415=AXIS2_PLACEMENT_3D('',#36891,#5189,#5190);
#4416=AXIS2_PLACEMENT_3D('',#36893,#5191,#5192);
#4417=AXIS2_PLACEMENT_3D('',#36895,#5194,#5195);
#4418=AXIS2_PLACEMENT_3D('',#36898,#5196,#5197);
#4419=AXIS2_PLACEMENT_3D('',#36899,#5198,#5199);
#4420=AXIS2_PLACEMENT_3D('',#36900,#5200,#5201);
#4421=AXIS2_PLACEMENT_3D('',#36901,#5202,#5203);
#4422=AXIS2_PLACEMENT_3D('',#36904,#5206,#5207);
#4423=AXIS2_PLACEMENT_3D('',#36906,#5209,#5210);
#4424=AXIS2_PLACEMENT_3D('',#36909,#5213,#5214);
#4425=AXIS2_PLACEMENT_3D('',#36911,#5216,#5217);
#4426=AXIS2_PLACEMENT_3D('',#36912,#5218,#5219);
#4427=AXIS2_PLACEMENT_3D('',#36914,#5221,#5222);
#4428=AXIS2_PLACEMENT_3D('',#36915,#5223,#5224);
#4429=AXIS2_PLACEMENT_3D('',#36916,#5225,#5226);
#4430=AXIS2_PLACEMENT_3D('',#36917,#5227,#5228);
#4431=AXIS2_PLACEMENT_3D('',#36918,#5229,#5230);
#4432=AXIS2_PLACEMENT_3D('',#36928,#5232,#5233);
#4433=AXIS2_PLACEMENT_3D('',#36934,#5234,#5235);
#4434=AXIS2_PLACEMENT_3D('',#37303,#5237,#5238);
#4435=AXIS2_PLACEMENT_3D('',#37850,#5240,#5241);
#4436=AXIS2_PLACEMENT_3D('',#38238,#5243,#5244);
#4437=AXIS2_PLACEMENT_3D('',#38699,#5246,#5247);
#4438=AXIS2_PLACEMENT_3D('',#39249,#5249,#5250);
#4439=AXIS2_PLACEMENT_3D('',#39271,#5252,#5253);
#4440=AXIS2_PLACEMENT_3D('',#39452,#5254,#5255);
#4441=AXIS2_PLACEMENT_3D('',#39528,#5257,#5258);
#4442=AXIS2_PLACEMENT_3D('',#39581,#5259,#5260);
#4443=AXIS2_PLACEMENT_3D('',#39840,#5262,#5263);
#4444=AXIS2_PLACEMENT_3D('',#39996,#5265,#5266);
#4445=AXIS2_PLACEMENT_3D('',#40200,#5268,#5269);
#4446=AXIS2_PLACEMENT_3D('',#40399,#5271,#5272);
#4447=AXIS2_PLACEMENT_3D('',#40595,#5274,#5275);
#4448=AXIS2_PLACEMENT_3D('',#40615,#5277,#5278);
#4449=AXIS2_PLACEMENT_3D('',#40728,#5279,#5280);
#4450=AXIS2_PLACEMENT_3D('',#41007,#5281,#5282);
#4451=AXIS2_PLACEMENT_3D('',#42599,#5283,#5284);
#4452=AXIS2_PLACEMENT_3D('',#42612,#5291,#5292);
#4453=AXIS2_PLACEMENT_3D('',#42618,#5296,#5297);
#4454=AXIS2_PLACEMENT_3D('',#42622,#5300,#5301);
#4455=AXIS2_PLACEMENT_3D('',#42626,#5304,#5305);
#4456=AXIS2_PLACEMENT_3D('',#42630,#5308,#5309);
#4457=AXIS2_PLACEMENT_3D('',#42634,#5312,#5313);
#4458=AXIS2_PLACEMENT_3D('',#42636,#5315,#5316);
#4459=AXIS2_PLACEMENT_3D('',#42637,#5317,#5318);
#4460=AXIS2_PLACEMENT_3D('',#42638,#5319,#5320);
#4461=AXIS2_PLACEMENT_3D('',#42639,#5321,#5322);
#4462=AXIS2_PLACEMENT_3D('',#42640,#5323,#5324);
#4463=AXIS2_PLACEMENT_3D('',#42641,#5325,#5326);
#4464=AXIS2_PLACEMENT_3D('',#42642,#5327,#5328);
#4465=AXIS2_PLACEMENT_3D('',#42643,#5329,#5330);
#4466=AXIS2_PLACEMENT_3D('',#42644,#5331,#5332);
#4467=AXIS2_PLACEMENT_3D('',#42645,#5333,#5334);
#4468=DIRECTION('axis',(0.,0.,1.));
#4469=DIRECTION('refdir',(1.,0.,0.));
#4470=DIRECTION('axis',(0.,0.,1.));
#4471=DIRECTION('refdir',(1.,0.,0.));
#4472=DIRECTION('center_axis',(0.866025403784439,0.5,0.));
#4473=DIRECTION('ref_axis',(0.5,-0.866025403784439,0.));
#4474=DIRECTION('',(0.5,-0.866025403784439,0.));
#4475=DIRECTION('',(0.,0.,1.));
#4476=DIRECTION('',(0.5,-0.866025403784439,0.));
#4477=DIRECTION('',(0.5,-0.866025403784439,0.));
#4478=DIRECTION('',(0.,0.,1.));
#4479=DIRECTION('center_axis',(3.20493781063927E-16,1.,0.));
#4480=DIRECTION('ref_axis',(1.,-3.20493781063927E-16,0.));
#4481=DIRECTION('',(1.,-3.20493781063927E-16,0.));
#4482=DIRECTION('',(0.,0.,1.));
#4483=DIRECTION('',(1.,-3.20493781063927E-16,0.));
#4484=DIRECTION('',(1.,-3.20493781063927E-16,0.));
#4485=DIRECTION('center_axis',(0.866025403784439,-0.5,0.));
#4486=DIRECTION('ref_axis',(-0.5,-0.866025403784439,0.));
#4487=DIRECTION('',(-0.5,-0.866025403784439,0.));
#4488=DIRECTION('',(-0.5,-0.866025403784439,0.));
#4489=DIRECTION('',(-0.5,-0.866025403784439,0.));
#4490=DIRECTION('',(0.,0.,1.));
#4491=DIRECTION('center_axis',(-0.866025403784438,0.5,0.));
#4492=DIRECTION('ref_axis',(0.5,0.866025403784438,0.));
#4493=DIRECTION('',(0.5,0.866025403784439,0.));
#4494=DIRECTION('',(0.,0.,1.));
#4495=DIRECTION('',(0.5,0.866025403784439,0.));
#4496=DIRECTION('',(0.5,0.866025403784439,0.));
#4497=DIRECTION('center_axis',(0.,0.,-1.));
#4498=DIRECTION('ref_axis',(-1.,0.,0.));
#4499=DIRECTION('center_axis',(0.,0.,1.));
#4500=DIRECTION('ref_axis',(1.,0.,0.));
#4501=DIRECTION('',(-0.499999999999999,0.866025403784439,0.));
#4502=DIRECTION('',(-1.,6.40987562127854E-16,0.));
#4503=DIRECTION('center_axis',(0.,0.,-1.));
#4504=DIRECTION('ref_axis',(-1.,0.,0.));
#4505=DIRECTION('center_axis',(0.,0.,1.));
#4506=DIRECTION('ref_axis',(1.,0.,0.));
#4507=DIRECTION('',(-1.,6.40987562127854E-16,0.));
#4508=DIRECTION('center_axis',(0.,0.,-1.));
#4509=DIRECTION('ref_axis',(-1.,0.,0.));
#4510=DIRECTION('center_axis',(0.,0.,1.));
#4511=DIRECTION('ref_axis',(1.,0.,0.));
#4512=DIRECTION('center_axis',(0.,0.,-1.));
#4513=DIRECTION('ref_axis',(-1.,0.,0.));
#4514=DIRECTION('center_axis',(0.,0.,1.));
#4515=DIRECTION('ref_axis',(1.,0.,0.));
#4516=DIRECTION('center_axis',(0.,0.,-1.));
#4517=DIRECTION('ref_axis',(-1.,0.,0.));
#4518=DIRECTION('center_axis',(0.,0.,1.));
#4519=DIRECTION('ref_axis',(1.,0.,0.));
#4520=DIRECTION('center_axis',(0.,0.,-1.));
#4521=DIRECTION('ref_axis',(-1.,0.,0.));
#4522=DIRECTION('center_axis',(0.,0.,1.));
#4523=DIRECTION('ref_axis',(1.,0.,0.));
#4524=DIRECTION('',(-0.499999999999999,0.866025403784439,0.));
#4525=DIRECTION('center_axis',(0.,0.,1.));
#4526=DIRECTION('ref_axis',(1.,0.,0.));
#4527=DIRECTION('center_axis',(-6.40987562127854E-16,-1.,0.));
#4528=DIRECTION('ref_axis',(-1.,6.40987562127854E-16,0.));
#4529=DIRECTION('',(-1.,6.40987562127854E-16,0.));
#4530=DIRECTION('',(0.,0.,-1.));
#4531=DIRECTION('center_axis',(-0.866025403784439,-0.5,0.));
#4532=DIRECTION('ref_axis',(-0.5,0.866025403784439,0.));
#4533=DIRECTION('',(-0.499999999999999,0.866025403784439,0.));
#4534=DIRECTION('center_axis',(0.,0.,1.));
#4535=DIRECTION('ref_axis',(1.,0.,0.));
#4536=DIRECTION('center_axis',(0.,0.,-1.));
#4537=DIRECTION('ref_axis',(1.,0.,0.));
#4538=DIRECTION('center_axis',(1.22464679914735E-16,-1.,0.));
#4539=DIRECTION('ref_axis',(-1.,-1.22464679914735E-16,0.));
#4540=DIRECTION('center_axis',(0.,0.,1.));
#4541=DIRECTION('ref_axis',(1.,0.,0.));
#4542=DIRECTION('center_axis',(0.,0.,1.));
#4543=DIRECTION('ref_axis',(1.,0.,0.));
#4544=DIRECTION('',(0.,0.,-1.));
#4545=DIRECTION('center_axis',(0.,0.,-1.));
#4546=DIRECTION('ref_axis',(1.,0.,0.));
#4547=DIRECTION('center_axis',(0.,0.,1.));
#4548=DIRECTION('ref_axis',(1.,0.,0.));
#4549=DIRECTION('center_axis',(0.,0.,1.));
#4550=DIRECTION('ref_axis',(1.,0.,0.));
#4551=DIRECTION('center_axis',(1.22464679914735E-16,-1.,0.));
#4552=DIRECTION('ref_axis',(-1.,-1.22464679914735E-16,0.));
#4553=DIRECTION('center_axis',(0.,0.,1.));
#4554=DIRECTION('ref_axis',(1.,0.,0.));
#4555=DIRECTION('center_axis',(0.,0.,1.));
#4556=DIRECTION('ref_axis',(1.,0.,0.));
#4557=DIRECTION('center_axis',(0.,0.,-1.));
#4558=DIRECTION('ref_axis',(1.,0.,0.));
#4559=DIRECTION('center_axis',(0.,0.,-1.));
#4560=DIRECTION('ref_axis',(-1.,0.,0.));
#4561=DIRECTION('center_axis',(0.,0.,1.));
#4562=DIRECTION('ref_axis',(1.,0.,0.));
#4563=DIRECTION('center_axis',(1.22464679914735E-16,1.,0.));
#4564=DIRECTION('ref_axis',(1.,-1.22464679914735E-16,0.));
#4565=DIRECTION('center_axis',(0.,0.,1.));
#4566=DIRECTION('ref_axis',(1.,0.,0.));
#4567=DIRECTION('center_axis',(0.,0.,1.));
#4568=DIRECTION('ref_axis',(1.,0.,0.));
#4569=DIRECTION('',(0.,0.,-1.));
#4570=DIRECTION('center_axis',(0.,1.,0.));
#4571=DIRECTION('ref_axis',(1.,0.,0.));
#4572=DIRECTION('center_axis',(0.,1.,0.));
#4573=DIRECTION('ref_axis',(1.,0.,0.));
#4574=DIRECTION('',(0.,-1.,0.));
#4575=DIRECTION('center_axis',(0.,-1.,0.));
#4576=DIRECTION('ref_axis',(1.,0.,0.));
#4577=DIRECTION('center_axis',(0.,0.,1.));
#4578=DIRECTION('ref_axis',(1.,0.,0.));
#4579=DIRECTION('',(0.,0.,1.));
#4580=DIRECTION('center_axis',(0.,-1.,0.));
#4581=DIRECTION('ref_axis',(1.,0.,0.));
#4582=DIRECTION('center_axis',(0.,-1.,0.));
#4583=DIRECTION('ref_axis',(1.,0.,0.));
#4584=DIRECTION('',(0.,1.,0.));
#4585=DIRECTION('center_axis',(0.,-1.,0.));
#4586=DIRECTION('ref_axis',(1.,0.,0.));
#4587=DIRECTION('center_axis',(0.,-1.,0.));
#4588=DIRECTION('ref_axis',(1.,0.,0.));
#4589=DIRECTION('center_axis',(0.,1.,0.));
#4590=DIRECTION('ref_axis',(1.,0.,0.));
#4591=DIRECTION('center_axis',(0.,-1.,0.));
#4592=DIRECTION('ref_axis',(1.,0.,0.));
#4593=DIRECTION('center_axis',(0.,-1.,0.));
#4594=DIRECTION('ref_axis',(1.,0.,0.));
#4595=DIRECTION('',(0.,1.,0.));
#4596=DIRECTION('center_axis',(0.,1.,0.));
#4597=DIRECTION('ref_axis',(1.,0.,0.));
#4598=DIRECTION('center_axis',(0.,-1.,0.));
#4599=DIRECTION('ref_axis',(1.,0.,0.));
#4600=DIRECTION('center_axis',(0.,1.,0.));
#4601=DIRECTION('ref_axis',(1.,0.,0.));
#4602=DIRECTION('center_axis',(0.,1.,0.));
#4603=DIRECTION('ref_axis',(1.,0.,0.));
#4604=DIRECTION('',(0.,1.,0.));
#4605=DIRECTION('center_axis',(0.,1.,0.));
#4606=DIRECTION('ref_axis',(1.,0.,0.));
#4607=DIRECTION('center_axis',(0.,1.,0.));
#4608=DIRECTION('ref_axis',(1.,0.,0.));
#4609=DIRECTION('axis',(0.,0.,1.));
#4610=DIRECTION('refdir',(1.,0.,0.));
#4611=DIRECTION('center_axis',(0.,1.,0.));
#4612=DIRECTION('ref_axis',(-0.707106781186547,0.,-0.707106781186548));
#4613=DIRECTION('center_axis',(0.,-1.,0.));
#4614=DIRECTION('ref_axis',(-0.707106781186547,0.,-0.707106781186548));
#4615=DIRECTION('',(0.,-1.,0.));
#4616=DIRECTION('center_axis',(0.,1.,0.));
#4617=DIRECTION('ref_axis',(0.,0.,-1.));
#4618=DIRECTION('',(0.,1.,0.));
#4619=DIRECTION('center_axis',(0.,0.,1.));
#4620=DIRECTION('ref_axis',(1.,0.,0.));
#4621=DIRECTION('center_axis',(0.,-1.,0.));
#4622=DIRECTION('ref_axis',(0.,0.,-1.));
#4623=DIRECTION('center_axis',(0.,0.,-1.));
#4624=DIRECTION('ref_axis',(1.00929365875014E-16,-1.,0.));
#4625=DIRECTION('center_axis',(0.,0.,1.));
#4626=DIRECTION('ref_axis',(1.00929365875014E-16,-1.,0.));
#4627=DIRECTION('center_axis',(0.,1.,0.));
#4628=DIRECTION('ref_axis',(0.707106781186547,0.,-0.707106781186548));
#4629=DIRECTION('center_axis',(0.,-1.,0.));
#4630=DIRECTION('ref_axis',(0.707106781186547,0.,-0.707106781186548));
#4631=DIRECTION('',(0.,-1.,0.));
#4632=DIRECTION('',(0.,1.,0.));
#4633=DIRECTION('center_axis',(1.,0.,0.));
#4634=DIRECTION('ref_axis',(0.,0.,-1.));
#4635=DIRECTION('',(0.,0.,1.));
#4636=DIRECTION('',(0.,-1.,0.));
#4637=DIRECTION('',(0.,0.,1.));
#4638=DIRECTION('center_axis',(0.,0.,-1.));
#4639=DIRECTION('ref_axis',(0.707106781186547,-0.707106781186548,0.));
#4640=DIRECTION('',(0.,0.,1.));
#4641=DIRECTION('center_axis',(0.,0.,1.));
#4642=DIRECTION('ref_axis',(-5.04646829375071E-16,-1.,0.));
#4643=DIRECTION('center_axis',(1.,0.,0.));
#4644=DIRECTION('ref_axis',(0.,0.,-1.));
#4645=DIRECTION('',(0.,0.,1.));
#4646=DIRECTION('',(0.,1.,0.));
#4647=DIRECTION('center_axis',(0.,-1.,0.));
#4648=DIRECTION('ref_axis',(0.707106781186547,0.,0.707106781186548));
#4649=DIRECTION('center_axis',(0.,-1.,0.));
#4650=DIRECTION('ref_axis',(0.707106781186547,0.,0.707106781186548));
#4651=DIRECTION('',(0.,-1.,0.));
#4652=DIRECTION('center_axis',(0.,1.,0.));
#4653=DIRECTION('ref_axis',(0.,0.,1.));
#4654=DIRECTION('center_axis',(0.,0.,1.));
#4655=DIRECTION('ref_axis',(1.,0.,0.));
#4656=DIRECTION('center_axis',(0.,-1.,0.));
#4657=DIRECTION('ref_axis',(0.,0.,1.));
#4658=DIRECTION('center_axis',(0.,0.,-1.));
#4659=DIRECTION('ref_axis',(-5.04646829375071E-16,-1.,0.));
#4660=DIRECTION('center_axis',(0.,-1.,0.));
#4661=DIRECTION('ref_axis',(-0.707106781186543,0.,0.707106781186552));
#4662=DIRECTION('center_axis',(0.,-1.,0.));
#4663=DIRECTION('ref_axis',(-0.707106781186543,0.,0.707106781186552));
#4664=DIRECTION('',(0.,1.,0.));
#4665=DIRECTION('center_axis',(0.,0.,1.));
#4666=DIRECTION('ref_axis',(0.,-1.,0.));
#4667=DIRECTION('',(1.,0.,0.));
#4668=DIRECTION('center_axis',(0.,1.,0.));
#4669=DIRECTION('ref_axis',(0.,0.,1.));
#4670=DIRECTION('',(1.,0.,0.));
#4671=DIRECTION('',(1.,0.,0.));
#4672=DIRECTION('',(0.,0.,-1.));
#4673=DIRECTION('',(1.,0.,0.));
#4674=DIRECTION('',(0.,0.,-1.));
#4675=DIRECTION('center_axis',(0.,0.,-1.));
#4676=DIRECTION('ref_axis',(-0.666666666666667,-0.74535599249993,0.));
#4677=DIRECTION('center_axis',(0.,0.,1.));
#4678=DIRECTION('ref_axis',(-0.666666666666667,-0.74535599249993,0.));
#4679=DIRECTION('',(0.,0.,-1.));
#4680=DIRECTION('center_axis',(0.,0.,-1.));
#4681=DIRECTION('ref_axis',(-0.666666666666667,-0.74535599249993,0.));
#4682=DIRECTION('',(0.,0.,-1.));
#4683=DIRECTION('center_axis',(-1.,0.,0.));
#4684=DIRECTION('ref_axis',(0.,0.,1.));
#4685=DIRECTION('',(0.,1.,0.));
#4686=DIRECTION('',(0.,-1.,0.));
#4687=DIRECTION('center_axis',(0.,0.,1.));
#4688=DIRECTION('ref_axis',(0.666666666666667,-0.74535599249993,0.));
#4689=DIRECTION('center_axis',(0.,0.,-1.));
#4690=DIRECTION('ref_axis',(0.666666666666667,-0.74535599249993,0.));
#4691=DIRECTION('',(0.,0.,-1.));
#4692=DIRECTION('center_axis',(0.,0.,1.));
#4693=DIRECTION('ref_axis',(0.666666666666667,-0.74535599249993,0.));
#4694=DIRECTION('center_axis',(0.,0.,-1.));
#4695=DIRECTION('ref_axis',(0.,1.,0.));
#4696=DIRECTION('',(0.,-1.,0.));
#4697=DIRECTION('center_axis',(-1.,0.,0.));
#4698=DIRECTION('ref_axis',(0.,0.,1.));
#4699=DIRECTION('',(0.,1.,0.));
#4700=DIRECTION('center_axis',(0.,0.,1.));
#4701=DIRECTION('ref_axis',(0.,-1.,0.));
#4702=DIRECTION('center_axis',(0.,0.,-1.));
#4703=DIRECTION('ref_axis',(0.,1.,0.));
#4704=DIRECTION('axis',(0.,0.,1.));
#4705=DIRECTION('refdir',(1.,0.,0.));
#4706=DIRECTION('center_axis',(0.,-1.,0.));
#4707=DIRECTION('ref_axis',(0.,0.,-1.));
#4708=DIRECTION('center_axis',(0.,1.,0.));
#4709=DIRECTION('ref_axis',(1.,0.,0.));
#4710=DIRECTION('center_axis',(1.22464679914735E-16,0.,1.));
#4711=DIRECTION('ref_axis',(1.,0.,-6.12323399573677E-17));
#4712=DIRECTION('axis',(0.,0.,1.));
#4713=DIRECTION('refdir',(1.,0.,0.));
#4714=DIRECTION('center_axis',(0.,-1.,0.));
#4715=DIRECTION('ref_axis',(-0.130665282675078,0.,-0.991426539842182));
#4716=DIRECTION('',(0.,-1.,0.));
#4717=DIRECTION('center_axis',(0.,-1.,0.));
#4718=DIRECTION('ref_axis',(1.,0.,1.81309624337467E-14));
#4719=DIRECTION('center_axis',(0.,-1.,0.));
#4720=DIRECTION('ref_axis',(-0.130665282675078,0.,-0.991426539842182));
#4721=DIRECTION('',(0.,-1.,0.));
#4722=DIRECTION('center_axis',(0.,-1.,0.));
#4723=DIRECTION('ref_axis',(1.,0.,1.81309624337467E-14));
#4724=DIRECTION('center_axis',(0.,-1.,0.));
#4725=DIRECTION('ref_axis',(-0.130665282675078,0.,-0.991426539842182));
#4726=DIRECTION('',(0.,-1.,0.));
#4727=DIRECTION('center_axis',(0.,-1.,0.));
#4728=DIRECTION('ref_axis',(-0.130665282675078,0.,-0.991426539842182));
#4729=DIRECTION('',(0.,-1.,0.));
#4730=DIRECTION('center_axis',(0.,-1.,0.));
#4731=DIRECTION('ref_axis',(-0.130665282675078,0.,-0.991426539842182));
#4732=DIRECTION('',(0.,-1.,0.));
#4733=DIRECTION('center_axis',(0.,-1.,0.));
#4734=DIRECTION('ref_axis',(-0.130665282675078,0.,-0.991426539842182));
#4735=DIRECTION('',(0.,-1.,0.));
#4736=DIRECTION('center_axis',(0.,-1.,0.));
#4737=DIRECTION('ref_axis',(-0.130665282675078,0.,-0.991426539842182));
#4738=DIRECTION('',(0.,-1.,0.));
#4739=DIRECTION('center_axis',(0.,-1.,0.));
#4740=DIRECTION('ref_axis',(0.936888000853192,0.,0.349629623826857));
#4741=DIRECTION('',(0.,-1.,0.));
#4742=DIRECTION('center_axis',(0.,-1.,0.));
#4743=DIRECTION('ref_axis',(1.,0.,0.));
#4744=DIRECTION('center_axis',(0.,-1.,0.));
#4745=DIRECTION('ref_axis',(0.936888000853192,0.,0.349629623826857));
#4746=DIRECTION('',(0.,-1.,0.));
#4747=DIRECTION('center_axis',(0.,-1.,0.));
#4748=DIRECTION('ref_axis',(0.936888000853192,0.,0.349629623826857));
#4749=DIRECTION('',(0.,-1.,0.));
#4750=DIRECTION('center_axis',(0.,-1.,0.));
#4751=DIRECTION('ref_axis',(0.936888000853192,0.,0.349629623826857));
#4752=DIRECTION('',(0.,-1.,0.));
#4753=DIRECTION('center_axis',(0.,-1.,0.));
#4754=DIRECTION('ref_axis',(0.936888000853192,0.,0.349629623826857));
#4755=DIRECTION('',(0.,-1.,0.));
#4756=DIRECTION('center_axis',(0.,-1.,0.));
#4757=DIRECTION('ref_axis',(0.936888000853192,0.,0.349629623826857));
#4758=DIRECTION('',(0.,-1.,0.));
#4759=DIRECTION('center_axis',(0.,-1.,0.));
#4760=DIRECTION('ref_axis',(0.936888000853192,0.,0.349629623826857));
#4761=DIRECTION('center_axis',(0.,-1.,0.));
#4762=DIRECTION('ref_axis',(1.,0.,0.));
#4763=DIRECTION('center_axis',(0.,-1.,0.));
#4764=DIRECTION('ref_axis',(-0.130665282675078,0.,-0.991426539842182));
#4765=DIRECTION('center_axis',(0.,1.,0.));
#4766=DIRECTION('ref_axis',(1.,0.,1.81309624337467E-14));
#4767=DIRECTION('center_axis',(0.,-1.,0.));
#4768=DIRECTION('ref_axis',(1.,0.,0.));
#4769=DIRECTION('',(-1.,0.,4.69353744302978E-16));
#4770=DIRECTION('',(-0.499999999999999,0.,0.866025403784439));
#4771=DIRECTION('',(0.500000000000001,0.,0.866025403784438));
#4772=DIRECTION('',(1.,0.,-4.69353744302978E-16));
#4773=DIRECTION('',(0.5,0.,-0.866025403784439));
#4774=DIRECTION('',(-0.5,0.,-0.866025403784439));
#4775=DIRECTION('center_axis',(-0.866025403784439,0.,-0.499999999999999));
#4776=DIRECTION('ref_axis',(-0.499999999999999,0.,0.866025403784439));
#4777=DIRECTION('',(-0.499999999999999,0.,0.866025403784439));
#4778=DIRECTION('',(0.,1.,0.));
#4779=DIRECTION('',(0.,1.,0.));
#4780=DIRECTION('center_axis',(-0.866025403784438,0.,0.500000000000001));
#4781=DIRECTION('ref_axis',(0.500000000000001,0.,0.866025403784438));
#4782=DIRECTION('',(0.500000000000001,0.,0.866025403784438));
#4783=DIRECTION('',(0.,1.,0.));
#4784=DIRECTION('center_axis',(4.69353744302978E-16,0.,1.));
#4785=DIRECTION('ref_axis',(1.,0.,-4.69353744302978E-16));
#4786=DIRECTION('',(1.,0.,-4.69353744302978E-16));
#4787=DIRECTION('',(0.,1.,0.));
#4788=DIRECTION('center_axis',(0.866025403784439,0.,0.5));
#4789=DIRECTION('ref_axis',(0.5,0.,-0.866025403784439));
#4790=DIRECTION('',(0.5,0.,-0.866025403784439));
#4791=DIRECTION('',(0.,1.,0.));
#4792=DIRECTION('center_axis',(0.866025403784439,0.,-0.5));
#4793=DIRECTION('ref_axis',(-0.5,0.,-0.866025403784439));
#4794=DIRECTION('',(-0.5,0.,-0.866025403784439));
#4795=DIRECTION('',(0.,1.,0.));
#4796=DIRECTION('center_axis',(-4.69353744302978E-16,0.,-1.));
#4797=DIRECTION('ref_axis',(-1.,0.,4.69353744302978E-16));
#4798=DIRECTION('',(-1.,0.,4.69353744302978E-16));
#4799=DIRECTION('center_axis',(0.,-1.,0.));
#4800=DIRECTION('ref_axis',(1.,0.,0.));
#4801=DIRECTION('axis',(0.,0.,1.));
#4802=DIRECTION('refdir',(1.,0.,0.));
#4803=DIRECTION('center_axis',(0.,0.,1.));
#4804=DIRECTION('ref_axis',(0.457762905907022,0.889074306217179,0.));
#4805=DIRECTION('',(0.,0.,-1.));
#4806=DIRECTION('center_axis',(0.,0.,-1.));
#4807=DIRECTION('ref_axis',(-1.,1.34107269471161E-13,0.));
#4808=DIRECTION('center_axis',(0.,0.,1.));
#4809=DIRECTION('ref_axis',(0.457762905907022,0.889074306217179,0.));
#4810=DIRECTION('',(0.,0.,-1.));
#4811=DIRECTION('center_axis',(0.,0.,1.));
#4812=DIRECTION('ref_axis',(0.457762905907022,0.889074306217179,0.));
#4813=DIRECTION('',(0.,0.,-1.));
#4814=DIRECTION('center_axis',(0.,0.,1.));
#4815=DIRECTION('ref_axis',(0.457762905907022,0.889074306217179,0.));
#4816=DIRECTION('',(0.,0.,-1.));
#4817=DIRECTION('center_axis',(0.,0.,1.));
#4818=DIRECTION('ref_axis',(0.457762905907022,0.889074306217179,0.));
#4819=DIRECTION('',(0.,0.,-1.));
#4820=DIRECTION('center_axis',(0.,0.,1.));
#4821=DIRECTION('ref_axis',(0.457762905907022,0.889074306217179,0.));
#4822=DIRECTION('',(0.,0.,-1.));
#4823=DIRECTION('center_axis',(0.,0.,1.));
#4824=DIRECTION('ref_axis',(0.457762905907022,0.889074306217179,0.));
#4825=DIRECTION('',(0.,0.,-1.));
#4826=DIRECTION('center_axis',(0.,0.,1.));
#4827=DIRECTION('ref_axis',(0.457762905907022,0.889074306217179,0.));
#4828=DIRECTION('',(0.,0.,-1.));
#4829=DIRECTION('center_axis',(0.,0.,1.));
#4830=DIRECTION('ref_axis',(0.457762905907022,0.889074306217179,0.));
#4831=DIRECTION('',(0.,0.,-1.));
#4832=DIRECTION('center_axis',(0.,0.,1.));
#4833=DIRECTION('ref_axis',(0.457762905907022,0.889074306217179,0.));
#4834=DIRECTION('',(0.,0.,-1.));
#4835=DIRECTION('center_axis',(0.,0.,1.));
#4836=DIRECTION('ref_axis',(0.457762905907022,0.889074306217179,0.));
#4837=DIRECTION('',(0.,0.,-1.));
#4838=DIRECTION('center_axis',(0.,0.,1.));
#4839=DIRECTION('ref_axis',(0.457762905907022,0.889074306217179,0.));
#4840=DIRECTION('',(0.,0.,-1.));
#4841=DIRECTION('center_axis',(0.,0.,1.));
#4842=DIRECTION('ref_axis',(0.457762905907022,0.889074306217179,0.));
#4843=DIRECTION('',(0.,0.,-1.));
#4844=DIRECTION('center_axis',(0.,0.,1.));
#4845=DIRECTION('ref_axis',(0.457762905907022,0.889074306217179,0.));
#4846=DIRECTION('',(0.,0.,-1.));
#4847=DIRECTION('center_axis',(0.,0.,1.));
#4848=DIRECTION('ref_axis',(0.457762905907022,0.889074306217179,0.));
#4849=DIRECTION('',(0.,0.,-1.));
#4850=DIRECTION('center_axis',(0.,0.,1.));
#4851=DIRECTION('ref_axis',(0.457762905907022,0.889074306217179,0.));
#4852=DIRECTION('',(0.,0.,-1.));
#4853=DIRECTION('center_axis',(0.,0.,1.));
#4854=DIRECTION('ref_axis',(0.457762905907022,0.889074306217179,0.));
#4855=DIRECTION('',(0.,0.,-1.));
#4856=DIRECTION('center_axis',(0.,0.,1.));
#4857=DIRECTION('ref_axis',(0.457762905907022,0.889074306217179,0.));
#4858=DIRECTION('',(0.,0.,-1.));
#4859=DIRECTION('center_axis',(0.,0.,1.));
#4860=DIRECTION('ref_axis',(0.457762905907022,0.889074306217179,0.));
#4861=DIRECTION('',(0.,0.,-1.));
#4862=DIRECTION('center_axis',(0.,0.,1.));
#4863=DIRECTION('ref_axis',(0.457762905907022,0.889074306217179,0.));
#4864=DIRECTION('',(0.,0.,-1.));
#4865=DIRECTION('center_axis',(0.,0.,1.));
#4866=DIRECTION('ref_axis',(0.457762905907022,0.889074306217179,0.));
#4867=DIRECTION('',(0.,0.,-1.));
#4868=DIRECTION('center_axis',(0.,0.,1.));
#4869=DIRECTION('ref_axis',(0.457762905907022,0.889074306217179,0.));
#4870=DIRECTION('',(0.,0.,-1.));
#4871=DIRECTION('center_axis',(0.,0.,1.));
#4872=DIRECTION('ref_axis',(0.457762905907022,0.889074306217179,0.));
#4873=DIRECTION('',(0.,0.,-1.));
#4874=DIRECTION('center_axis',(0.,0.,1.));
#4875=DIRECTION('ref_axis',(0.457762905907022,0.889074306217179,0.));
#4876=DIRECTION('',(0.,0.,-1.));
#4877=DIRECTION('center_axis',(0.,0.,1.));
#4878=DIRECTION('ref_axis',(0.457762905907022,0.889074306217179,0.));
#4879=DIRECTION('',(0.,0.,-1.));
#4880=DIRECTION('center_axis',(0.,0.,1.));
#4881=DIRECTION('ref_axis',(0.457762905907022,0.889074306217179,0.));
#4882=DIRECTION('',(0.,0.,-1.));
#4883=DIRECTION('center_axis',(0.,0.,1.));
#4884=DIRECTION('ref_axis',(0.457762905907022,0.889074306217179,0.));
#4885=DIRECTION('',(0.,0.,-1.));
#4886=DIRECTION('center_axis',(0.,0.,1.));
#4887=DIRECTION('ref_axis',(0.457762905907022,0.889074306217179,0.));
#4888=DIRECTION('',(0.,0.,-1.));
#4889=DIRECTION('center_axis',(0.,0.,1.));
#4890=DIRECTION('ref_axis',(-1.,0.,0.));
#4891=DIRECTION('center_axis',(0.,0.,-1.));
#4892=DIRECTION('ref_axis',(-1.,0.,0.));
#4893=DIRECTION('center_axis',(0.,0.,-1.));
#4894=DIRECTION('ref_axis',(-1.,0.,0.));
#4895=DIRECTION('center_axis',(0.,0.,1.));
#4896=DIRECTION('ref_axis',(0.457762905907022,0.889074306217179,0.));
#4897=DIRECTION('center_axis',(0.,0.,1.));
#4898=DIRECTION('ref_axis',(-1.,1.34107269471161E-13,0.));
#4899=DIRECTION('center_axis',(0.,0.,1.));
#4900=DIRECTION('ref_axis',(-1.,0.,0.));
#4901=DIRECTION('center_axis',(0.,0.,1.));
#4902=DIRECTION('ref_axis',(-1.,0.,0.));
#4903=DIRECTION('axis',(0.,0.,1.));
#4904=DIRECTION('refdir',(1.,0.,0.));
#4905=DIRECTION('center_axis',(0.,1.,0.));
#4906=DIRECTION('ref_axis',(0.,0.,1.));
#4907=DIRECTION('center_axis',(0.,1.,0.));
#4908=DIRECTION('ref_axis',(1.,0.,0.));
#4909=DIRECTION('center_axis',(1.22464679914735E-16,0.,1.));
#4910=DIRECTION('ref_axis',(1.,0.,-6.12323399573677E-17));
#4911=DIRECTION('axis',(0.,0.,1.));
#4912=DIRECTION('refdir',(1.,0.,0.));
#4913=DIRECTION('center_axis',(0.,0.,1.));
#4914=DIRECTION('ref_axis',(-1.,0.,0.));
#4915=DIRECTION('center_axis',(0.,0.,1.));
#4916=DIRECTION('ref_axis',(-1.,0.,0.));
#4917=DIRECTION('',(0.,0.,1.));
#4918=DIRECTION('center_axis',(0.,0.,-1.));
#4919=DIRECTION('ref_axis',(-1.,0.,0.));
#4920=DIRECTION('center_axis',(0.,0.,1.));
#4921=DIRECTION('ref_axis',(1.,0.,0.));
#4922=DIRECTION('',(1.,-6.40987562127854E-16,0.));
#4923=DIRECTION('',(0.5,0.866025403784439,0.));
#4924=DIRECTION('',(-0.5,0.866025403784439,0.));
#4925=DIRECTION('',(-1.,3.20493781063927E-16,0.));
#4926=DIRECTION('',(-0.5,-0.866025403784439,0.));
#4927=DIRECTION('',(0.499999999999999,-0.866025403784439,0.));
#4928=DIRECTION('center_axis',(0.866025403784439,-0.5,0.));
#4929=DIRECTION('ref_axis',(-0.5,-0.866025403784439,0.));
#4930=DIRECTION('',(0.,0.,1.));
#4931=DIRECTION('',(-0.5,-0.866025403784439,0.));
#4932=DIRECTION('',(0.,0.,1.));
#4933=DIRECTION('center_axis',(0.866025403784439,0.5,0.));
#4934=DIRECTION('ref_axis',(0.5,-0.866025403784439,0.));
#4935=DIRECTION('',(0.5,-0.866025403784439,0.));
#4936=DIRECTION('',(0.,0.,1.));
#4937=DIRECTION('center_axis',(3.20493781063927E-16,1.,0.));
#4938=DIRECTION('ref_axis',(1.,-3.20493781063927E-16,0.));
#4939=DIRECTION('',(1.,-3.20493781063927E-16,0.));
#4940=DIRECTION('',(0.,0.,1.));
#4941=DIRECTION('center_axis',(-0.866025403784438,0.5,0.));
#4942=DIRECTION('ref_axis',(0.5,0.866025403784438,0.));
#4943=DIRECTION('',(0.5,0.866025403784439,0.));
#4944=DIRECTION('',(0.,0.,1.));
#4945=DIRECTION('center_axis',(-0.866025403784439,-0.5,0.));
#4946=DIRECTION('ref_axis',(-0.5,0.866025403784439,0.));
#4947=DIRECTION('',(-0.499999999999999,0.866025403784439,0.));
#4948=DIRECTION('',(0.,0.,-1.));
#4949=DIRECTION('center_axis',(-6.40987562127854E-16,-1.,0.));
#4950=DIRECTION('ref_axis',(-1.,6.40987562127854E-16,0.));
#4951=DIRECTION('',(-1.,6.40987562127854E-16,0.));
#4952=DIRECTION('center_axis',(0.,0.,-1.));
#4953=DIRECTION('ref_axis',(-1.,0.,0.));
#4954=DIRECTION('axis',(0.,0.,1.));
#4955=DIRECTION('refdir',(1.,0.,0.));
#4956=DIRECTION('center_axis',(0.,0.,1.));
#4957=DIRECTION('ref_axis',(-1.,0.,0.));
#4958=DIRECTION('',(0.,0.,1.));
#4959=DIRECTION('center_axis',(0.,0.,-1.));
#4960=DIRECTION('ref_axis',(-1.,0.,0.));
#4961=DIRECTION('center_axis',(0.,0.,1.));
#4962=DIRECTION('ref_axis',(-1.,0.,0.));
#4963=DIRECTION('',(0.,0.,1.));
#4964=DIRECTION('center_axis',(0.,0.,1.));
#4965=DIRECTION('ref_axis',(-1.,0.,0.));
#4966=DIRECTION('center_axis',(0.,0.,1.));
#4967=DIRECTION('ref_axis',(0.457762905907022,0.889074306217179,0.));
#4968=DIRECTION('',(0.,0.,1.));
#4969=DIRECTION('center_axis',(0.,0.,-1.));
#4970=DIRECTION('ref_axis',(0.457762905907022,0.889074306217179,0.));
#4971=DIRECTION('center_axis',(0.,0.,1.));
#4972=DIRECTION('ref_axis',(0.457762905907022,0.889074306217179,0.));
#4973=DIRECTION('',(0.,0.,1.));
#4974=DIRECTION('center_axis',(0.,0.,1.));
#4975=DIRECTION('ref_axis',(0.457762905907022,0.889074306217179,0.));
#4976=DIRECTION('',(0.,0.,1.));
#4977=DIRECTION('center_axis',(0.,0.,1.));
#4978=DIRECTION('ref_axis',(0.457762905907022,0.889074306217179,0.));
#4979=DIRECTION('center_axis',(0.,0.,1.));
#4980=DIRECTION('ref_axis',(0.457762905907022,0.889074306217179,0.));
#4981=DIRECTION('center_axis',(0.,0.,1.));
#4982=DIRECTION('ref_axis',(0.457762905907022,0.889074306217179,0.));
#4983=DIRECTION('center_axis',(0.,0.,1.));
#4984=DIRECTION('ref_axis',(-1.,0.,0.));
#4985=DIRECTION('center_axis',(-1.,0.,0.));
#4986=DIRECTION('ref_axis',(0.,0.,1.));
#4987=DIRECTION('center_axis',(0.,1.,0.));
#4988=DIRECTION('ref_axis',(0.,0.,-1.));
#4989=DIRECTION('center_axis',(-1.,0.,0.));
#4990=DIRECTION('ref_axis',(0.,0.382683432365091,0.923879532511286));
#4991=DIRECTION('center_axis',(0.,-0.707106781186548,0.707106781186548));
#4992=DIRECTION('ref_axis',(-1.,0.,0.));
#4993=DIRECTION('center_axis',(1.,0.,0.));
#4994=DIRECTION('ref_axis',(0.,0.382683432365091,0.923879532511286));
#4995=DIRECTION('center_axis',(0.,-0.707106781186547,0.707106781186548));
#4996=DIRECTION('ref_axis',(-0.707106781186549,-0.499999999999999,-0.499999999999999));
#4997=DIRECTION('center_axis',(0.,-0.707106781186554,0.707106781186541));
#4998=DIRECTION('ref_axis',(-1.,0.,0.));
#4999=DIRECTION('',(0.,-0.707106781186547,0.707106781186548));
#5000=DIRECTION('',(0.,0.707106781186547,-0.707106781186548));
#5001=DIRECTION('center_axis',(1.,0.,0.));
#5002=DIRECTION('ref_axis',(0.,0.,-1.));
#5003=DIRECTION('center_axis',(0.,-1.,0.));
#5004=DIRECTION('ref_axis',(-1.,0.,0.));
#5005=DIRECTION('center_axis',(-1.,0.,0.));
#5006=DIRECTION('ref_axis',(0.,-0.38268343236509,-0.923879532511287));
#5007=DIRECTION('center_axis',(1.,0.,0.));
#5008=DIRECTION('ref_axis',(0.,-0.38268343236509,-0.923879532511287));
#5009=DIRECTION('center_axis',(0.,-1.,0.));
#5010=DIRECTION('ref_axis',(-0.707106781186549,0.,-0.707106781186546));
#5011=DIRECTION('center_axis',(0.,-1.,0.));
#5012=DIRECTION('ref_axis',(-1.,0.,0.));
#5013=DIRECTION('',(0.,-1.,0.));
#5014=DIRECTION('',(0.,1.,0.));
#5015=DIRECTION('center_axis',(0.,0.,1.));
#5016=DIRECTION('ref_axis',(1.,0.,0.));
#5017=DIRECTION('center_axis',(-1.,0.,0.));
#5018=DIRECTION('ref_axis',(0.,1.,0.));
#5019=DIRECTION('center_axis',(0.,0.,1.));
#5020=DIRECTION('ref_axis',(-0.707106781186547,0.707106781186547,0.));
#5021=DIRECTION('center_axis',(0.,0.,-1.));
#5022=DIRECTION('ref_axis',(-0.707106781186548,0.707106781186548,0.));
#5023=DIRECTION('center_axis',(1.,0.,0.));
#5024=DIRECTION('ref_axis',(0.,0.707106781186549,-0.707106781186546));
#5025=DIRECTION('center_axis',(-1.,0.,0.));
#5026=DIRECTION('ref_axis',(0.,1.,0.));
#5027=DIRECTION('',(-1.,0.,0.));
#5028=DIRECTION('',(1.,0.,0.));
#5029=DIRECTION('center_axis',(0.,0.,1.));
#5030=DIRECTION('ref_axis',(1.,0.,0.));
#5031=DIRECTION('center_axis',(0.,1.,0.));
#5032=DIRECTION('ref_axis',(1.,0.,0.));
#5033=DIRECTION('center_axis',(0.,0.,1.));
#5034=DIRECTION('ref_axis',(0.707106781186547,0.707106781186547,0.));
#5035=DIRECTION('center_axis',(0.,0.,-1.));
#5036=DIRECTION('ref_axis',(0.707106781186548,0.707106781186548,0.));
#5037=DIRECTION('center_axis',(0.,1.,0.));
#5038=DIRECTION('ref_axis',(0.707106781186549,0.,-0.707106781186546));
#5039=DIRECTION('center_axis',(0.,1.,-2.22044604925032E-15));
#5040=DIRECTION('ref_axis',(1.,0.,0.));
#5041=DIRECTION('',(0.,1.,0.));
#5042=DIRECTION('',(0.,-1.,0.));
#5043=DIRECTION('center_axis',(-1.,0.,0.));
#5044=DIRECTION('ref_axis',(0.,0.,1.));
#5045=DIRECTION('center_axis',(0.,0.707106781186548,-0.707106781186548));
#5046=DIRECTION('ref_axis',(1.,0.,0.));
#5047=DIRECTION('center_axis',(1.,0.,0.));
#5048=DIRECTION('ref_axis',(0.,-0.38268343236509,-0.923879532511287));
#5049=DIRECTION('center_axis',(-1.,0.,0.));
#5050=DIRECTION('ref_axis',(0.,-0.38268343236509,-0.923879532511287));
#5051=DIRECTION('center_axis',(0.,0.707106781186547,-0.707106781186548));
#5052=DIRECTION('ref_axis',(0.707106781186549,-0.499999999999999,-0.499999999999999));
#5053=DIRECTION('center_axis',(0.,0.707106781186552,-0.707106781186543));
#5054=DIRECTION('ref_axis',(1.,0.,0.));
#5055=DIRECTION('',(0.,0.707106781186547,-0.707106781186548));
#5056=DIRECTION('',(0.,-0.707106781186547,0.707106781186548));
#5057=DIRECTION('center_axis',(1.,0.,0.));
#5058=DIRECTION('ref_axis',(0.,0.,-1.));
#5059=DIRECTION('center_axis',(0.,1.,0.));
#5060=DIRECTION('ref_axis',(1.,0.,0.));
#5061=DIRECTION('center_axis',(-1.,0.,0.));
#5062=DIRECTION('ref_axis',(0.,0.382683432365091,0.923879532511286));
#5063=DIRECTION('center_axis',(1.,0.,0.));
#5064=DIRECTION('ref_axis',(0.,0.382683432365091,0.923879532511286));
#5065=DIRECTION('center_axis',(0.,1.,0.));
#5066=DIRECTION('ref_axis',(0.707106781186555,0.,-0.70710678118654));
#5067=DIRECTION('center_axis',(0.,1.,0.));
#5068=DIRECTION('ref_axis',(1.,0.,0.));
#5069=DIRECTION('',(0.,1.,0.));
#5070=DIRECTION('',(0.,-1.,0.));
#5071=DIRECTION('center_axis',(0.,0.,1.));
#5072=DIRECTION('ref_axis',(1.,0.,0.));
#5073=DIRECTION('center_axis',(0.,-1.,0.));
#5074=DIRECTION('ref_axis',(-1.,0.,0.));
#5075=DIRECTION('center_axis',(0.,0.,1.));
#5076=DIRECTION('ref_axis',(0.,-1.,0.));
#5077=DIRECTION('center_axis',(0.,0.,-1.));
#5078=DIRECTION('ref_axis',(0.,-1.,0.));
#5079=DIRECTION('center_axis',(0.,-1.,0.));
#5080=DIRECTION('ref_axis',(-0.707106781186555,0.,-0.70710678118654));
#5081=DIRECTION('',(0.,1.,0.));
#5082=DIRECTION('',(0.,-1.,0.));
#5083=DIRECTION('center_axis',(0.,0.,1.));
#5084=DIRECTION('ref_axis',(0.707106781186548,0.707106781186548,0.));
#5085=DIRECTION('',(0.,0.,1.));
#5086=DIRECTION('center_axis',(0.,0.,1.));
#5087=DIRECTION('ref_axis',(0.707106781186548,0.707106781186548,0.));
#5088=DIRECTION('',(0.,0.,-1.));
#5089=DIRECTION('center_axis',(0.,1.,0.));
#5090=DIRECTION('ref_axis',(0.,0.,1.));
#5091=DIRECTION('',(0.,0.,-1.));
#5092=DIRECTION('',(-1.,0.,0.));
#5093=DIRECTION('center_axis',(0.,0.,-1.));
#5094=DIRECTION('ref_axis',(-0.707106781186548,0.707106781186548,0.));
#5095=DIRECTION('',(0.,0.,1.));
#5096=DIRECTION('center_axis',(0.,0.,1.));
#5097=DIRECTION('ref_axis',(-0.707106781186548,0.707106781186548,0.));
#5098=DIRECTION('center_axis',(-1.,0.,0.));
#5099=DIRECTION('ref_axis',(0.,0.,1.));
#5100=DIRECTION('',(0.,0.,-1.));
#5101=DIRECTION('',(0.,-1.,0.));
#5102=DIRECTION('center_axis',(1.,0.,0.));
#5103=DIRECTION('ref_axis',(0.,0.382683432365091,0.923879532511286));
#5104=DIRECTION('',(0.,-0.707106781186547,0.707106781186548));
#5105=DIRECTION('center_axis',(-1.,0.,0.));
#5106=DIRECTION('ref_axis',(0.,-0.38268343236509,-0.923879532511287));
#5107=DIRECTION('',(0.,-1.,0.));
#5108=DIRECTION('center_axis',(0.,0.,-1.));
#5109=DIRECTION('ref_axis',(0.,1.,0.));
#5110=DIRECTION('',(-1.,0.,0.));
#5111=DIRECTION('center_axis',(1.,0.,0.));
#5112=DIRECTION('ref_axis',(0.,-0.38268343236509,-0.923879532511287));
#5113=DIRECTION('',(-1.,0.,0.));
#5114=DIRECTION('',(1.,0.,0.));
#5115=DIRECTION('center_axis',(0.,-0.707106781186548,-0.707106781186547));
#5116=DIRECTION('ref_axis',(0.,0.707106781186547,-0.707106781186548));
#5117=DIRECTION('',(1.,0.,0.));
#5118=DIRECTION('center_axis',(1.,0.,0.));
#5119=DIRECTION('ref_axis',(0.,0.38268343236509,0.923879532511287));
#5120=DIRECTION('center_axis',(-1.,0.,0.));
#5121=DIRECTION('ref_axis',(0.,0.,1.));
#5122=DIRECTION('center_axis',(0.,1.,0.));
#5123=DIRECTION('ref_axis',(0.,0.,1.));
#5124=DIRECTION('center_axis',(-1.,0.,0.));
#5125=DIRECTION('ref_axis',(0.,0.382683432365091,0.923879532511286));
#5126=DIRECTION('center_axis',(0.,-0.707106781186539,0.707106781186556));
#5127=DIRECTION('ref_axis',(1.,0.,0.));
#5128=DIRECTION('center_axis',(1.,0.,0.));
#5129=DIRECTION('ref_axis',(0.,0.382683432365091,0.923879532511286));
#5130=DIRECTION('center_axis',(0.,-0.707106781186547,0.707106781186548));
#5131=DIRECTION('ref_axis',(0.707106781186549,0.499999999999999,0.499999999999999));
#5132=DIRECTION('center_axis',(0.,-0.707106781186545,0.70710678118655));
#5133=DIRECTION('ref_axis',(1.,0.,0.));
#5134=DIRECTION('',(0.,-0.707106781186547,0.707106781186548));
#5135=DIRECTION('',(0.,0.707106781186547,-0.707106781186548));
#5136=DIRECTION('center_axis',(1.,0.,0.));
#5137=DIRECTION('ref_axis',(0.,0.,-1.));
#5138=DIRECTION('center_axis',(0.,-1.,0.));
#5139=DIRECTION('ref_axis',(1.,0.,0.));
#5140=DIRECTION('center_axis',(-1.,0.,0.));
#5141=DIRECTION('ref_axis',(0.,-0.38268343236509,-0.923879532511287));
#5142=DIRECTION('center_axis',(1.,0.,0.));
#5143=DIRECTION('ref_axis',(0.,-0.38268343236509,-0.923879532511287));
#5144=DIRECTION('center_axis',(0.,-1.,0.));
#5145=DIRECTION('ref_axis',(0.707106781186549,0.,0.707106781186546));
#5146=DIRECTION('center_axis',(0.,-1.,0.));
#5147=DIRECTION('ref_axis',(1.,0.,0.));
#5148=DIRECTION('',(0.,-1.,0.));
#5149=DIRECTION('',(0.,1.,0.));
#5150=DIRECTION('center_axis',(0.,0.,-1.));
#5151=DIRECTION('ref_axis',(-1.,0.,0.));
#5152=DIRECTION('center_axis',(1.,0.,0.));
#5153=DIRECTION('ref_axis',(0.,1.,0.));
#5154=DIRECTION('center_axis',(0.,0.,-1.));
#5155=DIRECTION('ref_axis',(0.707106781186547,0.707106781186547,0.));
#5156=DIRECTION('center_axis',(1.,0.,0.));
#5157=DIRECTION('ref_axis',(0.,0.707106781186549,0.707106781186546));
#5158=DIRECTION('center_axis',(1.,0.,0.));
#5159=DIRECTION('ref_axis',(0.,1.,0.));
#5160=DIRECTION('',(1.,0.,0.));
#5161=DIRECTION('center_axis',(0.,0.,-1.));
#5162=DIRECTION('ref_axis',(-1.,0.,0.));
#5163=DIRECTION('center_axis',(0.,1.,0.));
#5164=DIRECTION('ref_axis',(-1.,0.,0.));
#5165=DIRECTION('center_axis',(0.,0.,-1.));
#5166=DIRECTION('ref_axis',(-0.707106781186547,0.707106781186547,0.));
#5167=DIRECTION('center_axis',(0.,1.,0.));
#5168=DIRECTION('ref_axis',(-0.707106781186549,0.,0.707106781186546));
#5169=DIRECTION('center_axis',(0.,1.,0.));
#5170=DIRECTION('ref_axis',(-1.,0.,0.));
#5171=DIRECTION('',(0.,1.,0.));
#5172=DIRECTION('center_axis',(-1.,0.,0.));
#5173=DIRECTION('ref_axis',(0.,0.,1.));
#5174=DIRECTION('center_axis',(0.,0.707106781186545,-0.70710678118655));
#5175=DIRECTION('ref_axis',(-1.,0.,0.));
#5176=DIRECTION('center_axis',(1.,0.,0.));
#5177=DIRECTION('ref_axis',(0.,-0.38268343236509,-0.923879532511287));
#5178=DIRECTION('center_axis',(0.,0.707106781186547,-0.707106781186548));
#5179=DIRECTION('ref_axis',(-0.707106781186549,0.499999999999999,0.499999999999999));
#5180=DIRECTION('center_axis',(0.,0.707106781186548,-0.707106781186548));
#5181=DIRECTION('ref_axis',(-1.,0.,0.));
#5182=DIRECTION('',(0.,0.707106781186547,-0.707106781186548));
#5183=DIRECTION('center_axis',(1.,0.,0.));
#5184=DIRECTION('ref_axis',(0.,0.,-1.));
#5185=DIRECTION('center_axis',(0.,1.,0.));
#5186=DIRECTION('ref_axis',(-1.,0.,0.));
#5187=DIRECTION('center_axis',(-1.,0.,0.));
#5188=DIRECTION('ref_axis',(0.,0.382683432365091,0.923879532511286));
#5189=DIRECTION('center_axis',(0.,1.,0.));
#5190=DIRECTION('ref_axis',(-0.707106781186543,0.,0.707106781186552));
#5191=DIRECTION('center_axis',(0.,1.,0.));
#5192=DIRECTION('ref_axis',(-1.,0.,0.));
#5193=DIRECTION('',(0.,1.,0.));
#5194=DIRECTION('center_axis',(0.,0.,-1.));
#5195=DIRECTION('ref_axis',(-1.,0.,0.));
#5196=DIRECTION('center_axis',(0.,-1.,0.));
#5197=DIRECTION('ref_axis',(1.,0.,0.));
#5198=DIRECTION('center_axis',(0.,0.,-1.));
#5199=DIRECTION('ref_axis',(0.,-1.,0.));
#5200=DIRECTION('center_axis',(0.,0.,1.));
#5201=DIRECTION('ref_axis',(0.,-1.,0.));
#5202=DIRECTION('center_axis',(0.,-1.,0.));
#5203=DIRECTION('ref_axis',(0.707106781186543,0.,0.707106781186552));
#5204=DIRECTION('',(0.,1.,0.));
#5205=DIRECTION('',(0.,-1.,0.));
#5206=DIRECTION('center_axis',(0.,0.,1.));
#5207=DIRECTION('ref_axis',(0.,-1.,0.));
#5208=DIRECTION('',(1.,0.,0.));
#5209=DIRECTION('center_axis',(-1.,0.,0.));
#5210=DIRECTION('ref_axis',(0.,-0.38268343236509,-0.923879532511287));
#5211=DIRECTION('',(1.,0.,0.));
#5212=DIRECTION('',(-1.,0.,0.));
#5213=DIRECTION('center_axis',(0.,0.707106781186548,0.707106781186547));
#5214=DIRECTION('ref_axis',(0.,-0.707106781186547,0.707106781186548));
#5215=DIRECTION('',(-1.,0.,0.));
#5216=DIRECTION('center_axis',(1.,0.,0.));
#5217=DIRECTION('ref_axis',(0.,0.38268343236509,0.923879532511287));
#5218=DIRECTION('center_axis',(1.,0.,0.));
#5219=DIRECTION('ref_axis',(0.,0.,-1.));
#5220=DIRECTION('',(0.,0.,1.));
#5221=DIRECTION('center_axis',(0.,0.,1.));
#5222=DIRECTION('ref_axis',(-0.707106781186548,-0.707106781186548,0.));
#5223=DIRECTION('center_axis',(0.,0.,-1.));
#5224=DIRECTION('ref_axis',(0.,1.,0.));
#5225=DIRECTION('center_axis',(0.,0.,1.));
#5226=DIRECTION('ref_axis',(0.,-1.,0.));
#5227=DIRECTION('axis',(0.,0.,1.));
#5228=DIRECTION('refdir',(1.,0.,0.));
#5229=DIRECTION('center_axis',(0.,-1.,0.));
#5230=DIRECTION('ref_axis',(-0.608872791442031,0.,0.793267876471491));
#5231=DIRECTION('',(0.,-1.,0.));
#5232=DIRECTION('center_axis',(0.,1.,0.));
#5233=DIRECTION('ref_axis',(1.,0.,1.81309624337467E-14));
#5234=DIRECTION('center_axis',(0.,-1.,0.));
#5235=DIRECTION('ref_axis',(-0.608872791442031,0.,0.793267876471491));
#5236=DIRECTION('',(0.,-1.,0.));
#5237=DIRECTION('center_axis',(0.,-1.,0.));
#5238=DIRECTION('ref_axis',(-0.608872791442031,0.,0.793267876471491));
#5239=DIRECTION('',(0.,-1.,0.));
#5240=DIRECTION('center_axis',(0.,-1.,0.));
#5241=DIRECTION('ref_axis',(-0.608872791442031,0.,0.793267876471491));
#5242=DIRECTION('',(0.,-1.,0.));
#5243=DIRECTION('center_axis',(0.,-1.,0.));
#5244=DIRECTION('ref_axis',(-0.608872791442031,0.,0.793267876471491));
#5245=DIRECTION('',(0.,-1.,0.));
#5246=DIRECTION('center_axis',(0.,-1.,0.));
#5247=DIRECTION('ref_axis',(-0.608872791442031,0.,0.793267876471491));
#5248=DIRECTION('',(0.,-1.,0.));
#5249=DIRECTION('center_axis',(0.,-1.,0.));
#5250=DIRECTION('ref_axis',(-0.608872791442031,0.,0.793267876471491));
#5251=DIRECTION('',(0.,-1.,0.));
#5252=DIRECTION('center_axis',(0.,-1.,0.));
#5253=DIRECTION('ref_axis',(1.,0.,1.81309624337467E-14));
#5254=DIRECTION('center_axis',(0.,-1.,0.));
#5255=DIRECTION('ref_axis',(-0.986183607793452,0.,-0.165655943809726));
#5256=DIRECTION('',(0.,-1.,0.));
#5257=DIRECTION('center_axis',(0.,-1.,0.));
#5258=DIRECTION('ref_axis',(1.,0.,0.));
#5259=DIRECTION('center_axis',(0.,-1.,0.));
#5260=DIRECTION('ref_axis',(-0.986183607793452,0.,-0.165655943809726));
#5261=DIRECTION('',(0.,-1.,0.));
#5262=DIRECTION('center_axis',(0.,-1.,0.));
#5263=DIRECTION('ref_axis',(-0.986183607793452,0.,-0.165655943809726));
#5264=DIRECTION('',(0.,-1.,0.));
#5265=DIRECTION('center_axis',(0.,-1.,0.));
#5266=DIRECTION('ref_axis',(-0.986183607793452,0.,-0.165655943809726));
#5267=DIRECTION('',(0.,-1.,0.));
#5268=DIRECTION('center_axis',(0.,-1.,0.));
#5269=DIRECTION('ref_axis',(-0.986183607793452,0.,-0.165655943809726));
#5270=DIRECTION('',(0.,-1.,0.));
#5271=DIRECTION('center_axis',(0.,-1.,0.));
#5272=DIRECTION('ref_axis',(-0.986183607793452,0.,-0.165655943809726));
#5273=DIRECTION('',(0.,-1.,0.));
#5274=DIRECTION('center_axis',(0.,-1.,0.));
#5275=DIRECTION('ref_axis',(-0.986183607793452,0.,-0.165655943809726));
#5276=DIRECTION('',(0.,-1.,0.));
#5277=DIRECTION('center_axis',(0.,-1.,0.));
#5278=DIRECTION('ref_axis',(1.,0.,0.));
#5279=DIRECTION('center_axis',(0.,-1.,0.));
#5280=DIRECTION('ref_axis',(-0.986183607793452,0.,-0.165655943809726));
#5281=DIRECTION('center_axis',(0.,-1.,0.));
#5282=DIRECTION('ref_axis',(-0.608872791442031,0.,0.793267876471491));
#5283=DIRECTION('center_axis',(0.,-1.,0.));
#5284=DIRECTION('ref_axis',(1.,0.,0.));
#5285=DIRECTION('',(-1.,0.,4.69353744302978E-16));
#5286=DIRECTION('',(-0.5,0.,-0.866025403784439));
#5287=DIRECTION('',(0.5,0.,-0.866025403784439));
#5288=DIRECTION('',(1.,0.,-4.69353744302978E-16));
#5289=DIRECTION('',(0.500000000000001,0.,0.866025403784438));
#5290=DIRECTION('',(-0.499999999999999,0.,0.866025403784439));
#5291=DIRECTION('center_axis',(0.866025403784439,0.,0.499999999999999));
#5292=DIRECTION('ref_axis',(-0.499999999999999,0.,0.866025403784439));
#5293=DIRECTION('',(-0.499999999999999,0.,0.866025403784439));
#5294=DIRECTION('',(0.,-1.,0.));
#5295=DIRECTION('',(0.,-1.,0.));
#5296=DIRECTION('center_axis',(0.866025403784438,0.,-0.500000000000001));
#5297=DIRECTION('ref_axis',(0.500000000000001,0.,0.866025403784438));
#5298=DIRECTION('',(0.500000000000001,0.,0.866025403784438));
#5299=DIRECTION('',(0.,-1.,0.));
#5300=DIRECTION('center_axis',(-4.69353744302978E-16,0.,-1.));
#5301=DIRECTION('ref_axis',(1.,0.,-4.69353744302978E-16));
#5302=DIRECTION('',(1.,0.,-4.69353744302978E-16));
#5303=DIRECTION('',(0.,-1.,0.));
#5304=DIRECTION('center_axis',(-0.866025403784439,0.,-0.5));
#5305=DIRECTION('ref_axis',(0.5,0.,-0.866025403784439));
#5306=DIRECTION('',(0.5,0.,-0.866025403784439));
#5307=DIRECTION('',(0.,-1.,0.));
#5308=DIRECTION('center_axis',(-0.866025403784439,0.,0.5));
#5309=DIRECTION('ref_axis',(-0.5,0.,-0.866025403784439));
#5310=DIRECTION('',(-0.5,0.,-0.866025403784439));
#5311=DIRECTION('',(0.,-1.,0.));
#5312=DIRECTION('center_axis',(4.69353744302978E-16,0.,1.));
#5313=DIRECTION('ref_axis',(-1.,0.,4.69353744302978E-16));
#5314=DIRECTION('',(-1.,0.,4.69353744302978E-16));
#5315=DIRECTION('center_axis',(0.,-1.,0.));
#5316=DIRECTION('ref_axis',(1.,0.,0.));
#5317=DIRECTION('',(0.,0.,1.));
#5318=DIRECTION('',(1.,0.,0.));
#5319=DIRECTION('',(0.,0.,1.));
#5320=DIRECTION('',(1.,0.,0.));
#5321=DIRECTION('',(0.,0.,1.));
#5322=DIRECTION('',(1.,0.,0.));
#5323=DIRECTION('',(0.,0.,1.));
#5324=DIRECTION('',(1.,0.,0.));
#5325=DIRECTION('',(0.,0.,1.));
#5326=DIRECTION('',(1.,0.,0.));
#5327=DIRECTION('',(0.,0.,1.));
#5328=DIRECTION('',(1.,0.,0.));
#5329=DIRECTION('',(0.,0.,1.));
#5330=DIRECTION('',(1.,0.,0.));
#5331=DIRECTION('',(0.,0.,1.));
#5332=DIRECTION('',(1.,0.,0.));
#5333=DIRECTION('',(0.,0.,1.));
#5334=DIRECTION('',(1.,0.,0.));
#5335=CARTESIAN_POINT('',(0.,0.,0.));
#5336=CARTESIAN_POINT('',(0.,0.,0.));
#5337=CARTESIAN_POINT('Origin',(3.46410161513776,6.,32.));
#5338=CARTESIAN_POINT('',(3.46410161513776,6.,32.));
#5339=CARTESIAN_POINT('',(6.92820323027551,-2.22044604925031E-15,32.));
#5340=CARTESIAN_POINT('',(4.3301270189222,4.5,32.));
#5341=CARTESIAN_POINT('',(3.46410161513776,6.,29.));
#5342=CARTESIAN_POINT('',(3.46410161513776,6.,32.));
#5343=CARTESIAN_POINT('',(5.19615242270663,3.,29.));
#5344=CARTESIAN_POINT('',(6.92820323027551,-2.22044604925031E-15,29.));
#5345=CARTESIAN_POINT('',(6.92820323027551,-2.22044604925031E-15,29.));
#5346=CARTESIAN_POINT('',(6.92820323027551,-2.22044604925031E-15,29.));
#5347=CARTESIAN_POINT('',(6.92820323027551,-2.22044604925031E-15,32.));
#5348=CARTESIAN_POINT('Origin',(-3.46410161513775,6.,32.));
#5349=CARTESIAN_POINT('',(-3.46410161513775,6.,32.));
#5350=CARTESIAN_POINT('',(-1.73205080756887,6.,32.));
#5351=CARTESIAN_POINT('',(-3.46410161513775,6.,29.));
#5352=CARTESIAN_POINT('',(-3.46410161513775,6.,32.));
#5353=CARTESIAN_POINT('',(1.94289029309402E-15,6.,29.));
#5354=CARTESIAN_POINT('',(3.46410161513776,6.,29.));
#5355=CARTESIAN_POINT('',(3.46410161513776,6.,29.));
#5356=CARTESIAN_POINT('Origin',(6.92820323027551,-2.22044604925031E-15,
32.));
#5357=CARTESIAN_POINT('',(3.46410161513775,-6.,32.));
#5358=CARTESIAN_POINT('',(6.06217782649107,-1.5,32.));
#5359=CARTESIAN_POINT('',(5.19615242270663,-3.,29.));
#5360=CARTESIAN_POINT('',(3.46410161513775,-6.,29.));
#5361=CARTESIAN_POINT('',(3.46410161513775,-6.,29.));
#5362=CARTESIAN_POINT('',(3.46410161513775,-6.,29.));
#5363=CARTESIAN_POINT('',(3.46410161513775,-6.,32.));
#5364=CARTESIAN_POINT('Origin',(-6.92820323027551,4.44089209850063E-15,
32.));
#5365=CARTESIAN_POINT('',(-6.92820323027551,3.88578058618805E-15,32.));
#5366=CARTESIAN_POINT('',(-6.06217782649107,1.5,32.));
#5367=CARTESIAN_POINT('',(-6.92820323027551,4.44089209850063E-15,29.));
#5368=CARTESIAN_POINT('',(-6.92820323027551,3.88578058618805E-15,32.));
#5369=CARTESIAN_POINT('',(-5.19615242270663,3.,29.));
#5370=CARTESIAN_POINT('',(-3.46410161513775,6.,29.));
#5371=CARTESIAN_POINT('',(-3.46410161513775,6.,29.));
#5372=CARTESIAN_POINT('Origin',(0.,0.,29.));
#5373=CARTESIAN_POINT('',(-5.19615242270663,-3.,29.));
#5374=CARTESIAN_POINT('',(-3.88578058618805E-15,-6.,29.));
#5375=CARTESIAN_POINT('Origin',(0.,0.,29.));
#5376=CARTESIAN_POINT('',(-3.46410161513776,-6.,29.));
#5377=CARTESIAN_POINT('',(-6.92820323027551,3.88578058618805E-15,29.));
#5378=CARTESIAN_POINT('',(-3.46410161513776,-6.,29.));
#5379=CARTESIAN_POINT('Origin',(0.,0.,29.));
#5380=CARTESIAN_POINT('Origin',(0.,0.,29.));
#5381=CARTESIAN_POINT('',(-3.46410161513776,-6.,29.));
#5382=CARTESIAN_POINT('Origin',(0.,0.,29.));
#5383=CARTESIAN_POINT('Origin',(0.,0.,29.));
#5384=CARTESIAN_POINT('Origin',(0.,0.,29.));
#5385=CARTESIAN_POINT('Origin',(0.,0.,29.));
#5386=CARTESIAN_POINT('Origin',(0.,0.,29.));
#5387=CARTESIAN_POINT('Origin',(0.,0.,29.));
#5388=CARTESIAN_POINT('Origin',(0.,0.,29.));
#5389=CARTESIAN_POINT('',(-6.,-7.34788079488412E-16,29.));
#5390=CARTESIAN_POINT('Origin',(0.,0.,29.));
#5391=CARTESIAN_POINT('',(-6.92820323027551,3.88578058618805E-15,29.));
#5392=CARTESIAN_POINT('Origin',(0.,0.,29.));
#5393=CARTESIAN_POINT('Origin',(3.46410161513775,-6.,32.));
#5394=CARTESIAN_POINT('',(-3.46410161513776,-6.,32.));
#5395=CARTESIAN_POINT('',(1.73205080756887,-6.,32.));
#5396=CARTESIAN_POINT('',(-3.46410161513776,-6.,32.));
#5397=CARTESIAN_POINT('Origin',(-3.46410161513776,-6.,32.));
#5398=CARTESIAN_POINT('',(-4.3301270189222,-4.5,32.));
#5399=CARTESIAN_POINT('Origin',(0.,0.,31.5));
#5400=CARTESIAN_POINT('',(-8.5,1.04094977927525E-15,32.));
#5401=CARTESIAN_POINT('Origin',(0.,0.,32.));
#5402=CARTESIAN_POINT('',(-9.,-1.10218211923262E-15,31.5));
#5403=CARTESIAN_POINT('Origin',(-8.5,-1.04094977927525E-15,31.5));
#5404=CARTESIAN_POINT('Origin',(0.,0.,31.5));
#5405=CARTESIAN_POINT('Origin',(0.,0.,0.));
#5406=CARTESIAN_POINT('',(-9.,1.10218211923262E-15,28.5));
#5407=CARTESIAN_POINT('',(-9.,-1.10218211923262E-15,0.));
#5408=CARTESIAN_POINT('Origin',(0.,0.,28.5));
#5409=CARTESIAN_POINT('Origin',(0.,0.,32.));
#5410=CARTESIAN_POINT('Origin',(0.,0.,28.5));
#5411=CARTESIAN_POINT('',(-8.5,-1.04094977927525E-15,28.));
#5412=CARTESIAN_POINT('Origin',(-8.5,-1.04094977927525E-15,28.5));
#5413=CARTESIAN_POINT('Origin',(0.,0.,28.));
#5414=CARTESIAN_POINT('Origin',(0.,0.,28.));
#5415=CARTESIAN_POINT('',(8.,-9.79717439317883E-16,28.));
#5416=CARTESIAN_POINT('Origin',(0.,0.,28.));
#5417=CARTESIAN_POINT('Origin',(0.,0.,27.5));
#5418=CARTESIAN_POINT('',(-7.5,-9.18485099360515E-16,27.5));
#5419=CARTESIAN_POINT('',(7.5,-9.18485099360515E-16,27.5));
#5420=CARTESIAN_POINT('Origin',(0.,0.,27.5));
#5421=CARTESIAN_POINT('Origin',(8.,-9.79717439317883E-16,27.5));
#5422=CARTESIAN_POINT('Origin',(0.,0.,27.5));
#5423=CARTESIAN_POINT('Origin',(0.,0.,0.));
#5424=CARTESIAN_POINT('',(-7.49999999972844,-6.38227930889562E-5,19.332958859286));
#5425=CARTESIAN_POINT('',(-7.5,-9.18485099360515E-16,0.));
#5426=CARTESIAN_POINT('',(7.5,-2.77555756156289E-16,19.3326149291812));
#5427=CARTESIAN_POINT('Ctrl Pts',(7.5,1.82323373546694E-16,19.3326149291812));
#5428=CARTESIAN_POINT('Ctrl Pts',(7.5,-0.179953506202678,19.3326149291812));
#5429=CARTESIAN_POINT('Ctrl Pts',(7.49351901743291,-0.35981913831206,19.3379986486473));
#5430=CARTESIAN_POINT('Ctrl Pts',(7.48060194606833,-0.539068200210999,19.348331639646));
#5431=CARTESIAN_POINT('Ctrl Pts',(7.46767830519883,-0.718408426551234,19.3586698859099));
#5432=CARTESIAN_POINT('Ctrl Pts',(7.44831209315138,-0.897131076731049,19.3739624392954));
#5433=CARTESIAN_POINT('Ctrl Pts',(7.42259977836276,-1.07471509259388,19.393774188663));
#5434=CARTESIAN_POINT('Ctrl Pts',(7.39686912390173,-1.25242577276927,19.4136000690412));
#5435=CARTESIAN_POINT('Ctrl Pts',(7.36478341945685,-1.42899582546002,19.4379515944617));
#5436=CARTESIAN_POINT('Ctrl Pts',(7.32648959561089,-1.60391714418337,19.466392722073));
#5437=CARTESIAN_POINT('Ctrl Pts',(7.28813393850825,-1.77912090936192,19.494879773736));
#5438=CARTESIAN_POINT('Ctrl Pts',(7.24355024225288,-1.95267025573421,19.5274696452608));
#5439=CARTESIAN_POINT('Ctrl Pts',(7.19293465289676,-2.12407416988132,19.5637241781409));
#5440=CARTESIAN_POINT('Ctrl Pts',(7.1422713118924,-2.29563978953298,19.6000129141928));
#5441=CARTESIAN_POINT('Ctrl Pts',(7.0855648826377,-2.46505559387656,19.6399732294753));
#5442=CARTESIAN_POINT('Ctrl Pts',(7.0230580843623,-2.63185393661452,19.6831657242118));
#5443=CARTESIAN_POINT('Ctrl Pts',(6.96043766959649,-2.79895546305137,19.7264367284834));
#5444=CARTESIAN_POINT('Ctrl Pts',(6.89199600386832,-2.96342969182938,19.7729516729341));
#5445=CARTESIAN_POINT('Ctrl Pts',(6.81802018505874,-3.12483611668381,19.8222687573836));
#5446=CARTESIAN_POINT('Ctrl Pts',(6.79446991468079,-3.17622000140761,19.8379688968579));
#5447=CARTESIAN_POINT('Ctrl Pts',(6.77035908491064,-3.22729321641509,19.8539530256882));
#5448=CARTESIAN_POINT('Ctrl Pts',(6.74569781201533,-3.27804225551953,19.8702068896288));
#5449=CARTESIAN_POINT('Ctrl Pts',(6.63799263454312,-3.49968265042099,19.9411937080205));
#5450=CARTESIAN_POINT('Ctrl Pts',(6.51980121150529,-3.71512012776234,20.0173254587042));
#5451=CARTESIAN_POINT('Ctrl Pts',(6.39173197781128,-3.92374340698073,20.0969476480743));
#5452=CARTESIAN_POINT('Ctrl Pts',(6.24643834821673,-4.16042502504972,20.1872784524069));
#5453=CARTESIAN_POINT('Ctrl Pts',(6.08843156266247,-4.38833802903066,20.2821017096938));
#5454=CARTESIAN_POINT('Ctrl Pts',(5.91853733545478,-4.60661652504611,20.3790015676319));
#5455=CARTESIAN_POINT('Ctrl Pts',(5.73914601792361,-4.83709679287217,20.4813181293528));
#5456=CARTESIAN_POINT('Ctrl Pts',(5.5464996275473,-5.05683827770826,20.5859499447384));
#5457=CARTESIAN_POINT('Ctrl Pts',(5.34151401399943,-5.26481035159365,20.6900529536791));
#5458=CARTESIAN_POINT('Ctrl Pts',(5.15206615048807,-5.4570183040723,20.7862650355299));
#5459=CARTESIAN_POINT('Ctrl Pts',(4.95207643611402,-5.63917484269083,20.8820254389011));
#5460=CARTESIAN_POINT('Ctrl Pts',(4.74225084095691,-5.81042657310489,20.9750890530894));
#5461=CARTESIAN_POINT('Ctrl Pts',(4.72504179152039,-5.82447194965955,20.9827217555541));
#5462=CARTESIAN_POINT('Ctrl Pts',(4.70776658093554,-5.83844394397119,20.9903363177451));
#5463=CARTESIAN_POINT('Ctrl Pts',(4.69042560048463,-5.85234206846442,20.9979315010569));
#5464=CARTESIAN_POINT('Ctrl Pts',(4.53227676895431,-5.97909223436701,21.0671991742096));
#5465=CARTESIAN_POINT('Ctrl Pts',(4.36871099115427,-6.09965023465495,21.1348550392648));
#5466=CARTESIAN_POINT('Ctrl Pts',(4.20020516145961,-6.21355587418735,21.2001827671395));
#5467=CARTESIAN_POINT('Ctrl Pts',(4.03232824561985,-6.3270363840077,21.2652666725113));
#5468=CARTESIAN_POINT('Ctrl Pts',(3.85954822864127,-6.43391388412784,21.3280397868718));
#5469=CARTESIAN_POINT('Ctrl Pts',(3.6823763884026,-6.53376645849353,21.3877937718994));
#5470=CARTESIAN_POINT('Ctrl Pts',(3.50620389868854,-6.63305580722221,21.4472107102709));
#5471=CARTESIAN_POINT('Ctrl Pts',(3.32568916106491,-6.72539906465887,21.5036424824856));
#5472=CARTESIAN_POINT('Ctrl Pts',(3.14137181717059,-6.81041724905944,21.5563926690391));
#5473=CARTESIAN_POINT('Ctrl Pts',(2.95767572458469,-6.89514887519489,21.6089650583124));
#5474=CARTESIAN_POINT('Ctrl Pts',(2.77020278725585,-6.97260452982804,21.6578806380559));
#5475=CARTESIAN_POINT('Ctrl Pts',(2.57952150493091,-7.04244764308539,21.7024500070124));
#5476=CARTESIAN_POINT('Ctrl Pts',(2.38980714723273,-7.11193658929816,21.7467933694101));
#5477=CARTESIAN_POINT('Ctrl Pts',(2.196917093991,-7.17388983260061,21.7868344876134));
#5478=CARTESIAN_POINT('Ctrl Pts',(2.00144251249453,-7.2280168697354,21.8218943949161));
#5479=CARTESIAN_POINT('Ctrl Pts',(1.89911448599971,-7.25635156597884,21.8402477332167));
#5480=CARTESIAN_POINT('Ctrl Pts',(1.79607870623633,-7.2825422915802,21.8572360372855));
#5481=CARTESIAN_POINT('Ctrl Pts',(1.69242314334617,-7.30655212147743,21.872761906575));
#5482=CARTESIAN_POINT('Ctrl Pts',(1.53109479348353,-7.34392075013372,21.8969261945575));
#5483=CARTESIAN_POINT('Ctrl Pts',(1.3681702033035,-7.37602484342661,21.9175479596803));
#5484=CARTESIAN_POINT('Ctrl Pts',(1.20409713062058,-7.40271234751367,21.9346299924873));
#5485=CARTESIAN_POINT('Ctrl Pts',(1.04013459995097,-7.42938187125585,21.9517005165057));
#5486=CARTESIAN_POINT('Ctrl Pts',(0.875025527419233,-7.45064197717302,21.9652360762951));
#5487=CARTESIAN_POINT('Ctrl Pts',(0.709231910677198,-7.46639070079226,21.9752394567629));
#5488=CARTESIAN_POINT('Ctrl Pts',(0.543509118740266,-7.48213269676841,21.9852385639209));
#5489=CARTESIAN_POINT('Ctrl Pts',(0.377102774307521,-7.49236794293203,21.9917085089118));
#5490=CARTESIAN_POINT('Ctrl Pts',(0.210483412612377,-7.49704586707425,21.9946520730754));
#5491=CARTESIAN_POINT('Ctrl Pts',(0.043846333176655,-7.50172428865113,21.9975959502477));
#5492=CARTESIAN_POINT('Ctrl Pts',(-0.123003394892105,-7.50084417941287,
21.997012696586));
#5493=CARTESIAN_POINT('Ctrl Pts',(-0.289592115445145,-7.49440700834109,
21.9929050943176));
#5494=CARTESIAN_POINT('Ctrl Pts',(-0.456183318161168,-7.4879697413558,21.9887974308462));
#5495=CARTESIAN_POINT('Ctrl Pts',(-0.622513091568758,-7.47597527450695,
21.981165313742));
#5496=CARTESIAN_POINT('Ctrl Pts',(-0.788111005271544,-7.45847712628857,
21.9700115253567));
#5497=CARTESIAN_POINT('Ctrl Pts',(-0.953837293941331,-7.44096541313964,
21.9588490903214));
#5498=CARTESIAN_POINT('Ctrl Pts',(-1.11883017932857,-7.41794155647566,21.9441595217421));
#5499=CARTESIAN_POINT('Ctrl Pts',(-1.28262756847188,-7.38951057381989,21.9259456084462));
#5500=CARTESIAN_POINT('Ctrl Pts',(-1.42017866615189,-7.36563526730324,21.9106502256566));
#5501=CARTESIAN_POINT('Ctrl Pts',(-1.55688674308031,-7.33794777473905,21.8928694642867));
#5502=CARTESIAN_POINT('Ctrl Pts',(-1.69248640459601,-7.3065374679295,21.8726049758912));
#5503=CARTESIAN_POINT('Ctrl Pts',(-1.88273274116687,-7.2624688048201,21.844173896959));
#5504=CARTESIAN_POINT('Ctrl Pts',(-2.07088280936276,-7.21105234060234,21.8108538268066));
#5505=CARTESIAN_POINT('Ctrl Pts',(-2.25637490010937,-7.15253607541803,21.7732157763905));
#5506=CARTESIAN_POINT('Ctrl Pts',(-2.44228818762723,-7.09388693738798,21.7354922612775));
#5507=CARTESIAN_POINT('Ctrl Pts',(-2.62553116371187,-7.02810591273327,21.693431133967));
#5508=CARTESIAN_POINT('Ctrl Pts',(-2.80556734618175,-6.95548645790061,21.6476073040373));
#5509=CARTESIAN_POINT('Ctrl Pts',(-2.98633240777209,-6.8825730021419,21.6015979556612));
#5510=CARTESIAN_POINT('Ctrl Pts',(-3.16386441742821,-6.80276583871935,21.5517953762802));
#5511=CARTESIAN_POINT('Ctrl Pts',(-3.33765331847507,-6.716403079452,21.4987814863694));
#5512=CARTESIAN_POINT('Ctrl Pts',(-3.48618474969516,-6.64259178217798,21.4534723274095));
#5513=CARTESIAN_POINT('Ctrl Pts',(-3.63198249097864,-6.5639926901194,21.4058174549831));
#5514=CARTESIAN_POINT('Ctrl Pts',(-3.77474896103915,-6.48083870198402,21.3561801584053));
#5515=CARTESIAN_POINT('Ctrl Pts',(-4.01014670256992,-6.34373185190885,21.2743366589818));
#5516=CARTESIAN_POINT('Ctrl Pts',(-4.23726216824446,-6.19427134778842,21.1871036565295));
#5517=CARTESIAN_POINT('Ctrl Pts',(-4.45518879445125,-6.03334839088512,21.0965474453963));
#5518=CARTESIAN_POINT('Ctrl Pts',(-4.70496196761567,-5.84890907623891,20.9927578690687));
#5519=CARTESIAN_POINT('Ctrl Pts',(-4.94266540081088,-5.64941169864884,20.8846028468938));
#5520=CARTESIAN_POINT('Ctrl Pts',(-5.16700270581407,-5.43618276349407,20.775193369301));
#5521=CARTESIAN_POINT('Ctrl Pts',(-5.41937829936577,-5.19630389416685,20.6521095966433));
#5522=CARTESIAN_POINT('Ctrl Pts',(-5.65484050194211,-4.93904334303755,20.5274382025953));
#5523=CARTESIAN_POINT('Ctrl Pts',(-5.87159479072483,-4.66630202768028,20.405608498822));
#5524=CARTESIAN_POINT('Ctrl Pts',(-6.04218384490524,-4.45165029790822,20.3097265946877));
#5525=CARTESIAN_POINT('Ctrl Pts',(-6.20118676076994,-4.22740917015755,20.2156048161748));
#5526=CARTESIAN_POINT('Ctrl Pts',(-6.34773101513702,-3.99453513684228,20.1254023322322));
#5527=CARTESIAN_POINT('Ctrl Pts',(-6.49297957996139,-3.76372008871914,20.0359973849496));
#5528=CARTESIAN_POINT('Ctrl Pts',(-6.62598930102868,-3.52442256522106,19.9504427327492));
#5529=CARTESIAN_POINT('Ctrl Pts',(-6.74590126628717,-3.27762354542207,19.8708407777669));
#5530=CARTESIAN_POINT('Ctrl Pts',(-6.82733214648403,-3.11002507957565,19.8167839766326));
#5531=CARTESIAN_POINT('Ctrl Pts',(-6.90272398004706,-2.93895680522367,19.7654723313743));
#5532=CARTESIAN_POINT('Ctrl Pts',(-6.97175686004025,-2.76488811427908,19.7175734145484));
#5533=CARTESIAN_POINT('Ctrl Pts',(-7.04065596082013,-2.5911567520471,19.6697673213077));
#5534=CARTESIAN_POINT('Ctrl Pts',(-7.10322050225642,-2.41443685134032,19.6253607422239));
#5535=CARTESIAN_POINT('Ctrl Pts',(-7.15917310915023,-2.23522714577742,19.5850173762919));
#5536=CARTESIAN_POINT('Ctrl Pts',(-7.21512240740766,-2.0560280373928,19.5446763959776));
#5537=CARTESIAN_POINT('Ctrl Pts',(-7.26446033922906,-1.87433969536736,19.5083981482907));
#5538=CARTESIAN_POINT('Ctrl Pts',(-7.30695362166136,-1.69068884508356,19.4768462144938));
#5539=CARTESIAN_POINT('Ctrl Pts',(-7.34944690409365,-1.50703799479976,19.4452942806969));
#5540=CARTESIAN_POINT('Ctrl Pts',(-7.38509535231297,-1.32142493703578,19.4184686607899));
#5541=CARTESIAN_POINT('Ctrl Pts',(-7.41371272123842,-1.13440014410596,19.3970329360355));
#5542=CARTESIAN_POINT('Ctrl Pts',(-7.43818802515262,-0.974445234960639,
19.3786998083692));
#5543=CARTESIAN_POINT('Ctrl Pts',(-7.45752405553203,-0.813425201482107,
19.364309229696));
#5544=CARTESIAN_POINT('Ctrl Pts',(-7.47162453316991,-0.651787415752647,
19.3538503606095));
#5545=CARTESIAN_POINT('Ctrl Pts',(-7.48571915884413,-0.490216712747107,
19.3433958321506));
#5546=CARTESIAN_POINT('Ctrl Pts',(-7.49458250514591,-0.328029183151691,
19.3368697504885));
#5547=CARTESIAN_POINT('Ctrl Pts',(-7.49816978215991,-0.165680167503408,
19.3342612897069));
#5548=CARTESIAN_POINT('Ctrl Pts',(-7.49938932726501,-0.110487343927736,
19.3333745069004));
#5549=CARTESIAN_POINT('Ctrl Pts',(-7.4999995298899,-0.0552759010908673,
19.3329405052157));
#5550=CARTESIAN_POINT('Ctrl Pts',(-7.49999999972844,-6.38227930839602E-5,
19.332958859286));
#5551=CARTESIAN_POINT('Ctrl Pts',(-7.49999999972845,-6.38221443329073E-5,
19.3329588592862));
#5552=CARTESIAN_POINT('Ctrl Pts',(-7.50000137686945,0.161769623405833,19.3330126573518));
#5553=CARTESIAN_POINT('Ctrl Pts',(-7.4947604010034,0.323599227211819,19.3369528643072));
#5554=CARTESIAN_POINT('Ctrl Pts',(-7.48430383616557,0.48497019285453,19.3447687682629));
#5555=CARTESIAN_POINT('Ctrl Pts',(-7.47384231895815,0.646417585954605,19.3525883739357));
#5556=CARTESIAN_POINT('Ctrl Pts',(-7.45816032347053,0.807405489160749,19.3642873486424));
#5557=CARTESIAN_POINT('Ctrl Pts',(-7.43733642357596,0.967484843576559,19.3798549652665));
#5558=CARTESIAN_POINT('Ctrl Pts',(-7.43007828607042,1.02328025039424,19.385281033518));
#5559=CARTESIAN_POINT('Ctrl Pts',(-7.42219593523814,1.07896536718678,19.3911770876185));
#5560=CARTESIAN_POINT('Ctrl Pts',(-7.4136941505238,1.13452150375796,19.3975426733416));
#5561=CARTESIAN_POINT('Ctrl Pts',(-7.38485140438262,1.32299858210651,19.4191382534722));
#5562=CARTESIAN_POINT('Ctrl Pts',(-7.34886996628597,1.5100294373421,19.4461378648968));
#5563=CARTESIAN_POINT('Ctrl Pts',(-7.30594116139313,1.69505862620195,19.4778961232255));
#5564=CARTESIAN_POINT('Ctrl Pts',(-7.26293850090524,1.88040614306737,19.5097090191122));
#5565=CARTESIAN_POINT('Ctrl Pts',(-7.21296472182939,2.06374480770197,19.546296949735));
#5566=CARTESIAN_POINT('Ctrl Pts',(-7.15625861648385,2.2445406242705,19.5870111939725));
#5567=CARTESIAN_POINT('Ctrl Pts',(-7.09936154725929,2.42594529010196,19.6278625477851));
#5568=CARTESIAN_POINT('Ctrl Pts',(-7.03568692374006,2.60478967078624,19.6728680536135));
#5569=CARTESIAN_POINT('Ctrl Pts',(-6.96551997668802,2.78056315417582,19.7213724143269));
#5570=CARTESIAN_POINT('Ctrl Pts',(-6.89820683644311,2.94918763672547,19.7679040217627));
#5571=CARTESIAN_POINT('Ctrl Pts',(-6.82491919803976,3.11498593049364,19.8176556633038));
#5572=CARTESIAN_POINT('Ctrl Pts',(-6.7459440810335,3.27753542399913,19.8700487900425));
#5573=CARTESIAN_POINT('Ctrl Pts',(-6.63072214042775,3.51468946436221,19.9464885341807));
#5574=CARTESIAN_POINT('Ctrl Pts',(-6.50338764282049,3.74495378726884,20.0285508887797));
#5575=CARTESIAN_POINT('Ctrl Pts',(-6.36470549534165,3.96743291784093,20.1143153130233));
#5576=CARTESIAN_POINT('Ctrl Pts',(-6.2136393301195,4.20977895666768,20.207738316045));
#5577=CARTESIAN_POINT('Ctrl Pts',(-6.0491079526643,4.44288805980257,20.3055540831348));
#5578=CARTESIAN_POINT('Ctrl Pts',(-5.87210066028485,4.66566542258253,20.4052802616237));
#5579=CARTESIAN_POINT('Ctrl Pts',(-5.67438099506923,4.91451090795411,20.5166758225579));
#5580=CARTESIAN_POINT('Ctrl Pts',(-5.46109323358007,5.15046648299211,20.6304550435319));
#5581=CARTESIAN_POINT('Ctrl Pts',(-5.23363288347398,5.37206541667354,20.7431582152801));
#5582=CARTESIAN_POINT('Ctrl Pts',(-5.01495184833834,5.58511126919161,20.8515113689153));
#5583=CARTESIAN_POINT('Ctrl Pts',(-4.78316943962577,5.78488927769216,20.9588699351008));
#5584=CARTESIAN_POINT('Ctrl Pts',(-4.53956528780731,5.97012118786,21.0621595457893));
#5585=CARTESIAN_POINT('Ctrl Pts',(-4.3266267571509,6.13203554969409,21.1524467505347));
#5586=CARTESIAN_POINT('Ctrl Pts',(-4.10465503258614,6.28283627218151,21.2396249456005));
#5587=CARTESIAN_POINT('Ctrl Pts',(-3.87454829813565,6.42167232778302,21.3216407735323));
#5588=CARTESIAN_POINT('Ctrl Pts',(-3.84141025626157,6.44166633202258,21.3334520051629));
#5589=CARTESIAN_POINT('Ctrl Pts',(-3.8081035883213,6.46141219329767,21.3451561726828));
#5590=CARTESIAN_POINT('Ctrl Pts',(-3.77463107174321,6.48090736488578,21.3567471433162));
#5591=CARTESIAN_POINT('Ctrl Pts',(-3.59538368742212,6.58530520739359,21.4188175037246));
#5592=CARTESIAN_POINT('Ctrl Pts',(-3.41138061249562,6.68250937266347,21.4776417528438));
#5593=CARTESIAN_POINT('Ctrl Pts',(-3.22316644017786,6.77208964049585,21.5326304570881));
#5594=CARTESIAN_POINT('Ctrl Pts',(-3.03610753231628,6.86112006185212,21.5872816389518));
#5595=CARTESIAN_POINT('Ctrl Pts',(-2.8448891541714,6.9426196918104,21.6381442168227));
#5596=CARTESIAN_POINT('Ctrl Pts',(-2.65008522422012,7.0161989926434,21.6846395445151));
#5597=CARTESIAN_POINT('Ctrl Pts',(-2.45716260701487,7.08906770372322,21.7306858450619));
#5598=CARTESIAN_POINT('Ctrl Pts',(-2.26072348245475,7.15416815105665,21.7724488412702));
#5599=CARTESIAN_POINT('Ctrl Pts',(-2.06136233189299,7.2111570040218,21.8093664903413));
#5600=CARTESIAN_POINT('Ctrl Pts',(-1.93952212373797,7.24598592474294,21.8319288302693));
#5601=CARTESIAN_POINT('Ctrl Pts',(-1.81659123049385,7.2777857918624,21.8526813930556));
#5602=CARTESIAN_POINT('Ctrl Pts',(-1.69271195884026,7.30648521687406,21.871495880758));
#5603=CARTESIAN_POINT('Ctrl Pts',(-1.54076476717671,7.34168720809236,21.8945732570681));
#5604=CARTESIAN_POINT('Ctrl Pts',(-1.3873755369066,7.37222456154265,21.9147348270972));
#5605=CARTESIAN_POINT('Ctrl Pts',(-1.23296187718936,7.39795951660981,21.9318611863869));
#5606=CARTESIAN_POINT('Ctrl Pts',(-1.07863059043489,7.4236807431992,21.9489784095097));
#5607=CARTESIAN_POINT('Ctrl Pts',(-0.923276373536958,7.44460457864745,21.9630636593349));
#5608=CARTESIAN_POINT('Ctrl Pts',(-0.767329781169641,7.46064373944569,21.9739977223933));
#5609=CARTESIAN_POINT('Ctrl Pts',(-0.611426078689014,7.4766784890043,21.9849287782638));
#5610=CARTESIAN_POINT('Ctrl Pts',(-0.454930745505132,7.4878311887663,21.9927103804668));
#5611=CARTESIAN_POINT('Ctrl Pts',(-0.298281394079239,7.49406619999758,21.9972234138677));
#5612=CARTESIAN_POINT('Ctrl Pts',(-0.141560740138866,7.500304049236,22.0017385014785));
#5613=CARTESIAN_POINT('Ctrl Pts',(0.0153136481942017,7.50161972110047,22.0029820440832));
#5614=CARTESIAN_POINT('Ctrl Pts',(0.171902471705738,7.49802971054539,22.0008347638195));
#5615=CARTESIAN_POINT('Ctrl Pts',(0.305568621085933,7.49496523329619,21.9990018189256));
#5616=CARTESIAN_POINT('Ctrl Pts',(0.439026530392158,7.48832709367931,21.9946981373927));
#5617=CARTESIAN_POINT('Ctrl Pts',(0.572005831492304,7.47815547636841,21.9878495298179));
#5618=CARTESIAN_POINT('Ctrl Pts',(0.768094469245658,7.4631566113891,21.9777507090335));
#5619=CARTESIAN_POINT('Ctrl Pts',(0.963317829131666,7.44046192620981,21.9621182351183));
#5620=CARTESIAN_POINT('Ctrl Pts',(1.15706933924185,7.41020853580966,21.9414600255889));
#5621=CARTESIAN_POINT('Ctrl Pts',(1.35121737676857,7.37989322951153,21.9207595374395));
#5622=CARTESIAN_POINT('Ctrl Pts',(1.54388725002921,7.34198837015578,21.8950127215142));
#5623=CARTESIAN_POINT('Ctrl Pts',(1.73448713276613,7.29668105279851,21.8647306201931));
#5624=CARTESIAN_POINT('Ctrl Pts',(1.92549417720536,7.25127694941914,21.8343838298924));
#5625=CARTESIAN_POINT('Ctrl Pts',(2.11442210634573,7.19843887574435,21.79948235684));
#5626=CARTESIAN_POINT('Ctrl Pts',(2.30069800903712,7.13840238927539,21.7605405255016));
#5627=CARTESIAN_POINT('Ctrl Pts',(2.48738865405972,7.0782322318807,21.7215119903777));
#5628=CARTESIAN_POINT('Ctrl Pts',(2.67141519319667,7.01083174340814,21.6784250852651));
#5629=CARTESIAN_POINT('Ctrl Pts',(2.85222764907197,6.93648307414279,21.6317975777061));
#5630=CARTESIAN_POINT('Ctrl Pts',(3.03371105458721,6.86185851562726,21.5849970471701));
#5631=CARTESIAN_POINT('Ctrl Pts',(3.21195623090598,6.78023430023224,21.5346295888609));
#5632=CARTESIAN_POINT('Ctrl Pts',(3.38643781016122,6.69193835580622,21.4812187556522));
#5633=CARTESIAN_POINT('Ctrl Pts',(3.56127443599491,6.60346274099269,21.4276992385717));
#5634=CARTESIAN_POINT('Ctrl Pts',(3.73233191190736,6.50828843639492,21.3711239482717));
#5635=CARTESIAN_POINT('Ctrl Pts',(3.89911599643454,6.40678503200695,21.3120196402132));
#5636=CARTESIAN_POINT('Ctrl Pts',(4.0664769606818,6.30493054342724,21.2527108997186));
#5637=CARTESIAN_POINT('Ctrl Pts',(4.229534712043,6.19670332730237,21.190855616266));
#5638=CARTESIAN_POINT('Ctrl Pts',(4.38782764842825,6.08251333970495,21.1269860301346));
#5639=CARTESIAN_POINT('Ctrl Pts',(4.49080837173162,6.00822469622331,21.0854343581075));
#5640=CARTESIAN_POINT('Ctrl Pts',(4.59177320403997,5.93141309365973,21.0430301484942));
#5641=CARTESIAN_POINT('Ctrl Pts',(4.69060418288513,5.85219893710907,20.9999199530233));
#5642=CARTESIAN_POINT('Ctrl Pts',(4.90988924268625,5.67643946108971,20.9042675381394));
#5643=CARTESIAN_POINT('Ctrl Pts',(5.11865959298013,5.48887002871858,20.8051395384096));
#5644=CARTESIAN_POINT('Ctrl Pts',(5.31613179428595,5.29043880465336,20.7051913113127));
#5645=CARTESIAN_POINT('Ctrl Pts',(5.51624645380641,5.08935228928837,20.603905635137));
#5646=CARTESIAN_POINT('Ctrl Pts',(5.70476104395003,4.87710926925346,20.5017776331107));
#5647=CARTESIAN_POINT('Ctrl Pts',(5.88083921476348,4.65464608000438,20.4015706928499));
#5648=CARTESIAN_POINT('Ctrl Pts',(6.04863046411871,4.44265287103811,20.3060798797483));
#5649=CARTESIAN_POINT('Ctrl Pts',(6.20512960953633,4.22137645327274,20.2123335583494));
#5650=CARTESIAN_POINT('Ctrl Pts',(6.34956762900155,3.99161507722572,20.1227230237679));
#5651=CARTESIAN_POINT('Ctrl Pts',(6.4782693500351,3.78688584711183,20.0428754180885));
#5652=CARTESIAN_POINT('Ctrl Pts',(6.59739471133209,3.57541842759605,19.966311514912));
#5653=CARTESIAN_POINT('Ctrl Pts',(6.70635739485687,3.35779250288766,19.8947230855874));
#5654=CARTESIAN_POINT('Ctrl Pts',(6.71968021052779,3.33118348421894,19.8859700022637));
#5655=CARTESIAN_POINT('Ctrl Pts',(6.73285104073735,3.30448243080959,19.8772913014631));
#5656=CARTESIAN_POINT('Ctrl Pts',(6.74586876681577,3.27769043396406,19.8686900755905));
#5657=CARTESIAN_POINT('Ctrl Pts',(6.82430646662419,3.11625650969972,19.8168637912674));
#5658=CARTESIAN_POINT('Ctrl Pts',(6.89715640692234,2.9515711207856,19.7678503184023));
#5659=CARTESIAN_POINT('Ctrl Pts',(6.96411695834188,2.78407524871995,19.7220840532085));
#5660=CARTESIAN_POINT('Ctrl Pts',(7.03097289981926,2.61684104913335,19.6763892869234));
#5661=CARTESIAN_POINT('Ctrl Pts',(7.09195760838124,2.44680543583005,19.633931590255));
#5662=CARTESIAN_POINT('Ctrl Pts',(7.14681265559779,2.27443814287996,19.5951433266732));
#5663=CARTESIAN_POINT('Ctrl Pts',(7.20159314251032,2.10230513571426,19.5564077850354));
#5664=CARTESIAN_POINT('Ctrl Pts',(7.25026042307138,1.92784710265306,19.5213317080993));
#5665=CARTESIAN_POINT('Ctrl Pts',(7.29260203951382,1.75155801881608,19.4903456986937));
#5666=CARTESIAN_POINT('Ctrl Pts',(7.33488204075116,1.57552546954176,19.4594047798984));
#5667=CARTESIAN_POINT('Ctrl Pts',(7.37085461729061,1.39766753541784,19.4325420336229));
#5668=CARTESIAN_POINT('Ctrl Pts',(7.40035570833137,1.21849718512899,19.4101861855999));
#5669=CARTESIAN_POINT('Ctrl Pts',(7.42983195743503,1.03947770853382,19.3878491627305));
#5670=CARTESIAN_POINT('Ctrl Pts',(7.45284749385224,0.859148380629525,19.3700114510759));
#5671=CARTESIAN_POINT('Ctrl Pts',(7.46928819351229,0.678036785327972,19.3571006942315));
#5672=CARTESIAN_POINT('Ctrl Pts',(7.48571612175541,0.497065880613931,19.3441999666841));
#5673=CARTESIAN_POINT('Ctrl Pts',(7.49557934457186,0.315314290784328,19.3362185422342));
#5674=CARTESIAN_POINT('Ctrl Pts',(7.49881497880803,0.133318841895481,19.3335830686486));
#5675=CARTESIAN_POINT('Ctrl Pts',(7.49960484421833,0.0888911039569122,19.3329397111881));
#5676=CARTESIAN_POINT('Ctrl Pts',(7.5,0.0444488682210776,19.3326149291812));
#5677=CARTESIAN_POINT('Ctrl Pts',(7.5,1.83697019872103E-15,19.3326149291812));
#5678=CARTESIAN_POINT('Ctrl Pts',(9.06818181818182,-2.77555756156289E-16,
16.6963492570201));
#5679=CARTESIAN_POINT('Ctrl Pts',(9.06818181818182,-1.59578114831733,16.6963492570201));
#5680=CARTESIAN_POINT('Ctrl Pts',(8.41792693003091,-4.7680728734062,17.0694389926071));
#5681=CARTESIAN_POINT('Ctrl Pts',(5.86812439794336,-8.45147311504401,18.176238977512));
#5682=CARTESIAN_POINT('Ctrl Pts',(2.13637643354675,-10.5855566851176,19.0330683300942));
#5683=CARTESIAN_POINT('Ctrl Pts',(-1.66033921810787,-10.5859872665705,19.0322636243943));
#5684=CARTESIAN_POINT('Ctrl Pts',(-5.48966678697824,-8.80610845315595,18.3204282727391));
#5685=CARTESIAN_POINT('Ctrl Pts',(-7.9972027779537,-5.6823888865083,17.2720041386699));
#5686=CARTESIAN_POINT('Ctrl Pts',(-9.10276599747076,-1.62090974430359,16.6774277042663));
#5687=CARTESIAN_POINT('Ctrl Pts',(-9.10168338064412,1.6211254766953,16.678827094141));
#5688=CARTESIAN_POINT('Ctrl Pts',(-7.99795456455011,5.6815718382537,17.2694619372668));
#5689=CARTESIAN_POINT('Ctrl Pts',(-5.48802720874369,8.80873683615948,18.3244182502819));
#5690=CARTESIAN_POINT('Ctrl Pts',(-2.08802932955049,10.3840276033752,18.9482929035547));
#5691=CARTESIAN_POINT('Ctrl Pts',(1.64285450861998,10.7207692947679,19.0979776863544));
#5692=CARTESIAN_POINT('Ctrl Pts',(5.59169260247156,8.86861695682125,18.3071970067273));
#5693=CARTESIAN_POINT('Ctrl Pts',(8.41406720829093,4.76388507099759,17.0652606363946));
#5694=CARTESIAN_POINT('Ctrl Pts',(9.06818181818182,1.59578114831733,16.6963492570201));
#5695=CARTESIAN_POINT('Ctrl Pts',(9.06818181818182,-2.77555756156289E-16,
16.6963492570201));
#5696=CARTESIAN_POINT('Ctrl Pts',(8.52925489606833,-2.04324230714416E-16,
16.9890532033264));
#5697=CARTESIAN_POINT('Ctrl Pts',(8.52925489606833,-1.48962154953277,16.9890532033264));
#5698=CARTESIAN_POINT('Ctrl Pts',(7.87687500329371,-4.44985072056414,17.3363463617318));
#5699=CARTESIAN_POINT('Ctrl Pts',(5.37101016546914,-7.81747651588321,18.3271776375016));
#5700=CARTESIAN_POINT('Ctrl Pts',(1.90652317397209,-9.67880593256366,19.027936254452));
#5701=CARTESIAN_POINT('Ctrl Pts',(-1.48242488666645,-9.67656253638176,19.0242925274118));
#5702=CARTESIAN_POINT('Ctrl Pts',(-5.00803293593842,-8.13057125719761,18.4491055978167));
#5703=CARTESIAN_POINT('Ctrl Pts',(-7.45861508030558,-5.2962344172881,17.5218568938428));
#5704=CARTESIAN_POINT('Ctrl Pts',(-8.56396284436833,-1.5139035461346,16.9719681314427));
#5705=CARTESIAN_POINT('Ctrl Pts',(-8.56304269786486,1.51420311672056,16.9729380768753));
#5706=CARTESIAN_POINT('Ctrl Pts',(-7.45892636451772,5.29539679129704,17.5194393239992));
#5707=CARTESIAN_POINT('Ctrl Pts',(-5.00753889620558,8.13267896507007,18.4521891181082));
#5708=CARTESIAN_POINT('Ctrl Pts',(-1.87388181025726,9.50233127388934,18.9572985482202));
#5709=CARTESIAN_POINT('Ctrl Pts',(1.46541943459002,9.79166364559922,19.0778999502934));
#5710=CARTESIAN_POINT('Ctrl Pts',(5.0943002984368,8.19665431249147,18.4428143198929));
#5711=CARTESIAN_POINT('Ctrl Pts',(7.87606641456947,4.44699289538305,17.3333349814256));
#5712=CARTESIAN_POINT('Ctrl Pts',(8.52925489606833,1.48962154953272,16.9890532033264));
#5713=CARTESIAN_POINT('Ctrl Pts',(8.52925489606833,-2.41380287841585E-16,
16.9890532033264));
#5714=CARTESIAN_POINT('Ctrl Pts',(7.75033632345811,-4.50174017686739E-17,
17.7987073905814));
#5715=CARTESIAN_POINT('Ctrl Pts',(7.75033632345811,-1.30455312354164,17.7987073905814));
#5716=CARTESIAN_POINT('Ctrl Pts',(7.10826290029318,-3.89360315842007,18.1503268520871));
#5717=CARTESIAN_POINT('Ctrl Pts',(4.70053765930092,-6.71224153203073,19.133184606454));
#5718=CARTESIAN_POINT('Ctrl Pts',(1.60333612140186,-8.1097961186631,19.7809692603298));
#5719=CARTESIAN_POINT('Ctrl Pts',(-1.24739767962264,-8.10458971579584,19.7768036158037));
#5720=CARTESIAN_POINT('Ctrl Pts',(-4.36061605167524,-6.95356866926854,19.2482436597623));
#5721=CARTESIAN_POINT('Ctrl Pts',(-6.70160515983065,-4.62154273010426,18.3373097614389));
#5722=CARTESIAN_POINT('Ctrl Pts',(-7.78395626574493,-1.32716243511598,17.7808035499084));
#5723=CARTESIAN_POINT('Ctrl Pts',(-7.78335904380905,1.32737409349607,17.7818079474956));
#5724=CARTESIAN_POINT('Ctrl Pts',(-6.70129128714702,4.62079718556549,18.3348534089681));
#5725=CARTESIAN_POINT('Ctrl Pts',(-4.36163002862514,6.95584707246026,19.2523271250457));
#5726=CARTESIAN_POINT('Ctrl Pts',(-1.59115196857109,7.97628900960331,19.7149140395441));
#5727=CARTESIAN_POINT('Ctrl Pts',(1.2323404820187,8.1853538169283,19.8249773268813));
#5728=CARTESIAN_POINT('Ctrl Pts',(4.42748256065924,7.02563177285682,19.2467581349916));
#5729=CARTESIAN_POINT('Ctrl Pts',(7.11158331347841,3.89285136784028,18.1476536477004));
#5730=CARTESIAN_POINT('Ctrl Pts',(7.75033632345811,1.30455312354152,17.7987073905814));
#5731=CARTESIAN_POINT('Ctrl Pts',(7.75033632345811,-1.62495706346568E-16,
17.7987073905814));
#5732=CARTESIAN_POINT('Ctrl Pts',(7.49997898926977,1.18727990181773E-16,
18.8727417166749));
#5733=CARTESIAN_POINT('Ctrl Pts',(7.49997898926977,-1.17773001028884,18.8727417166749));
#5734=CARTESIAN_POINT('Ctrl Pts',(6.92434994470585,-3.5173122090396,19.2806044731049));
#5735=CARTESIAN_POINT('Ctrl Pts',(4.71974380892434,-6.14234789882435,20.4728855461179));
#5736=CARTESIAN_POINT('Ctrl Pts',(1.6753432303372,-7.55890683324212,21.3625000258593));
#5737=CARTESIAN_POINT('Ctrl Pts',(-1.30266100196853,-7.55659632853009,21.3607622545602));
#5738=CARTESIAN_POINT('Ctrl Pts',(-4.40054398399628,-6.38168901511819,20.6242901562785));
#5739=CARTESIAN_POINT('Ctrl Pts',(-6.55612322809675,-4.18225627169105,19.5009453626012));
#5740=CARTESIAN_POINT('Ctrl Pts',(-7.53043693696764,-1.19744723403944,18.851946280041));
#5741=CARTESIAN_POINT('Ctrl Pts',(-7.52965797516887,1.19768815648017,18.8534063249902));
#5742=CARTESIAN_POINT('Ctrl Pts',(-6.55645674912434,4.18156062850628,19.4981462935819));
#5743=CARTESIAN_POINT('Ctrl Pts',(-4.40001770889782,6.38344201396891,20.628879238981));
#5744=CARTESIAN_POINT('Ctrl Pts',(-1.64701789222801,7.42449614751224,21.2739304159005));
#5745=CARTESIAN_POINT('Ctrl Pts',(1.28815795162506,7.64293786766958,21.4284314886368));
#5746=CARTESIAN_POINT('Ctrl Pts',(4.47613818554217,6.43700979105439,20.6131496315766));
#5747=CARTESIAN_POINT('Ctrl Pts',(6.92370291988582,3.51549848232719,19.2763960689845));
#5748=CARTESIAN_POINT('Ctrl Pts',(7.49997898926977,1.17773001028865,18.8727417166749));
#5749=CARTESIAN_POINT('Ctrl Pts',(7.49997898926977,-8.11489720641551E-17,
18.8727417166749));
#5750=CARTESIAN_POINT('Ctrl Pts',(7.50000000308588,1.82342057246943E-16,
19.3327500340666));
#5751=CARTESIAN_POINT('Ctrl Pts',(7.50000000308588,-1.13983254637561,19.3327500340666));
#5752=CARTESIAN_POINT('Ctrl Pts',(6.96220632038699,-3.40573356596564,19.7647557660862));
#5753=CARTESIAN_POINT('Ctrl Pts',(4.85337521228726,-6.03673548829487,21.0463398717424));
#5754=CARTESIAN_POINT('Ctrl Pts',(1.76695478202178,-7.56111255891257,22.0384881837842));
#5755=CARTESIAN_POINT('Ctrl Pts',(-1.37323361305111,-7.56142088620697,22.037556656091));
#5756=CARTESIAN_POINT('Ctrl Pts',(-4.54036697665852,-6.29005054782313,21.2133004666028));
#5757=CARTESIAN_POINT('Ctrl Pts',(-6.61424492839959,-4.05881294736392,19.999309056778));
#5758=CARTESIAN_POINT('Ctrl Pts',(-7.52860291482921,-1.15778102404128,19.3108405405169));
#5759=CARTESIAN_POINT('Ctrl Pts',(-7.52770748324762,1.15793509310074,19.3124609337831));
#5760=CARTESIAN_POINT('Ctrl Pts',(-6.61486679147359,4.05822937438032,19.9963654126915));
#5761=CARTESIAN_POINT('Ctrl Pts',(-4.53901069073959,6.29192800079645,21.2179204496805));
#5762=CARTESIAN_POINT('Ctrl Pts',(-1.72696502969537,7.41716041273811,21.9403243457452));
#5763=CARTESIAN_POINT('Ctrl Pts',(1.35877258747706,7.6576966809742,22.1136490964728));
#5764=CARTESIAN_POINT('Ctrl Pts',(4.62475181174631,6.33469634386154,21.1979788253294));
#5765=CARTESIAN_POINT('Ctrl Pts',(6.95901332159314,3.40274193259946,19.7599174844227));
#5766=CARTESIAN_POINT('Ctrl Pts',(7.50000000308588,1.13983254637542,19.3327500340666));
#5767=CARTESIAN_POINT('Ctrl Pts',(7.50000000308588,-4.94995460683127E-17,
19.3327500340666));
#5768=CARTESIAN_POINT('',(9.06818181818182,-2.77555756156289E-16,16.6963492570201));
#5769=CARTESIAN_POINT('Ctrl Pts',(9.06818181818182,-2.77555756156289E-16,
16.6963492570201));
#5770=CARTESIAN_POINT('Ctrl Pts',(8.52925489606833,-2.04324230714416E-16,
16.9890532033264));
#5771=CARTESIAN_POINT('Ctrl Pts',(7.75036900658895,-4.50240862234006E-17,
17.7986734177958));
#5772=CARTESIAN_POINT('Ctrl Pts',(7.49999999999984,1.1871424879926E-16,
18.8726515849863));
#5773=CARTESIAN_POINT('Ctrl Pts',(7.5,1.82323373546833E-16,19.3326149291822));
#5774=CARTESIAN_POINT('Ctrl Pts',(9.06818181818182,-2.77555756156289E-16,
16.6963492570201));
#5775=CARTESIAN_POINT('Ctrl Pts',(9.06818181818182,1.59578114831733,16.6963492570201));
#5776=CARTESIAN_POINT('Ctrl Pts',(8.41406720829093,4.76388507099759,17.0652606363946));
#5777=CARTESIAN_POINT('Ctrl Pts',(5.59169260247156,8.86861695682125,18.3071970067273));
#5778=CARTESIAN_POINT('Ctrl Pts',(1.64285450861998,10.7207692947679,19.0979776863544));
#5779=CARTESIAN_POINT('Ctrl Pts',(-2.08802932955049,10.3840276033752,18.9482929035547));
#5780=CARTESIAN_POINT('Ctrl Pts',(-5.48802720874369,8.80873683615948,18.3244182502819));
#5781=CARTESIAN_POINT('Ctrl Pts',(-7.99795456455011,5.6815718382537,17.2694619372668));
#5782=CARTESIAN_POINT('Ctrl Pts',(-9.10168338064412,1.6211254766953,16.678827094141));
#5783=CARTESIAN_POINT('Ctrl Pts',(-9.10276599747076,-1.62090974430359,16.6774277042663));
#5784=CARTESIAN_POINT('Ctrl Pts',(-7.9972027779537,-5.6823888865083,17.2720041386699));
#5785=CARTESIAN_POINT('Ctrl Pts',(-5.48966678697824,-8.80610845315595,18.3204282727391));
#5786=CARTESIAN_POINT('Ctrl Pts',(-1.66033921810787,-10.5859872665705,19.0322636243943));
#5787=CARTESIAN_POINT('Ctrl Pts',(2.13637643354675,-10.5855566851176,19.0330683300942));
#5788=CARTESIAN_POINT('Ctrl Pts',(5.86812439794336,-8.45147311504401,18.176238977512));
#5789=CARTESIAN_POINT('Ctrl Pts',(8.41792693003091,-4.7680728734062,17.0694389926071));
#5790=CARTESIAN_POINT('Ctrl Pts',(9.06818181818182,-1.59578114831733,16.6963492570201));
#5791=CARTESIAN_POINT('Ctrl Pts',(9.06818181818182,-2.77555756156289E-16,
16.6963492570201));
#5792=CARTESIAN_POINT('Origin',(0.,0.,0.));
#5793=CARTESIAN_POINT('',(-19.,20.,2.32682891837997E-15));
#5794=CARTESIAN_POINT('Origin',(0.,20.,0.));
#5795=CARTESIAN_POINT('',(-19.,-20.,2.32682891837997E-15));
#5796=CARTESIAN_POINT('',(-19.,0.,2.32682891837997E-15));
#5797=CARTESIAN_POINT('Origin',(0.,-20.,0.));
#5798=CARTESIAN_POINT('Origin',(0.,0.,0.));
#5799=CARTESIAN_POINT('',(6.,6.93889390390723E-16,10.3923048454133));
#5800=CARTESIAN_POINT('',(-6.,-7.34788079488412E-16,10.3923048454133));
#5801=CARTESIAN_POINT('Ctrl Pts',(6.,5.55111512312578E-16,10.3923048454133));
#5802=CARTESIAN_POINT('Ctrl Pts',(6.,0.769830401762947,10.3923048454133));
#5803=CARTESIAN_POINT('Ctrl Pts',(5.84331350686056,1.57883160757971,10.4869526157176));
#5804=CARTESIAN_POINT('Ctrl Pts',(5.22737225841736,3.05149415704693,10.8071760747641));
#5805=CARTESIAN_POINT('Ctrl Pts',(4.76853496878621,3.71674640545236,11.026202805293));
#5806=CARTESIAN_POINT('Ctrl Pts',(3.71818001883758,4.76710135540099,11.423199660423));
#5807=CARTESIAN_POINT('Ctrl Pts',(3.05244454868625,5.22699047954748,11.6295890462369));
#5808=CARTESIAN_POINT('Ctrl Pts',(1.57767045293313,5.84378343521477,11.9195518101039));
#5809=CARTESIAN_POINT('Ctrl Pts',(0.767731806652134,6.,12.));
#5810=CARTESIAN_POINT('Ctrl Pts',(-0.767731806652134,6.,12.));
#5811=CARTESIAN_POINT('Ctrl Pts',(-1.57767045293313,5.84378343521477,11.9195518101039));
#5812=CARTESIAN_POINT('Ctrl Pts',(-3.05244454868625,5.22699047954748,11.6295890462369));
#5813=CARTESIAN_POINT('Ctrl Pts',(-3.71818001883758,4.76710135540099,11.423199660423));
#5814=CARTESIAN_POINT('Ctrl Pts',(-4.76853496878621,3.71674640545236,11.026202805293));
#5815=CARTESIAN_POINT('Ctrl Pts',(-5.22737225841736,3.05149415704693,10.8071760747641));
#5816=CARTESIAN_POINT('Ctrl Pts',(-5.84331350686056,1.57883160757971,10.4869526157176));
#5817=CARTESIAN_POINT('Ctrl Pts',(-6.,0.769830401762947,10.3923048454133));
#5818=CARTESIAN_POINT('Ctrl Pts',(-6.,5.55111512312578E-16,10.3923048454133));
#5819=CARTESIAN_POINT('Ctrl Pts',(-6.,-2.77555756156289E-16,10.3923048454133));
#5820=CARTESIAN_POINT('Ctrl Pts',(-6.,-0.769830401762946,10.3923048454133));
#5821=CARTESIAN_POINT('Ctrl Pts',(-5.84331350686056,-1.57883160757971,10.4869526157176));
#5822=CARTESIAN_POINT('Ctrl Pts',(-5.22737225841736,-3.05149415704693,10.8071760747641));
#5823=CARTESIAN_POINT('Ctrl Pts',(-4.76853496878621,-3.71674640545236,11.026202805293));
#5824=CARTESIAN_POINT('Ctrl Pts',(-3.71818001883758,-4.76710135540099,11.423199660423));
#5825=CARTESIAN_POINT('Ctrl Pts',(-3.05244454868625,-5.22699047954748,11.6295890462369));
#5826=CARTESIAN_POINT('Ctrl Pts',(-1.57767045293313,-5.84378343521477,11.9195518101039));
#5827=CARTESIAN_POINT('Ctrl Pts',(-0.767731806652135,-6.,12.));
#5828=CARTESIAN_POINT('Ctrl Pts',(0.767731806652132,-6.,12.));
#5829=CARTESIAN_POINT('Ctrl Pts',(1.57767045293313,-5.84378343521477,11.9195518101039));
#5830=CARTESIAN_POINT('Ctrl Pts',(3.05244454868625,-5.22699047954749,11.6295890462369));
#5831=CARTESIAN_POINT('Ctrl Pts',(3.71818001883758,-4.767101355401,11.423199660423));
#5832=CARTESIAN_POINT('Ctrl Pts',(4.76853496878621,-3.71674640545237,11.026202805293));
#5833=CARTESIAN_POINT('Ctrl Pts',(5.22737225841736,-3.05149415704693,10.8071760747641));
#5834=CARTESIAN_POINT('Ctrl Pts',(5.84331350686056,-1.57883160757971,10.4869526157176));
#5835=CARTESIAN_POINT('Ctrl Pts',(6.,-0.769830401762948,10.3923048454133));
#5836=CARTESIAN_POINT('Ctrl Pts',(6.,-8.32667268468867E-16,10.3923048454133));
#5837=CARTESIAN_POINT('',(-6.,-7.34788079488412E-16,0.));
#5838=CARTESIAN_POINT('Origin',(0.,20.,0.));
#5839=CARTESIAN_POINT('',(-15.,20.,-1.83697019872103E-15));
#5840=CARTESIAN_POINT('Origin',(0.,20.,0.));
#5841=CARTESIAN_POINT('',(-15.,26.,-1.83697019872103E-15));
#5842=CARTESIAN_POINT('',(-15.,20.,-1.83697019872103E-15));
#5843=CARTESIAN_POINT('Origin',(0.,26.,0.));
#5844=CARTESIAN_POINT('Origin',(0.,26.,0.));
#5845=CARTESIAN_POINT('',(-12.,26.,-1.46957615897682E-15));
#5846=CARTESIAN_POINT('Origin',(0.,26.,0.));
#5847=CARTESIAN_POINT('Origin',(0.,-20.,0.));
#5848=CARTESIAN_POINT('',(-15.,-26.,-1.83697019872103E-15));
#5849=CARTESIAN_POINT('Origin',(0.,-26.,0.));
#5850=CARTESIAN_POINT('',(-15.,-20.,-1.83697019872103E-15));
#5851=CARTESIAN_POINT('',(-15.,-20.,-1.83697019872103E-15));
#5852=CARTESIAN_POINT('Origin',(0.,-20.,0.));
#5853=CARTESIAN_POINT('Origin',(0.,-26.,0.));
#5854=CARTESIAN_POINT('',(-12.,-26.,-1.46957615897682E-15));
#5855=CARTESIAN_POINT('Origin',(0.,-26.,0.));
#5856=CARTESIAN_POINT('Origin',(0.,-20.,0.));
#5857=CARTESIAN_POINT('',(-12.,-20.,1.46957615897682E-15));
#5858=CARTESIAN_POINT('Origin',(0.,-20.,0.));
#5859=CARTESIAN_POINT('Origin',(0.,20.,0.));
#5860=CARTESIAN_POINT('',(0.,0.,0.));
#5861=CARTESIAN_POINT('Origin',(-9.5,-85.5138405476197,49.642135623731));
#5862=CARTESIAN_POINT('',(-11.,-31.1289553192861,49.642135623731));
#5863=CARTESIAN_POINT('',(-9.5,-31.1289553192861,48.142135623731));
#5864=CARTESIAN_POINT('Origin',(-9.5,-31.1289553192861,49.642135623731));
#5865=CARTESIAN_POINT('',(-9.5,-92.6421356237309,48.142135623731));
#5866=CARTESIAN_POINT('',(-9.5,-85.5138405476197,48.142135623731));
#5867=CARTESIAN_POINT('',(-11.,-92.6421356237309,49.642135623731));
#5868=CARTESIAN_POINT('Origin',(-9.5,-92.6421356237309,49.642135623731));
#5869=CARTESIAN_POINT('',(-11.,-85.5138405476197,49.642135623731));
#5870=CARTESIAN_POINT('Origin',(0.,-92.6421356237309,49.642135623731));
#5871=CARTESIAN_POINT('',(9.5,-92.6421356237309,48.142135623731));
#5872=CARTESIAN_POINT('',(11.,-92.6421356237309,49.642135623731));
#5873=CARTESIAN_POINT('Origin',(9.5,-92.6421356237309,49.642135623731));
#5874=CARTESIAN_POINT('Origin',(0.,-92.6421356237309,49.642135623731));
#5875=CARTESIAN_POINT('Origin',(0.,-92.6421356237309,48.142135623731));
#5876=CARTESIAN_POINT('Origin',(9.5,-85.5138405476197,49.642135623731));
#5877=CARTESIAN_POINT('',(9.5,-31.1289553192861,48.142135623731));
#5878=CARTESIAN_POINT('',(11.,-31.1289553192861,49.642135623731));
#5879=CARTESIAN_POINT('Origin',(9.5,-31.1289553192861,49.642135623731));
#5880=CARTESIAN_POINT('',(11.,-85.5138405476197,49.642135623731));
#5881=CARTESIAN_POINT('',(9.5,-85.5138405476197,48.142135623731));
#5882=CARTESIAN_POINT('Origin',(-11.,-67.3855454715085,50.642135623731));
#5883=CARTESIAN_POINT('',(-11.,-92.6421356237309,51.642135623731));
#5884=CARTESIAN_POINT('',(-11.,-92.6421356237309,51.892135623731));
#5885=CARTESIAN_POINT('',(-11.,-31.1289553192861,51.6421356237309));
#5886=CARTESIAN_POINT('',(-11.,-49.2572503953973,51.6421356237309));
#5887=CARTESIAN_POINT('',(-11.,-31.1289553192861,53.142135623731));
#5888=CARTESIAN_POINT('Origin',(0.,-92.6421356237309,51.892135623731));
#5889=CARTESIAN_POINT('',(11.,-92.6421356237309,51.642135623731));
#5890=CARTESIAN_POINT('',(11.,-92.6421356237309,51.892135623731));
#5891=CARTESIAN_POINT('Origin',(0.,-92.6421356237309,51.642135623731));
#5892=CARTESIAN_POINT('Origin',(11.,-67.3855454715085,50.642135623731));
#5893=CARTESIAN_POINT('',(11.,-31.1289553192861,51.642135623731));
#5894=CARTESIAN_POINT('',(11.,-31.1289553192861,53.142135623731));
#5895=CARTESIAN_POINT('',(11.,-49.2572503953973,51.642135623731));
#5896=CARTESIAN_POINT('Origin',(9.5,-49.2572503953973,51.642135623731));
#5897=CARTESIAN_POINT('',(9.5,-31.1289553192861,53.142135623731));
#5898=CARTESIAN_POINT('Origin',(9.5,-31.1289553192861,51.642135623731));
#5899=CARTESIAN_POINT('',(9.5,-92.6421356237309,53.142135623731));
#5900=CARTESIAN_POINT('',(9.5,-49.2572503953973,53.142135623731));
#5901=CARTESIAN_POINT('Origin',(9.5,-92.6421356237309,51.642135623731));
#5902=CARTESIAN_POINT('Origin',(0.,-92.6421356237309,51.642135623731));
#5903=CARTESIAN_POINT('',(-9.5,-92.6421356237309,53.142135623731));
#5904=CARTESIAN_POINT('Origin',(-9.5,-92.6421356237309,51.642135623731));
#5905=CARTESIAN_POINT('Origin',(0.,-92.6421356237309,53.142135623731));
#5906=CARTESIAN_POINT('Origin',(-9.5,-49.2572503953973,51.6421356237309));
#5907=CARTESIAN_POINT('',(-9.5,-31.1289553192861,53.142135623731));
#5908=CARTESIAN_POINT('Origin',(-9.5,-31.1289553192861,51.6421356237309));
#5909=CARTESIAN_POINT('',(-9.5,-49.2572503953973,53.142135623731));
#5910=CARTESIAN_POINT('Origin',(0.,-31.1289553192861,53.142135623731));
#5911=CARTESIAN_POINT('',(0.,-31.1289553192861,53.142135623731));
#5912=CARTESIAN_POINT('Origin',(0.,-31.1289553192861,52.142135623731));
#5913=CARTESIAN_POINT('',(0.,-31.1289553192861,48.142135623731));
#5914=CARTESIAN_POINT('',(-10.,-31.1289553192861,49.142135623731));
#5915=CARTESIAN_POINT('',(10.,-31.1289553192861,49.142135623731));
#5916=CARTESIAN_POINT('',(0.,-31.1289553192861,49.142135623731));
#5917=CARTESIAN_POINT('',(10.,-31.1289553192861,52.142135623731));
#5918=CARTESIAN_POINT('',(10.,-31.1289553192861,53.142135623731));
#5919=CARTESIAN_POINT('',(-10.,-31.1289553192861,52.142135623731));
#5920=CARTESIAN_POINT('',(0.,-31.1289553192861,52.142135623731));
#5921=CARTESIAN_POINT('',(-10.,-31.1289553192861,53.142135623731));
#5922=CARTESIAN_POINT('Origin',(20.,-80.281455848733,52.142135623731));
#5923=CARTESIAN_POINT('',(-10.,-80.281455848733,52.142135623731));
#5924=CARTESIAN_POINT('',(0.,-102.642135623731,52.142135623731));
#5925=CARTESIAN_POINT('Origin',(20.,-80.281455848733,52.142135623731));
#5926=CARTESIAN_POINT('',(0.,-102.642135623731,49.142135623731));
#5927=CARTESIAN_POINT('',(0.,-102.642135623731,52.142135623731));
#5928=CARTESIAN_POINT('',(-10.,-80.281455848733,49.142135623731));
#5929=CARTESIAN_POINT('Origin',(20.,-80.281455848733,49.142135623731));
#5930=CARTESIAN_POINT('',(-10.,-80.281455848733,52.142135623731));
#5931=CARTESIAN_POINT('Origin',(-10.,-67.3855454715085,50.642135623731));
#5932=CARTESIAN_POINT('',(-10.,-49.2572503953973,49.142135623731));
#5933=CARTESIAN_POINT('',(-10.,-85.0138405476197,52.142135623731));
#5934=CARTESIAN_POINT('Origin',(-20.,-80.281455848733,52.142135623731));
#5935=CARTESIAN_POINT('',(10.,-80.281455848733,52.142135623731));
#5936=CARTESIAN_POINT('Origin',(-20.,-80.281455848733,52.142135623731));
#5937=CARTESIAN_POINT('',(10.,-80.281455848733,49.142135623731));
#5938=CARTESIAN_POINT('',(10.,-80.281455848733,52.142135623731));
#5939=CARTESIAN_POINT('Origin',(-20.,-80.281455848733,49.142135623731));
#5940=CARTESIAN_POINT('Origin',(0.,-102.642135623731,52.142135623731));
#5941=CARTESIAN_POINT('',(10.,-85.0138405476197,52.142135623731));
#5942=CARTESIAN_POINT('Origin',(10.,-67.3855454715085,50.642135623731));
#5943=CARTESIAN_POINT('',(10.,-49.2572503953973,49.142135623731));
#5944=CARTESIAN_POINT('Origin',(0.,-31.1289553192861,49.142135623731));
#5945=CARTESIAN_POINT('Origin',(0.,-103.642135623731,48.142135623731));
#5946=CARTESIAN_POINT('',(0.,0.,0.));
#5947=CARTESIAN_POINT('Origin',(0.,4.0019382647053,9.1643052178268));
#5948=CARTESIAN_POINT('',(0.,4.0019382647053,9.1643052178268));
#5949=CARTESIAN_POINT('Origin',(0.,4.0019382647053,0.));
#5950=CARTESIAN_POINT('Origin',(0.,0.,0.));
#5951=CARTESIAN_POINT('',(0.,0.,0.));
#5952=CARTESIAN_POINT('Origin',(0.,13.3748739960349,0.));
#5953=CARTESIAN_POINT('',(1.59078448392775,20.0623165459775,12.0701224093086));
#5954=CARTESIAN_POINT('',(1.59078448392774,20.,12.0701224093086));
#5955=CARTESIAN_POINT('',(1.59078448392774,13.3748739960349,12.0701224093086));
#5956=CARTESIAN_POINT('',(3.14799128255578,20.,11.7604677260283));
#5957=CARTESIAN_POINT('Ctrl Pts',(3.14799128255578,20.,11.7604677260283));
#5958=CARTESIAN_POINT('Ctrl Pts',(2.8740867128099,20.0111238992557,11.8337853200134));
#5959=CARTESIAN_POINT('Ctrl Pts',(2.59757666171726,20.0222477985115,11.8975412512316));
#5960=CARTESIAN_POINT('Ctrl Pts',(2.31914702161461,20.0333716977672,11.9515692418249));
#5961=CARTESIAN_POINT('Ctrl Pts',(2.07765185627277,20.043019980504,11.9984302675283));
#5962=CARTESIAN_POINT('Ctrl Pts',(1.83471293240725,20.0526682632408,12.0379738048562));
#5963=CARTESIAN_POINT('Ctrl Pts',(1.59078448392775,20.0623165459775,12.0701224093086));
#5964=CARTESIAN_POINT('Origin',(0.,20.,0.));
#5965=CARTESIAN_POINT('Origin',(0.,13.3748739960349,0.));
#5966=CARTESIAN_POINT('',(1.59078448392772,23.0623012722853,12.0701224093087));
#5967=CARTESIAN_POINT('',(1.5908148051505,22.812547089465,12.070351758578));
#5968=CARTESIAN_POINT('',(1.59078448392774,13.3748739960349,12.0701224093086));
#5969=CARTESIAN_POINT('',(-12.1744999960254,20.8748739960726,-0.000311090449405607));
#5970=CARTESIAN_POINT('Ctrl Pts',(-12.1744999960254,20.8748739960726,-0.000311090449404772));
#5971=CARTESIAN_POINT('Ctrl Pts',(-12.1744923950652,20.8865393020214,-0.297774062673808));
#5972=CARTESIAN_POINT('Ctrl Pts',(-12.1635784601364,20.8982046079702,-0.595182841827181));
#5973=CARTESIAN_POINT('Ctrl Pts',(-12.1417960711354,20.909869913919,-0.891761412577232));
#5974=CARTESIAN_POINT('Ctrl Pts',(-12.1231530265705,20.9198539803433,-1.14559617382575));
#5975=CARTESIAN_POINT('Ctrl Pts',(-12.0965494250141,20.9298380467676,-1.39882274221339));
#5976=CARTESIAN_POINT('Ctrl Pts',(-12.0620392196327,20.939822113192,-1.65095733259334));
#5977=CARTESIAN_POINT('Ctrl Pts',(-12.0235090635879,20.9509691820964,-1.9324620354562));
#5978=CARTESIAN_POINT('Ctrl Pts',(-11.9751141751885,20.9621162510008,-2.2126594358091));
#5979=CARTESIAN_POINT('Ctrl Pts',(-11.9169675814257,20.9732633199052,-2.49085003829017));
#5980=CARTESIAN_POINT('Ctrl Pts',(-11.8588308783237,20.9844084927074,-2.76899332090735));
#5981=CARTESIAN_POINT('Ctrl Pts',(-11.7909458361135,20.9955536655097,-3.04513022613635));
#5982=CARTESIAN_POINT('Ctrl Pts',(-11.7134766039781,21.006698838312,-3.31857139414821));
#5983=CARTESIAN_POINT('Ctrl Pts',(-11.6360159868468,21.0178427717099,-3.591982154));
#5984=CARTESIAN_POINT('Ctrl Pts',(-11.5489733807489,21.0289867051078,-3.86269751864585));
#5985=CARTESIAN_POINT('Ctrl Pts',(-11.4525631648402,21.0401306385056,-4.1300420343315));
#5986=CARTESIAN_POINT('Ctrl Pts',(-11.3531130779724,21.0516259466949,-4.40581608024554));
#5987=CARTESIAN_POINT('Ctrl Pts',(-11.2436951564039,21.0631212548842,-4.67800297633621));
#5988=CARTESIAN_POINT('Ctrl Pts',(-11.1245994311076,21.0746165630735,-4.94588088689978));
#5989=CARTESIAN_POINT('Ctrl Pts',(-11.0091379329855,21.0857610898951,-5.20558445552521));
#5990=CARTESIAN_POINT('Ctrl Pts',(-10.8845806273897,21.0969056167168,-5.46123786352323));
#5991=CARTESIAN_POINT('Ctrl Pts',(-10.7512401330826,21.1080501435385,-5.71220499026376));
#5992=CARTESIAN_POINT('Ctrl Pts',(-10.6116041681331,21.1197208424116,-5.97502115196405));
#5993=CARTESIAN_POINT('Ctrl Pts',(-10.4623358132792,21.1313915412847,-6.23269757967499));
#5994=CARTESIAN_POINT('Ctrl Pts',(-10.3038478790065,21.1430622401578,-6.48453307002857));
#5995=CARTESIAN_POINT('Ctrl Pts',(-10.1453599447337,21.1547329390309,-6.73636856038215));
#5996=CARTESIAN_POINT('Ctrl Pts',(-9.97765261724218,21.166403637904,-6.98236283400452));
#5997=CARTESIAN_POINT('Ctrl Pts',(-9.80119115426147,21.1780743367771,-7.22184894660825));
#5998=CARTESIAN_POINT('Ctrl Pts',(-9.63264179299859,21.1892217499704,-7.45059708588386));
#5999=CARTESIAN_POINT('Ctrl Pts',(-9.45605571647231,21.2003691631638,-7.67347617436341));
#6000=CARTESIAN_POINT('Ctrl Pts',(-9.27186695090699,21.2115165763572,-7.88992607662954));
#6001=CARTESIAN_POINT('Ctrl Pts',(-9.08770945043724,21.2226620973345,-8.10633923763807));
#6002=CARTESIAN_POINT('Ctrl Pts',(-8.89595201024563,21.2338076183118,-8.31632518819218));
#6003=CARTESIAN_POINT('Ctrl Pts',(-8.69706869375794,21.2449531392891,-8.51935715802874));
#6004=CARTESIAN_POINT('Ctrl Pts',(-8.49820744079386,21.2560974238155,-8.72236660410243));
#6005=CARTESIAN_POINT('Ctrl Pts',(-8.29222207669095,21.2672417083419,-8.91842341943104));
#6006=CARTESIAN_POINT('Ctrl Pts',(-8.07962411441024,21.2783859928682,-9.10703708237979));
#6007=CARTESIAN_POINT('Ctrl Pts',(-7.86033469976557,21.2898810401594,-9.30158729959874));
#6008=CARTESIAN_POINT('Ctrl Pts',(-7.63400990204134,21.3013760874505,-9.48821803027954));
#6009=CARTESIAN_POINT('Ctrl Pts',(-7.40124976128749,21.3128711347417,-9.66643430749115));
#6010=CARTESIAN_POINT('Ctrl Pts',(-7.17558004674712,21.3240160156153,-9.83922169400216));
#6011=CARTESIAN_POINT('Ctrl Pts',(-6.94386147980823,21.3351608964889,-10.0040995187547));
#6012=CARTESIAN_POINT('Ctrl Pts',(-6.70667300845964,21.3463057773625,-10.1606588077545));
#6013=CARTESIAN_POINT('Ctrl Pts',(-6.45830602768054,21.3579759078624,-10.3245966151054));
#6014=CARTESIAN_POINT('Ctrl Pts',(-6.20394142385836,21.3696460383624,-10.4794127629059));
#6015=CARTESIAN_POINT('Ctrl Pts',(-5.94427710028753,21.3813161688623,-10.6246891721592));
#6016=CARTESIAN_POINT('Ctrl Pts',(-5.68461277671671,21.3929862993622,-10.7699655814125));
#6017=CARTESIAN_POINT('Ctrl Pts',(-5.41964903042489,21.4046564298622,-10.9057020959921));
#6018=CARTESIAN_POINT('Ctrl Pts',(-5.15011341352574,21.4163265603621,-11.031535798692));
#6019=CARTESIAN_POINT('Ctrl Pts',(-4.89265384818702,21.4274738319566,-11.1517317519199));
#6020=CARTESIAN_POINT('Ctrl Pts',(-4.63094619394671,21.4386211035511,-11.262928642111));
#6021=CARTESIAN_POINT('Ctrl Pts',(-4.36563958289154,21.4497683751456,-11.3648423342469));
#6022=CARTESIAN_POINT('Ctrl Pts',(-4.10037804211338,21.460913753042,-11.4667387132886));
#6023=CARTESIAN_POINT('Ctrl Pts',(-3.83151901407759,21.4720591309384,-11.5593549471958));
#6024=CARTESIAN_POINT('Ctrl Pts',(-3.55973082007956,21.4832045088348,-11.6424553569501));
#6025=CARTESIAN_POINT('Ctrl Pts',(-3.28797280464175,21.4943486491813,-11.7255465394797));
#6026=CARTESIAN_POINT('Ctrl Pts',(-3.01328652773389,21.5054927895278,-11.7991239297607));
#6027=CARTESIAN_POINT('Ctrl Pts',(-2.73635584774457,21.5166369298742,-11.8630015984368));
#6028=CARTESIAN_POINT('Ctrl Pts',(-2.45070250392632,21.5281320843803,-11.9288912631476));
#6029=CARTESIAN_POINT('Ctrl Pts',(-2.16266136567062,21.5396272388864,-11.9844601901464));
#6030=CARTESIAN_POINT('Ctrl Pts',(-1.87299620102137,21.5511223933925,-12.0295609014195));
#6031=CARTESIAN_POINT('Ctrl Pts',(-1.59216120034856,21.5622671291682,-12.0732867608822));
#6032=CARTESIAN_POINT('Ctrl Pts',(-1.30979999634929,21.573411864944,-12.1071731361329));
#6033=CARTESIAN_POINT('Ctrl Pts',(-1.02661663648201,21.5845566007197,-12.1311379734837));
#6034=CARTESIAN_POINT('Ctrl Pts',(-0.730077273105364,21.596226964591,-12.156233083644));
#6035=CARTESIAN_POINT('Ctrl Pts',(-0.432636652240616,21.6078973284622,-12.1704482314372));
#6036=CARTESIAN_POINT('Ctrl Pts',(-0.135107706832327,21.6195676923335,-12.1737502914079));
#6037=CARTESIAN_POINT('Ctrl Pts',(0.162421238575963,21.6312380562048,-12.1770523513786));
#6038=CARTESIAN_POINT('Ctrl Pts',(0.460038172932362,21.642908420076,-12.1694413285824));
#6039=CARTESIAN_POINT('Ctrl Pts',(0.756930527455535,21.6545787839473,-12.1509467296423));
#6040=CARTESIAN_POINT('Ctrl Pts',(1.04051646831786,21.665726093968,-12.1332810398346));
#6041=CARTESIAN_POINT('Ctrl Pts',(1.3235260540737,21.6768734039887,-12.1056806331005));
#6042=CARTESIAN_POINT('Ctrl Pts',(1.60525332965216,21.6880207140093,-12.06820666038));
#6043=CARTESIAN_POINT('Ctrl Pts',(1.88693275396258,21.6991661306637,-12.0307390525992));
#6044=CARTESIAN_POINT('Ctrl Pts',(2.16733003861535,21.7103115473181,-11.983401262163));
#6045=CARTESIAN_POINT('Ctrl Pts',(2.44574556760614,21.7214569639726,-11.9263061703335));
#6046=CARTESIAN_POINT('Ctrl Pts',(2.72413018796549,21.7326011433053,-11.8692174169836));
#6047=CARTESIAN_POINT('Ctrl Pts',(3.00053323073995,21.743745322638,-11.8023735788287));
#6048=CARTESIAN_POINT('Ctrl Pts',(3.27426524481732,21.7548895019707,-11.7259386556719));
#6049=CARTESIAN_POINT('Ctrl Pts',(3.55661747114543,21.7663846274342,-11.6470966875694));
#6050=CARTESIAN_POINT('Ctrl Pts',(3.83612742536485,21.7778797528976,-11.5580498424948));
#6051=CARTESIAN_POINT('Ctrl Pts',(4.11205390419272,21.7893748783611,-11.4590341189392));
#6052=CARTESIAN_POINT('Ctrl Pts',(4.37957064322381,21.8005196532004,-11.3630362154727));
#6053=CARTESIAN_POINT('Ctrl Pts',(4.64371884535662,21.8116644280397,-11.2576681964017));
#6054=CARTESIAN_POINT('Ctrl Pts',(4.90384104113907,21.8228092028791,-11.1431949320309));
#6055=CARTESIAN_POINT('Ctrl Pts',(5.1762291608586,21.8344795036546,-11.0233237416994));
#6056=CARTESIAN_POINT('Ctrl Pts',(5.44420215910206,21.8461498044302,-10.8934680664645));
#6057=CARTESIAN_POINT('Ctrl Pts',(5.70703039091337,21.8578201052057,-10.7539878355516));
#6058=CARTESIAN_POINT('Ctrl Pts',(5.96985862272468,21.8694904059813,-10.6145076046387));
#6059=CARTESIAN_POINT('Ctrl Pts',(6.22754179586538,21.8811607067569,-10.465402983073));
#6060=CARTESIAN_POINT('Ctrl Pts',(6.47938055605088,21.8928310075324,-10.3070887189288));
#6061=CARTESIAN_POINT('Ctrl Pts',(6.71993349237776,21.9039783190793,-10.1558691009707));
#6062=CARTESIAN_POINT('Ctrl Pts',(6.95522616261537,21.9151256306262,-9.9962019716106));
#6063=CARTESIAN_POINT('Ctrl Pts',(7.18466795616308,21.9262729421732,-9.82847885533074));
#6064=CARTESIAN_POINT('Ctrl Pts',(7.41407078071216,21.9374183604313,-9.66078422558678));
#6065=CARTESIAN_POINT('Ctrl Pts',(7.6376244972866,21.9485637786895,-9.48503649799234));
#6066=CARTESIAN_POINT('Ctrl Pts',(7.85476881658421,21.9597091969477,-9.30166958604832));
#6067=CARTESIAN_POINT('Ctrl Pts',(8.07188903077369,21.9708533779572,-9.11832302959531));
#6068=CARTESIAN_POINT('Ctrl Pts',(8.28260106469835,21.9819975589667,-8.92735914978249));
#6069=CARTESIAN_POINT('Ctrl Pts',(8.48637801690925,21.9931417399762,-8.72925188112472));
#6070=CARTESIAN_POINT('Ctrl Pts',(8.69657214291512,22.004636864238,-8.52490598361697));
#6071=CARTESIAN_POINT('Ctrl Pts',(8.89938710238414,22.0161319884998,-8.31295969955983));
#6072=CARTESIAN_POINT('Ctrl Pts',(9.09428500702047,22.0276271127616,-8.09397494813783));
#6073=CARTESIAN_POINT('Ctrl Pts',(9.28324282708307,22.0387718894379,-7.88166439850486));
#6074=CARTESIAN_POINT('Ctrl Pts',(9.46475885166343,22.0499166661142,-7.66273827282285));
#6075=CARTESIAN_POINT('Ctrl Pts',(9.63838253212706,22.0610614427905,-7.43774377176224));
#6076=CARTESIAN_POINT('Ctrl Pts',(9.82019327263628,22.072731740845,-7.20213986831372));
#6077=CARTESIAN_POINT('Ctrl Pts',(9.99334925383761,22.0844020388995,-6.95988177403458));
#6078=CARTESIAN_POINT('Ctrl Pts',(10.1573820426963,22.096072336954,-6.71163469571394));
#6079=CARTESIAN_POINT('Ctrl Pts',(10.3214148315549,22.1077426350085,-6.4633876173933));
#6080=CARTESIAN_POINT('Ctrl Pts',(10.4763242504391,22.119412933063,-6.20915183978187));
#6081=CARTESIAN_POINT('Ctrl Pts',(10.6216946965625,22.1310832311175,-5.94962620868038));
#6082=CARTESIAN_POINT('Ctrl Pts',(10.7605504536662,22.142230531791,-5.70173106248379));
#6083=CARTESIAN_POINT('Ctrl Pts',(10.8907448834759,22.1533778324646,-5.44893572672565));
#6084=CARTESIAN_POINT('Ctrl Pts',(11.0119467530863,22.1645251331381,-5.19186661589001));
#6085=CARTESIAN_POINT('Ctrl Pts',(11.133128035799,22.1756705403727,-4.934841169855));
#6086=CARTESIAN_POINT('Ctrl Pts',(11.2453196941389,22.1868159476073,-4.67354363924085));
#6087=CARTESIAN_POINT('Ctrl Pts',(11.3482374041766,22.197961354842,-4.4086231488355));
#6088=CARTESIAN_POINT('Ctrl Pts',(11.4511436882337,22.2091055247073,-4.14373207004823));
#6089=CARTESIAN_POINT('Ctrl Pts',(11.5447779833639,22.2202496945727,-3.87521908322539));
#6090=CARTESIAN_POINT('Ctrl Pts',(11.6289044340636,22.2313938644381,-3.6037524767131));
#6091=CARTESIAN_POINT('Ctrl Pts',(11.7156802739048,22.2428889969602,-3.3237365890463));
#6092=CARTESIAN_POINT('Ctrl Pts',(11.7923396078497,22.2543841294822,-3.04057831121402));
#6093=CARTESIAN_POINT('Ctrl Pts',(11.8586790366335,22.2658792620042,-2.75502844923766));
#6094=CARTESIAN_POINT('Ctrl Pts',(11.9229964655406,22.2770240273771,-2.47818203551679));
#6095=CARTESIAN_POINT('Ctrl Pts',(11.9776137036275,22.2881687927499,-2.19908793968402));
#6096=CARTESIAN_POINT('Ctrl Pts',(12.0223969991252,22.2993135581228,-1.91844224448522));
#6097=CARTESIAN_POINT('Ctrl Pts',(12.0692921285266,22.3109838742194,-1.62456221520135));
#6098=CARTESIAN_POINT('Ctrl Pts',(12.1054034747324,22.322654190316,-1.32898104250092));
#6099=CARTESIAN_POINT('Ctrl Pts',(12.1306380526509,22.3343245064127,-1.03250699057074));
#6100=CARTESIAN_POINT('Ctrl Pts',(12.1558726305694,22.3459948225093,-0.736032938640579));
#6101=CARTESIAN_POINT('Ctrl Pts',(12.1702304204935,22.3576651386059,-0.43866634252017));
#6102=CARTESIAN_POINT('Ctrl Pts',(12.1736809240298,22.3693354547026,-0.14121972211462));
#6103=CARTESIAN_POINT('Ctrl Pts',(12.1769767929329,22.3804827645107,0.142896800657586));
#6104=CARTESIAN_POINT('Ctrl Pts',(12.1703224929076,22.3916300743188,0.427171187125004));
#6105=CARTESIAN_POINT('Ctrl Pts',(12.1537269468445,22.4027773841269,0.710894894865639));
#6106=CARTESIAN_POINT('Ctrl Pts',(12.1371342194696,22.4139228006082,0.99457041324932));
#6107=CARTESIAN_POINT('Ctrl Pts',(12.11060363268,22.4250682170895,1.2776951734493));
#6108=CARTESIAN_POINT('Ctrl Pts',(12.074196166311,22.4362136335708,1.55956313993394));
#6109=CARTESIAN_POINT('Ctrl Pts',(12.0377927416301,22.4473578127703,1.84139981551791));
#6110=CARTESIAN_POINT('Ctrl Pts',(11.9915146609846,22.4585019919697,2.12197971150438));
#6111=CARTESIAN_POINT('Ctrl Pts',(11.9354746331794,22.4696461711692,2.40060315977681));
#6112=CARTESIAN_POINT('Ctrl Pts',(11.8776698234813,22.4811412967624,2.68800086523175));
#6113=CARTESIAN_POINT('Ctrl Pts',(11.8094783169454,22.4926364223556,2.97331661069409));
#6114=CARTESIAN_POINT('Ctrl Pts',(11.7310808084977,22.5041315479488,3.25579380712257));
#6115=CARTESIAN_POINT('Ctrl Pts',(11.6550727153316,22.5152763227554,3.52966160583902));
#6116=CARTESIAN_POINT('Ctrl Pts',(11.5694716039288,22.5264210975619,3.80086105222759));
#6117=CARTESIAN_POINT('Ctrl Pts',(11.474493137458,22.5375658723685,4.06871693392769));
#6118=CARTESIAN_POINT('Ctrl Pts',(11.3750360097731,22.549236173355,4.34920342331078));
#6119=CARTESIAN_POINT('Ctrl Pts',(11.2652959853262,22.5609064743416,4.62602313302054));
#6120=CARTESIAN_POINT('Ctrl Pts',(11.1455782047075,22.5725767753281,4.89842186145174));
#6121=CARTESIAN_POINT('Ctrl Pts',(11.0258604240889,22.5842470763146,5.17082058988296));
#6122=CARTESIAN_POINT('Ctrl Pts',(10.8961650303231,22.5959173773012,5.43879803342295));
#6123=CARTESIAN_POINT('Ctrl Pts',(10.7568540674013,22.6075876782877,5.7016261559867));
#6124=CARTESIAN_POINT('Ctrl Pts',(10.6237862289835,22.6187349828027,5.95267581791911));
#6125=CARTESIAN_POINT('Ctrl Pts',(10.4819059659421,22.6298822873177,6.19910251958811));
#6126=CARTESIAN_POINT('Ctrl Pts',(10.331560180348,22.6410295918327,6.44028838561183));
#6127=CARTESIAN_POINT('Ctrl Pts',(10.1812399312278,22.65217500296,6.68143328582792));
#6128=CARTESIAN_POINT('Ctrl Pts',(10.0224571713425,22.6633204140874,6.91733890132951));
#6129=CARTESIAN_POINT('Ctrl Pts',(9.85560331246676,22.6744658252148,7.14741446939341));
#6130=CARTESIAN_POINT('Ctrl Pts',(9.68876797717991,22.6856099990138,7.37746449519373));
#6131=CARTESIAN_POINT('Ctrl Pts',(9.51386348869,22.6967541728128,7.60168555009451));
#6132=CARTESIAN_POINT('Ctrl Pts',(9.33132363306449,22.7078983466118,7.81951721687548));
#6133=CARTESIAN_POINT('Ctrl Pts',(9.14303517522486,22.7193934762168,8.04420890662334));
#6134=CARTESIAN_POINT('Ctrl Pts',(8.9466228297042,22.7308886058219,8.26210202013036));
#6135=CARTESIAN_POINT('Ctrl Pts',(8.74260731912758,22.742383735427,8.47261869279722));
#6136=CARTESIAN_POINT('Ctrl Pts',(8.54481000069478,22.7535285047855,8.67671902429267));
#6137=CARTESIAN_POINT('Ctrl Pts',(8.33986632224162,22.7646732741439,8.87388570935947));
#6138=CARTESIAN_POINT('Ctrl Pts',(8.12828876731127,22.7758180435024,9.0636290725736));
#6139=CARTESIAN_POINT('Ctrl Pts',(7.90673410626821,22.7874883532308,9.26231993340673));
#6140=CARTESIAN_POINT('Ctrl Pts',(7.67790509962432,22.7991586629592,9.45287030906345));
#6141=CARTESIAN_POINT('Ctrl Pts',(7.44243059986118,22.8108289726876,9.63476398342222));
#6142=CARTESIAN_POINT('Ctrl Pts',(7.20695610009804,22.822499282416,9.81665765778099));
#6143=CARTESIAN_POINT('Ctrl Pts',(6.96483637809425,22.8341695921444,9.98989443269214));
#6144=CARTESIAN_POINT('Ctrl Pts',(6.71673773003182,22.8458399018728,10.1540082980056));
#6145=CARTESIAN_POINT('Ctrl Pts',(6.47975894975053,22.8569871442562,10.3107665227399));
#6146=CARTESIAN_POINT('Ctrl Pts',(6.23725464023926,22.8681343866396,10.4592484615104));
#6147=CARTESIAN_POINT('Ctrl Pts',(5.98982507339607,22.879281629023,10.5990775938341));
#6148=CARTESIAN_POINT('Ctrl Pts',(5.74243799903203,22.8904269570274,10.7388827125099));
#6149=CARTESIAN_POINT('Ctrl Pts',(5.49012758823057,22.9015722850318,10.8700378604094));
#6150=CARTESIAN_POINT('Ctrl Pts',(5.2335202165415,22.9127176130361,10.9922116242843));
#6151=CARTESIAN_POINT('Ctrl Pts',(4.97694181572515,22.9238616827373,11.1143715947887));
#6152=CARTESIAN_POINT('Ctrl Pts',(4.71606766354038,22.9350057524385,11.2275520914857));
#6153=CARTESIAN_POINT('Ctrl Pts',(4.4515468169242,22.9461498221397,11.3314686244428));
#6154=CARTESIAN_POINT('Ctrl Pts',(4.18701646107352,22.957294292458,11.4353888930854));
#6155=CARTESIAN_POINT('Ctrl Pts',(3.91883939619725,22.9684387627762,11.5300444326363));
#6156=CARTESIAN_POINT('Ctrl Pts',(3.64768399310814,22.9795832330945,11.6151991690381));
#6157=CARTESIAN_POINT('Ctrl Pts',(3.3765343878357,22.9907274651229,11.7003520846701));
#6158=CARTESIAN_POINT('Ctrl Pts',(3.10240682663631,23.0018716971513,11.7760045248472));
#6159=CARTESIAN_POINT('Ctrl Pts',(2.82598510932383,23.0130159291796,11.8419702081993));
#6160=CARTESIAN_POINT('Ctrl Pts',(2.54952132601668,23.0241618571428,11.9079459302419));
#6161=CARTESIAN_POINT('Ctrl Pts',(2.27076294842339,23.0353077851059,11.9642318876258));
#6162=CARTESIAN_POINT('Ctrl Pts',(1.99040570099081,23.0464537130691,12.0106925443733));
#6163=CARTESIAN_POINT('Ctrl Pts',(1.85753271828706,23.0517362328078,12.0327121857307));
#6164=CARTESIAN_POINT('Ctrl Pts',(1.72430074052143,23.0570187525466,12.0525256043933));
#6165=CARTESIAN_POINT('Ctrl Pts',(1.59078448392772,23.0623012722853,12.0701224093086));
#6166=CARTESIAN_POINT('Ctrl Pts',(1.59078448392775,20.0623165459775,12.0701224093086));
#6167=CARTESIAN_POINT('Ctrl Pts',(1.30962621197678,20.073437407519,12.1071777266766));
#6168=CARTESIAN_POINT('Ctrl Pts',(1.02715337834117,20.0845582690605,12.134407435356));
#6169=CARTESIAN_POINT('Ctrl Pts',(0.744068298005909,20.0956791306019,12.1517411352408));
#6170=CARTESIAN_POINT('Ctrl Pts',(0.460962936440192,20.1068007888818,12.169076076974));
#6171=CARTESIAN_POINT('Ctrl Pts',(0.177245508869123,20.1179224471617,12.1765135734054));
#6172=CARTESIAN_POINT('Ctrl Pts',(-0.106378153026004,20.1290441054415,12.1740352364596));
#6173=CARTESIAN_POINT('Ctrl Pts',(-0.389997569760771,20.1401655972571,12.1715569366084));
#6174=CARTESIAN_POINT('Ctrl Pts',(-0.673522954588797,20.1512870890726,12.1591631043686));
#6175=CARTESIAN_POINT('Ctrl Pts',(-0.956249174934971,20.1624085808882,12.1368874826059));
#6176=CARTESIAN_POINT('Ctrl Pts',(-1.23904168428342,20.1735326802885,12.1146066380212));
#6177=CARTESIAN_POINT('Ctrl Pts',(-1.52103438623292,20.1846567796889,12.0824393934102));
#6178=CARTESIAN_POINT('Ctrl Pts',(-1.80152635112408,20.1957808790892,12.040471463203));
#6179=CARTESIAN_POINT('Ctrl Pts',(-2.0476611742289,20.205542400205,12.0036441370383));
#6180=CARTESIAN_POINT('Ctrl Pts',(-2.29264034845842,20.2153039213208,11.9592708188833));
#6181=CARTESIAN_POINT('Ctrl Pts',(-2.53599567615223,20.2250654424367,11.90744205027));
#6182=CARTESIAN_POINT('Ctrl Pts',(-2.81389961659165,20.2362127849193,11.8482552670495));
#6183=CARTESIAN_POINT('Ctrl Pts',(-3.08977208840519,20.2473601274019,11.7793265425913));
#6184=CARTESIAN_POINT('Ctrl Pts',(-3.36292380790852,20.2585074698845,11.7008202153611));
#6185=CARTESIAN_POINT('Ctrl Pts',(-3.63602920899081,20.2696529221088,11.6223272004729));
#6186=CARTESIAN_POINT('Ctrl Pts',(-3.9064145225981,20.2807983743331,11.5342598989375));
#6187=CARTESIAN_POINT('Ctrl Pts',(-4.17340434525476,20.2919438265575,11.4368328841952));
#6188=CARTESIAN_POINT('Ctrl Pts',(-4.44036459984117,20.3030880444669,11.3394166591106));
#6189=CARTESIAN_POINT('Ctrl Pts',(-4.70392986384737,20.3142322623763,11.2326428820652));
#6190=CARTESIAN_POINT('Ctrl Pts',(-4.96344230817149,20.3253764802858,11.1167751935286));
#6191=CARTESIAN_POINT('Ctrl Pts',(-5.23112562292012,20.3368715790971,10.9972593567428));
#6192=CARTESIAN_POINT('Ctrl Pts',(-5.49449649858255,20.3483666779084,10.8680677908843));
#6193=CARTESIAN_POINT('Ctrl Pts',(-5.75285652074247,20.3598617767198,10.729542958661));
#6194=CARTESIAN_POINT('Ctrl Pts',(-6.00334380137742,20.3710065971057,10.5952392524066));
#6195=CARTESIAN_POINT('Ctrl Pts',(-6.24912084279441,20.3821514174917,10.4521627969435));
#6196=CARTESIAN_POINT('Ctrl Pts',(-6.48957628823942,20.3932962378776,10.3006723008317));
#6197=CARTESIAN_POINT('Ctrl Pts',(-6.74136789952962,20.4049664759016,10.1420398521444));
#6198=CARTESIAN_POINT('Ctrl Pts',(-6.98732380660484,20.4166367139257,9.97418109459459));
#6199=CARTESIAN_POINT('Ctrl Pts',(-7.22677526496643,20.4283069519497,9.79755936545778));
#6200=CARTESIAN_POINT('Ctrl Pts',(-7.46622672332803,20.4399771899737,9.62093763632096));
#6201=CARTESIAN_POINT('Ctrl Pts',(-7.69917346821445,20.4516474279977,9.43555314181044));
#6202=CARTESIAN_POINT('Ctrl Pts',(-7.9249847794445,20.4633176660218,9.24191898339155));
#6203=CARTESIAN_POINT('Ctrl Pts',(-8.14066853729478,20.474464498208,9.05696924500836));
#6204=CARTESIAN_POINT('Ctrl Pts',(-8.34990739550198,20.4856113303942,8.86443818228698));
#6205=CARTESIAN_POINT('Ctrl Pts',(-8.55217478046388,20.4967581625804,8.66479986926402));
#6206=CARTESIAN_POINT('Ctrl Pts',(-8.75440768931906,20.5079030948094,8.46519558422725));
#6207=CARTESIAN_POINT('Ctrl Pts',(-8.9496713075049,20.5190480270384,8.25848665482182));
#6208=CARTESIAN_POINT('Ctrl Pts',(-9.13747528589881,20.5301929592674,8.04518462495352));
#6209=CARTESIAN_POINT('Ctrl Pts',(-9.3252583249383,20.5413366488833,7.83190637736524));
#6210=CARTESIAN_POINT('Ctrl Pts',(-9.5055832087329,20.5524803384992,7.61203669738287));
#6211=CARTESIAN_POINT('Ctrl Pts',(-9.67799849801041,20.5636240281151,7.38612180528512));
#6212=CARTESIAN_POINT('Ctrl Pts',(-9.85585682286771,20.5751195165727,7.15307493086235));
#6213=CARTESIAN_POINT('Ctrl Pts',(-10.0252978522716,20.5866150050304,6.91359518794776));
#6214=CARTESIAN_POINT('Ctrl Pts',(-10.1858721211816,20.598110493488,6.66831758248921));
#6215=CARTESIAN_POINT('Ctrl Pts',(-10.3415405228375,20.6092547716255,6.43053370177853));
#6216=CARTESIAN_POINT('Ctrl Pts',(-10.4888757631469,20.620399049763,6.18730120579808));
#6217=CARTESIAN_POINT('Ctrl Pts',(-10.6275127035771,20.6315433279005,5.93922755796635));
#6218=CARTESIAN_POINT('Ctrl Pts',(-10.7727033288179,20.6432144215182,5.67942690221995));
#6219=CARTESIAN_POINT('Ctrl Pts',(-10.9083532859157,20.654885515136,5.41431662760413));
#6220=CARTESIAN_POINT('Ctrl Pts',(-11.0340969861489,20.6665566087537,5.14462379093558));
#6221=CARTESIAN_POINT('Ctrl Pts',(-11.159840686382,20.6782277023714,4.87493095426703));
#6222=CARTESIAN_POINT('Ctrl Pts',(-11.2756779958382,20.6898987959892,4.60065586355721));
#6223=CARTESIAN_POINT('Ctrl Pts',(-11.3813005554201,20.7015698896069,4.32255108902081));
#6224=CARTESIAN_POINT('Ctrl Pts',(-11.4819409370545,20.7126904619584,4.05756441614999));
#6225=CARTESIAN_POINT('Ctrl Pts',(-11.5733394354702,20.7238110343099,3.7890178396337));
#6226=CARTESIAN_POINT('Ctrl Pts',(-11.6552609185346,20.7349316066614,3.51757632054809));
#6227=CARTESIAN_POINT('Ctrl Pts',(-11.7411699266226,20.7465934724425,3.23292239600646));
#6228=CARTESIAN_POINT('Ctrl Pts',(-11.8166563253145,20.7582553382236,2.94508500430039));
#6229=CARTESIAN_POINT('Ctrl Pts',(-11.8815075908379,20.7699172040048,2.65484982981369));
#6230=CARTESIAN_POINT('Ctrl Pts',(-11.9433326930578,20.7810348905784,2.37815793821194));
#6231=CARTESIAN_POINT('Ctrl Pts',(-11.995492397791,20.792152577152,2.09928720024168));
#6232=CARTESIAN_POINT('Ctrl Pts',(-12.0378545291329,20.8032702637256,1.81893061589332));
#6233=CARTESIAN_POINT('Ctrl Pts',(-12.0802138904517,20.8143872233234,1.53859236381978));
#6234=CARTESIAN_POINT('Ctrl Pts',(-12.1127769187808,20.8255041829211,1.25676872584638));
#6235=CARTESIAN_POINT('Ctrl Pts',(-12.1354629727721,20.8366211425188,0.974160503447343));
#6236=CARTESIAN_POINT('Ctrl Pts',(-12.1581504142312,20.8477387820242,0.691534996870884));
#6237=CARTESIAN_POINT('Ctrl Pts',(-12.1709596530285,20.8588564215296,0.408125078448854));
#6238=CARTESIAN_POINT('Ctrl Pts',(-12.1738620090751,20.869974061035,0.124635604858819));
#6239=CARTESIAN_POINT('Ctrl Pts',(-12.1742883992265,20.8716073727016,0.0829876755153614));
#6240=CARTESIAN_POINT('Ctrl Pts',(-12.1745010602666,20.8732406843683,0.0413380318515849));
#6241=CARTESIAN_POINT('Ctrl Pts',(-12.1744999960254,20.8748739960349,-0.000311089488517879));
#6242=CARTESIAN_POINT('',(-3.14788895504393,20.,11.7604951161383));
#6243=CARTESIAN_POINT('Origin',(0.,20.,0.));
#6244=CARTESIAN_POINT('',(-12.1737246773372,20.6251260039651,-0.000249401258526419));
#6245=CARTESIAN_POINT('Ctrl Pts',(-3.14788895504386,20.,11.7604951161383));
#6246=CARTESIAN_POINT('Ctrl Pts',(-5.10402892604601,20.0794174078617,11.2369022445433));
#6247=CARTESIAN_POINT('Ctrl Pts',(-8.7479903792511,20.2382522235851,9.19518133472436));
#6248=CARTESIAN_POINT('Ctrl Pts',(-11.6635919119852,20.4466275582401,4.5523794220281));
#6249=CARTESIAN_POINT('Ctrl Pts',(-12.1729512588234,20.5755854850334,1.26311059284835));
#6250=CARTESIAN_POINT('Ctrl Pts',(-12.1737246773372,20.6251260039651,-0.000249401258526419));
#6251=CARTESIAN_POINT('Ctrl Pts',(-12.1737246773372,20.6251260039651,-0.000249401258526419));
#6252=CARTESIAN_POINT('Ctrl Pts',(-12.1741911104616,20.6550028928951,-0.762156362199578));
#6253=CARTESIAN_POINT('Ctrl Pts',(-11.9165818304369,20.7642971896869,-3.54900219940989));
#6254=CARTESIAN_POINT('Ctrl Pts',(-9.8146932898574,20.9530088943404,-8.04643346012397));
#6255=CARTESIAN_POINT('Ctrl Pts',(-4.76736202235426,21.1912611179255,-11.7619196070543));
#6256=CARTESIAN_POINT('Ctrl Pts',(1.44252672235886,21.4295133415106,-12.6091655852676));
#6257=CARTESIAN_POINT('Ctrl Pts',(7.30065724870191,21.6677655650957,-10.3813184923891));
#6258=CARTESIAN_POINT('Ctrl Pts',(11.3783496330833,21.9060177886808,-5.62180304001539));
#6259=CARTESIAN_POINT('Ctrl Pts',(12.6811956770552,22.1442700122659,0.50872888397338));
#6260=CARTESIAN_POINT('Ctrl Pts',(10.8914562364704,22.382522235851,6.51518676137968));
#6261=CARTESIAN_POINT('Ctrl Pts',(6.73471108682879,22.605281261584,10.6455116559698));
#6262=CARTESIAN_POINT('Ctrl Pts',(3.2064497298399,22.7486228794554,11.8556871280485));
#6263=CARTESIAN_POINT('Ctrl Pts',(1.5908148051505,22.812547089465,12.070351758578));
#6264=CARTESIAN_POINT('Origin',(0.,13.3748739960349,0.));
#6265=CARTESIAN_POINT('',(1.59078448392775,26.0623070005467,12.0701224093086));
#6266=CARTESIAN_POINT('',(1.59078448392773,25.8125631998879,12.0701224093087));
#6267=CARTESIAN_POINT('',(1.59078448392774,13.3748739960349,12.0701224093086));
#6268=CARTESIAN_POINT('',(-12.1744999967658,23.8748739960011,0.000280623926547941));
#6269=CARTESIAN_POINT('Ctrl Pts',(-12.1744999967658,23.8748739960349,0.00028062306491734));
#6270=CARTESIAN_POINT('Ctrl Pts',(-12.1745065428157,23.8860100974646,-0.283712015376132));
#6271=CARTESIAN_POINT('Ctrl Pts',(-12.1645717688562,23.8971461988943,-0.567720156626778));
#6272=CARTESIAN_POINT('Ctrl Pts',(-12.1447184939399,23.908282300324,-0.8510363993127));
#6273=CARTESIAN_POINT('Ctrl Pts',(-12.1248634023349,23.9194194207708,-1.13437856706043));
#6274=CARTESIAN_POINT('Ctrl Pts',(-12.0950880117066,23.9305565412177,-1.41702844262597));
#6275=CARTESIAN_POINT('Ctrl Pts',(-12.0554671639295,23.9416936616646,-1.6982819876032));
#6276=CARTESIAN_POINT('Ctrl Pts',(-12.0158465226463,23.9528307240675,-1.97953406675724));
#6277=CARTESIAN_POINT('Ctrl Pts',(-11.9663805663668,23.9639677864705,-2.25938956526504));
#6278=CARTESIAN_POINT('Ctrl Pts',(-11.9071957223858,23.9751048488735,-2.53715200151623));
#6279=CARTESIAN_POINT('Ctrl Pts',(-11.8479967642311,23.9862445672002,-2.81498067748367));
#6280=CARTESIAN_POINT('Ctrl Pts',(-11.7790743410825,23.9973842855269,-3.09071503164591));
#6281=CARTESIAN_POINT('Ctrl Pts',(-11.7006058479935,24.0085240038537,-3.36366957947735));
#6282=CARTESIAN_POINT('Ctrl Pts',(-11.6335067433188,24.0180496758352,-3.59707543519565));
#6283=CARTESIAN_POINT('Ctrl Pts',(-11.5594283093542,24.0275753478167,-3.82844876548518));
#6284=CARTESIAN_POINT('Ctrl Pts',(-11.4785103889095,24.0371010197983,-4.05736977630798));
#6285=CARTESIAN_POINT('Ctrl Pts',(-11.3838171384972,24.0482483260728,-4.32526191297343));
#6286=CARTESIAN_POINT('Ctrl Pts',(-11.2797273169031,24.0593956323473,-4.58987760285483));
#6287=CARTESIAN_POINT('Ctrl Pts',(-11.1664931690163,24.0705429386218,-4.85055466481025));
#6288=CARTESIAN_POINT('Ctrl Pts',(-11.053278253932,24.081688351528,-5.11118745080703));
#6289=CARTESIAN_POINT('Ctrl Pts',(-10.9309222196804,24.0928337644342,-5.36788269991822));
#6290=CARTESIAN_POINT('Ctrl Pts',(-10.7997253247509,24.1039791773405,-5.61999850177324));
#6291=CARTESIAN_POINT('Ctrl Pts',(-10.6685429947127,24.115123352933,-5.87208631486202));
#6292=CARTESIAN_POINT('Ctrl Pts',(-10.5285218869459,24.1262675285254,-6.11959545930329));
#6293=CARTESIAN_POINT('Ctrl Pts',(-10.3800086368805,24.1374117041179,-6.36190780727653));
#6294=CARTESIAN_POINT('Ctrl Pts',(-10.2268184035207,24.14890683239,-6.61185106227649));
#6295=CARTESIAN_POINT('Ctrl Pts',(-10.0645926378427,24.1604019606621,-6.85626464349746));
#6296=CARTESIAN_POINT('Ctrl Pts',(-9.89376139950918,24.1718970889342,-7.09450037843273));
#6297=CARTESIAN_POINT('Ctrl Pts',(-9.72813688326918,24.1830418601,-7.32547498667565));
#6298=CARTESIAN_POINT('Ctrl Pts',(-9.55442385726194,24.1941866312657,-7.55064253139713));
#6299=CARTESIAN_POINT('Ctrl Pts',(-9.37305720387854,24.2053314024315,-7.76944328139543));
#6300=CARTESIAN_POINT('Ctrl Pts',(-9.18313814126281,24.2170017092568,-7.99856165880439));
#6301=CARTESIAN_POINT('Ctrl Pts',(-8.98482646679887,24.2286720160821,-8.22069809174982));
#6302=CARTESIAN_POINT('Ctrl Pts',(-8.77866826149681,24.2403423229074,-8.43524948087421));
#6303=CARTESIAN_POINT('Ctrl Pts',(-8.57251005619474,24.2520126297327,-8.6498008699986));
#6304=CARTESIAN_POINT('Ctrl Pts',(-8.35850555884004,24.263682936558,-8.85676697946432));
#6305=CARTESIAN_POINT('Ctrl Pts',(-8.13724527165577,24.2753532433833,-9.05558886207384));
#6306=CARTESIAN_POINT('Ctrl Pts',(-7.92590068440107,24.2865005496194,-9.24550061375804));
#6307=CARTESIAN_POINT('Ctrl Pts',(-7.70787322336667,24.2976478558555,-9.42803877404122));
#6308=CARTESIAN_POINT('Ctrl Pts',(-7.48370125772818,24.3087951620916,-9.60274261526766));
#6309=CARTESIAN_POINT('Ctrl Pts',(-7.25956736767171,24.3199405749591,-9.77741678306721));
#6310=CARTESIAN_POINT('Ctrl Pts',(-7.02929126696434,24.3310859878265,-9.94425912456056));
#6311=CARTESIAN_POINT('Ctrl Pts',(-6.79344378337951,24.342231400694,-10.1028496876902));
#6312=CARTESIAN_POINT('Ctrl Pts',(-6.55762248253287,24.3533755762473,-10.2614226448012));
#6313=CARTESIAN_POINT('Ctrl Pts',(-6.31623125517515,24.3645197518006,-10.4117455039978));
#6314=CARTESIAN_POINT('Ctrl Pts',(-6.06987027004878,24.3756639273539,-10.5534413891762));
#6315=CARTESIAN_POINT('Ctrl Pts',(-5.81575087656889,24.3871590556551,-10.6995995658927));
#6316=CARTESIAN_POINT('Ctrl Pts',(-5.55634388989934,24.3986541839563,-10.836578445479));
#6317=CARTESIAN_POINT('Ctrl Pts',(-5.29233710829935,24.4101493122576,-10.9640146927172));
#6318=CARTESIAN_POINT('Ctrl Pts',(-5.03637692415595,24.4212940833839,-11.0875668420671));
#6319=CARTESIAN_POINT('Ctrl Pts',(-4.776093436397,24.4324388545102,-11.2021493190998));
#6320=CARTESIAN_POINT('Ctrl Pts',(-4.51213635499412,24.4435836256365,-11.3074787536365));
#6321=CARTESIAN_POINT('Ctrl Pts',(-4.2357322807886,24.4552539325252,-11.4177750362176));
#6322=CARTESIAN_POINT('Ctrl Pts',(-3.95530011241909,24.4669242394138,-11.517924499486));
#6323=CARTESIAN_POINT('Ctrl Pts',(-3.67160795292729,24.4785945463025,-11.6076589065152));
#6324=CARTESIAN_POINT('Ctrl Pts',(-3.38791579343547,24.4902648531912,-11.6973933135444));
#6325=CARTESIAN_POINT('Ctrl Pts',(-3.10096396534875,24.5019351600798,-11.7767125715228));
#6326=CARTESIAN_POINT('Ctrl Pts',(-2.81153844769576,24.5136054669685,-11.8454084694082));
#6327=CARTESIAN_POINT('Ctrl Pts',(-2.53508343133578,24.5247527732184,-11.9110257851439));
#6328=CARTESIAN_POINT('Ctrl Pts',(-2.25628900057298,24.5359000794684,-11.9669705731406));
#6329=CARTESIAN_POINT('Ctrl Pts',(-1.97584835600998,24.5470473857183,-12.0130959175415));
#6330=CARTESIAN_POINT('Ctrl Pts',(-1.6954553442541,24.5581927985997,-12.0592134275587));
#6331=CARTESIAN_POINT('Ctrl Pts',(-1.41341694004873,24.5693382114812,-12.0955147805296));
#6332=CARTESIAN_POINT('Ctrl Pts',(-1.13043533186683,24.5804836243626,-12.1219043970189));
#6333=CARTESIAN_POINT('Ctrl Pts',(-0.847485139039559,24.59162779993,-12.1482910838509));
#6334=CARTESIAN_POINT('Ctrl Pts',(-0.563592216852303,24.6027719754975,-12.1647682066768));
#6335=CARTESIAN_POINT('Ctrl Pts',(-0.279463903351351,24.6139161510649,-12.1712920504244));
#6336=CARTESIAN_POINT('Ctrl Pts',(0.0136121878273971,24.6254112793557,-12.178021343262));
#6337=CARTESIAN_POINT('Ctrl Pts',(0.306938440053928,24.6369064076464,-12.1741602840482));
#6338=CARTESIAN_POINT('Ctrl Pts',(0.599737050830368,24.6484015359371,-12.1597189819445));
#6339=CARTESIAN_POINT('Ctrl Pts',(0.883611525722312,24.6595463070775,-12.1457178326885));
#6340=CARTESIAN_POINT('Ctrl Pts',(1.16698976785634,24.670691078218,-12.1217718491366));
#6341=CARTESIAN_POINT('Ctrl Pts',(1.44916568538033,24.6818358493584,-12.0879431280229));
#6342=CARTESIAN_POINT('Ctrl Pts',(1.7446477106423,24.6935061562243,-12.0525192012952));
#6343=CARTESIAN_POINT('Ctrl Pts',(2.0388109751728,24.7051764630901,-12.006258099938));
#6344=CARTESIAN_POINT('Ctrl Pts',(2.33085267230887,24.716846769956,-11.9492918647923));
#6345=CARTESIAN_POINT('Ctrl Pts',(2.62289436944495,24.7285170768218,-11.8923256296465));
#6346=CARTESIAN_POINT('Ctrl Pts',(2.91281417157252,24.7401873836877,-11.8246543335607));
#6347=CARTESIAN_POINT('Ctrl Pts',(3.19982230071158,24.7518576905535,-11.7464712783827));
#6348=CARTESIAN_POINT('Ctrl Pts',(3.47396826343337,24.7630049968009,-11.6717919687945));
#6349=CARTESIAN_POINT('Ctrl Pts',(3.74553966481412,24.7741523030483,-11.587500048405));
#6350=CARTESIAN_POINT('Ctrl Pts',(4.01385752465415,24.7852996092957,-11.4937982417379));
#6351=CARTESIAN_POINT('Ctrl Pts',(4.28212981073978,24.7964450221745,-11.4001123503108));
#6352=CARTESIAN_POINT('Ctrl Pts',(4.54714940684029,24.8075904350533,-11.2970198514592));
#6353=CARTESIAN_POINT('Ctrl Pts',(4.80825400749799,24.8187358479322,-11.1847728474645));
#6354=CARTESIAN_POINT('Ctrl Pts',(5.06932962149008,24.8298800234971,-11.0725383046305));
#6355=CARTESIAN_POINT('Ctrl Pts',(5.32649086291784,24.841024199062,-10.9511513913509));
#6356=CARTESIAN_POINT('Ctrl Pts',(5.57909572397968,24.8521683746269,-10.8209122144425));
#6357=CARTESIAN_POINT('Ctrl Pts',(5.83965562527876,24.8636635029195,-10.6865715412747));
#6358=CARTESIAN_POINT('Ctrl Pts',(6.09536724836163,24.8751586312122,-10.5428121455003));
#6359=CARTESIAN_POINT('Ctrl Pts',(6.34555247030226,24.8866537595048,-10.390015115323));
#6360=CARTESIAN_POINT('Ctrl Pts',(6.58811235911965,24.8977985306427,-10.2418751478064));
#6361=CARTESIAN_POINT('Ctrl Pts',(6.82547749579582,24.9089433017806,-10.0852404450836));
#6362=CARTESIAN_POINT('Ctrl Pts',(7.05705760223552,24.9200880729185,-9.92050342718201));
#6363=CARTESIAN_POINT('Ctrl Pts',(7.29955795273287,24.9317583797885,-9.74799817534841));
#6364=CARTESIAN_POINT('Ctrl Pts',(7.53571429569325,24.9434286866585,-9.56660827088475));
#6365=CARTESIAN_POINT('Ctrl Pts',(7.76488490244142,24.9550989935286,-9.37683383140799));
#6366=CARTESIAN_POINT('Ctrl Pts',(7.99405550918959,24.9667693003986,-9.18705939193122));
#6367=CARTESIAN_POINT('Ctrl Pts',(8.21624012692051,24.9784396072687,-8.98890063818444));
#6368=CARTESIAN_POINT('Ctrl Pts',(8.43083778298808,24.9901099141387,-8.78290524410578));
#6369=CARTESIAN_POINT('Ctrl Pts',(8.63581832193552,25.0012572203849,-8.58614145985624));
#6370=CARTESIAN_POINT('Ctrl Pts',(8.83393818577717,25.0124045266311,-8.38216922295967));
#6371=CARTESIAN_POINT('Ctrl Pts',(9.02469819859376,25.0235518328773,-8.17149145959895));
#6372=CARTESIAN_POINT('Ctrl Pts',(9.21542581084571,25.0346972457549,-7.96084947983034));
#6373=CARTESIAN_POINT('Ctrl Pts',(9.39879588886446,25.0458426586325,-7.74350444513577));
#6374=CARTESIAN_POINT('Ctrl Pts',(9.57434752759173,25.0569880715101,-7.5199946589674));
#6375=CARTESIAN_POINT('Ctrl Pts',(9.74987967736235,25.0681322470739,-7.2965096858544));
#6376=CARTESIAN_POINT('Ctrl Pts',(9.91759495631258,25.0792764226377,-7.06686153759513));
#6377=CARTESIAN_POINT('Ctrl Pts',(10.0770732542511,25.0904205982015,-6.83162095541444));
#6378=CARTESIAN_POINT('Ctrl Pts',(10.2415738477981,25.101915726495,-6.58897216937083));
#6379=CARTESIAN_POINT('Ctrl Pts',(10.3973100804441,25.1134108547885,-6.34037324759497));
#6380=CARTESIAN_POINT('Ctrl Pts',(10.5438688836484,25.1249059830821,-6.0864833208045));
#6381=CARTESIAN_POINT('Ctrl Pts',(10.6859607575328,25.1360507542187,-5.84033164196093));
#6382=CARTESIAN_POINT('Ctrl Pts',(10.8194262115696,25.1471955253553,-5.58920695028821));
#6383=CARTESIAN_POINT('Ctrl Pts',(10.9439347333879,25.1583402964919,-5.3337362890704));
#6384=CARTESIAN_POINT('Ctrl Pts',(11.0743144998257,25.1700106033639,-5.06621881592986));
#6385=CARTESIAN_POINT('Ctrl Pts',(11.19487213416,25.1816809102359,-4.79393592517833));
#6386=CARTESIAN_POINT('Ctrl Pts',(11.3052834849987,25.1933512171079,-4.51763384680682));
#6387=CARTESIAN_POINT('Ctrl Pts',(11.4156948358375,25.2050215239798,-4.2413317684353));
#6388=CARTESIAN_POINT('Ctrl Pts',(11.5159597868368,25.2166918308518,-3.96101081724842));
#6389=CARTESIAN_POINT('Ctrl Pts',(11.6058127307487,25.2283621377238,-3.67743947724378));
#6390=CARTESIAN_POINT('Ctrl Pts',(11.6916389471497,25.2395094439717,-3.4065762853131));
#6391=CARTESIAN_POINT('Ctrl Pts',(11.7679914973803,25.2506567502196,-3.13266673460072));
#6392=CARTESIAN_POINT('Ctrl Pts',(11.834672744551,25.2618040564674,-2.85639130361768));
#6393=CARTESIAN_POINT('Ctrl Pts',(11.9013426659205,25.2729494693468,-2.58016279798063));
#6394=CARTESIAN_POINT('Ctrl Pts',(11.9583445012586,25.2840948822262,-2.30156947355845));
#6395=CARTESIAN_POINT('Ctrl Pts',(12.0055311474859,25.2952402951056,-2.02130455813741));
#6396=CARTESIAN_POINT('Ctrl Pts',(12.0527125552623,25.3063844706709,-1.7410707564762));
#6397=CARTESIAN_POINT('Ctrl Pts',(12.0900809054865,25.3175286462363,-1.45916599735268));
#6398=CARTESIAN_POINT('Ctrl Pts',(12.1175404384541,25.3286728218017,-1.17629246891674));
#6399=CARTESIAN_POINT('Ctrl Pts',(12.1458647278962,25.340167950094,-0.884510678439701));
#6400=CARTESIAN_POINT('Ctrl Pts',(12.163645951052,25.3516630783862,-0.591698407265157));
#6401=CARTESIAN_POINT('Ctrl Pts',(12.1708368293856,25.3631582066785,-0.29863208546831));
#6402=CARTESIAN_POINT('Ctrl Pts',(12.1778085387284,25.3743029778168,-0.0144980591447471));
#6403=CARTESIAN_POINT('Ctrl Pts',(12.1748258979266,25.3854477489552,0.269874481842067));
#6404=CARTESIAN_POINT('Ctrl Pts',(12.1618987628609,25.3965925200936,0.553776788898335));
#6405=CARTESIAN_POINT('Ctrl Pts',(12.148362044046,25.4082628269628,0.851066612358317));
#6406=CARTESIAN_POINT('Ctrl Pts',(12.1239204060494,25.419933133832,1.14784046916088));
#6407=CARTESIAN_POINT('Ctrl Pts',(12.088646326029,25.4316034407012,1.44328800112304));
#6408=CARTESIAN_POINT('Ctrl Pts',(12.0533722460086,25.4432737475704,1.73873553308519));
#6409=CARTESIAN_POINT('Ctrl Pts',(12.0072657724544,25.4549440544397,2.03285640811261));
#6410=CARTESIAN_POINT('Ctrl Pts',(11.9504614375384,25.4666143613089,2.32484874344699));
#6411=CARTESIAN_POINT('Ctrl Pts',(11.8962027685468,25.4777616675556,2.60375554685274));
#6412=CARTESIAN_POINT('Ctrl Pts',(11.832167798918,25.4889089738023,2.88080369527671));
#6413=CARTESIAN_POINT('Ctrl Pts',(11.7585086287844,25.5000562800489,3.15530110715318));
#6414=CARTESIAN_POINT('Ctrl Pts',(11.6848619696517,25.5112016929271,3.4297518956788));
#6415=CARTESIAN_POINT('Ctrl Pts',(11.6015944427383,25.5223471058052,3.70165255508999));
#6416=CARTESIAN_POINT('Ctrl Pts',(11.5089086211831,25.5334925186833,3.97032399172388));
#6417=CARTESIAN_POINT('Ctrl Pts',(11.4162330891935,25.5446366942475,4.23896560165561));
#6418=CARTESIAN_POINT('Ctrl Pts',(11.3141414373819,25.5557808698117,4.5043784525661));
#6419=CARTESIAN_POINT('Ctrl Pts',(11.2028856095872,25.5669250453759,4.76590015301466));
#6420=CARTESIAN_POINT('Ctrl Pts',(11.0881261097483,25.5784201736691,5.03565770311674));
#6421=CARTESIAN_POINT('Ctrl Pts',(10.9636159909716,25.5899153019623,5.30127477407346));
#6422=CARTESIAN_POINT('Ctrl Pts',(10.8296852946106,25.6014104302554,5.56204698557055));
#6423=CARTESIAN_POINT('Ctrl Pts',(10.6998366386309,25.6125552013926,5.81487118569636));
#6424=CARTESIAN_POINT('Ctrl Pts',(10.5611332838991,25.6236999725298,6.06314123540553));
#6425=CARTESIAN_POINT('Ctrl Pts',(10.4139230509799,25.6348447436669,6.30623952433371));
#6426=CARTESIAN_POINT('Ctrl Pts',(10.2597710660175,25.6465150505381,6.56080120144097));
#6427=CARTESIAN_POINT('Ctrl Pts',(10.0962907731105,25.6581853574093,6.80969135715406));
#6428=CARTESIAN_POINT('Ctrl Pts',(9.92393360285792,25.6698556642805,7.05223312831244));
#6429=CARTESIAN_POINT('Ctrl Pts',(9.75157643260539,25.6815259711516,7.29477489947081));
#6430=CARTESIAN_POINT('Ctrl Pts',(9.57034258650591,25.6931962780228,7.53096801767879));
#6431=CARTESIAN_POINT('Ctrl Pts',(9.38073392759741,25.704866584894,7.76017275771763));
#6432=CARTESIAN_POINT('Ctrl Pts',(9.1996225128482,25.7160138911413,7.97910576939877));
#6433=CARTESIAN_POINT('Ctrl Pts',(9.01081632348767,25.7271611973887,8.19172838519741));
#6434=CARTESIAN_POINT('Ctrl Pts',(8.81478010379239,25.738308503636,8.39750569941967));
#6435=CARTESIAN_POINT('Ctrl Pts',(8.61877718082369,25.7494539165148,8.60324806239169));
#6436=CARTESIAN_POINT('Ctrl Pts',(8.41554686318361,25.7605993293936,8.80214725200337));
#6437=CARTESIAN_POINT('Ctrl Pts',(8.20559199842654,25.7717447422724,8.99370392026324));
#6438=CARTESIAN_POINT('Ctrl Pts',(7.99566044192285,25.7828889178371,9.1852393227555));
#6439=CARTESIAN_POINT('Ctrl Pts',(7.77900602600686,25.7940330934018,9.36943365184792));
#6440=CARTESIAN_POINT('Ctrl Pts',(7.55616695615486,25.8051772689665,9.54582585116204));
#6441=CARTESIAN_POINT('Ctrl Pts',(7.32631023129463,25.8166723972593,9.72777299917411));
#6442=CARTESIAN_POINT('Ctrl Pts',(7.08987323231034,25.828167525552,9.90141845280155));
#6443=CARTESIAN_POINT('Ctrl Pts',(6.84748283278494,25.8396626538447,10.0663016597316));
#6444=CARTESIAN_POINT('Ctrl Pts',(6.612480189934,25.8508074249824,10.2261594324247));
#6445=CARTESIAN_POINT('Ctrl Pts',(6.37188190783972,25.8619521961202,10.3777810168315));
#6446=CARTESIAN_POINT('Ctrl Pts',(6.12628894824933,25.8730969672579,10.5207905583448));
#6447=CARTESIAN_POINT('Ctrl Pts',(5.86911496341343,25.8847672741281,10.6705437667506));
#6448=CARTESIAN_POINT('Ctrl Pts',(5.60646418974834,25.8964375809983,10.8108530211056));
#6449=CARTESIAN_POINT('Ctrl Pts',(5.33905692026464,25.9081078878685,10.9413400208646));
#6450=CARTESIAN_POINT('Ctrl Pts',(5.07164965078095,25.9197781947387,11.0718270206237));
#6451=CARTESIAN_POINT('Ctrl Pts',(4.79948619084612,25.9314485016088,11.1924916265437));
#6452=CARTESIAN_POINT('Ctrl Pts',(4.52331334430271,25.943118808479,11.3030122816554));
#6453=CARTESIAN_POINT('Ctrl Pts',(4.25951707437787,25.954266115174,11.4085799974284));
#6454=CARTESIAN_POINT('Ctrl Pts',(3.99198409131871,25.9654134218689,11.5049245009964));
#6455=CARTESIAN_POINT('Ctrl Pts',(3.72137844577119,25.9765607285639,11.5917985107295));
#6456=CARTESIAN_POINT('Ctrl Pts',(3.45082167223791,25.9877060220291,11.6786568308126));
#6457=CARTESIAN_POINT('Ctrl Pts',(3.17719359814242,25.9988513154943,11.7560479907674));
#6458=CARTESIAN_POINT('Ctrl Pts',(2.90117469334908,26.0099966089595,11.8237741710788));
#6459=CARTESIAN_POINT('Ctrl Pts',(2.62517723677871,26.0211410363727,11.8914950886848));
#6460=CARTESIAN_POINT('Ctrl Pts',(2.34678957918977,26.0322854637858,11.9495524615316));
#6461=CARTESIAN_POINT('Ctrl Pts',(2.06670498175388,26.043429891199,11.9977989968324));
#6462=CARTESIAN_POINT('Ctrl Pts',(1.90856353651569,26.0497222609815,12.025039969346));
#6463=CARTESIAN_POINT('Ctrl Pts',(1.749881326521,26.0560146307641,12.0491542053372));
#6464=CARTESIAN_POINT('Ctrl Pts',(1.59078448392775,26.0623070005467,12.0701224093086));
#6465=CARTESIAN_POINT('Ctrl Pts',(1.59078448392772,23.0623012722853,12.0701224093086));
#6466=CARTESIAN_POINT('Ctrl Pts',(1.40719576191192,23.0695648900095,12.0943185260093));
#6467=CARTESIAN_POINT('Ctrl Pts',(1.22306953313744,23.0768285077337,12.1143233119144));
#6468=CARTESIAN_POINT('Ctrl Pts',(1.03860091274412,23.0840921254579,12.1301178227603));
#6469=CARTESIAN_POINT('Ctrl Pts',(0.755501187515748,23.0952394315824,12.1543572932515));
#6470=CARTESIAN_POINT('Ctrl Pts',(0.471510238288568,23.1063867377068,12.1686853376153));
#6471=CARTESIAN_POINT('Ctrl Pts',(0.187335335693578,23.1175340438313,12.1730586017648));
#6472=CARTESIAN_POINT('Ctrl Pts',(-0.0967912998095614,23.1286794565864,
12.1774311231157));
#6473=CARTESIAN_POINT('Ctrl Pts',(-0.381101559686401,23.1398248693415,12.1718522358687));
#6474=CARTESIAN_POINT('Ctrl Pts',(-0.664886834336528,23.1509702820966,12.1563306860058));
#6475=CARTESIAN_POINT('Ctrl Pts',(-0.948640604399958,23.1621144575373,12.1408108592767));
#6476=CARTESIAN_POINT('Ctrl Pts',(-1.2318692393348,23.1732586329779,12.1153505885898));
#6477=CARTESIAN_POINT('Ctrl Pts',(-1.51386666477452,23.1844028084186,12.0800106776147));
#6478=CARTESIAN_POINT('Ctrl Pts',(-1.80474476760346,23.195897936804,12.0435578403501));
#6479=CARTESIAN_POINT('Ctrl Pts',(-2.09431256209703,23.2073930651893,11.9965930464181));
#6480=CARTESIAN_POINT('Ctrl Pts',(-2.38180219291559,23.2188881935747,11.9392407029854));
#6481=CARTESIAN_POINT('Ctrl Pts',(-2.66052949347102,23.2300329645888,11.8836363884227));
#6482=CARTESIAN_POINT('Ctrl Pts',(-2.93730316054589,23.2411777356028,11.8182684020138));
#6483=CARTESIAN_POINT('Ctrl Pts',(-3.21143391640613,23.2523225066169,11.743302025008));
#6484=CARTESIAN_POINT('Ctrl Pts',(-3.49849141578957,23.2639928136879,11.6648005790335));
#6485=CARTESIAN_POINT('Ctrl Pts',(-3.78265044479703,23.2756631207589,11.5757738130286));
#6486=CARTESIAN_POINT('Ctrl Pts',(-4.06313635096133,23.2873334278299,11.4764704174888));
#6487=CARTESIAN_POINT('Ctrl Pts',(-4.34362225712563,23.299003734901,11.3771670219491));
#6488=CARTESIAN_POINT('Ctrl Pts',(-4.62043472711151,23.310674041972,11.2675871171198));
#6489=CARTESIAN_POINT('Ctrl Pts',(-4.89282100638345,23.322344349043,11.1480380717637));
#6490=CARTESIAN_POINT('Ctrl Pts',(-5.15300038646404,23.3334916552407,11.0338465765346));
#6491=CARTESIAN_POINT('Ctrl Pts',(-5.40921927779757,23.3446389614383,10.9105257231928));
#6492=CARTESIAN_POINT('Ctrl Pts',(-5.66083590451648,23.355786267636,10.7783759032675));
#6493=CARTESIAN_POINT('Ctrl Pts',(-5.91240979416356,23.3669316804642,10.6462485289827));
#6494=CARTESIAN_POINT('Ctrl Pts',(-6.15938274378058,23.3780770932925,10.5052953060483));
#6495=CARTESIAN_POINT('Ctrl Pts',(-6.40113673390645,23.3892225061207,10.3558630139566));
#6496=CARTESIAN_POINT('Ctrl Pts',(-6.64286388556777,23.4003666816343,10.2064473111806));
#6497=CARTESIAN_POINT('Ctrl Pts',(-6.87937300783742,23.4115108571478,10.0485545591068));
#6498=CARTESIAN_POINT('Ctrl Pts',(-7.11007321917927,23.4226550326614,9.882576034006));
#6499=CARTESIAN_POINT('Ctrl Pts',(-7.34803865072143,23.4341501609919,9.71137050661351));
#6500=CARTESIAN_POINT('Ctrl Pts',(-7.57982312721504,23.4456452893225,9.53156184412831));
#6501=CARTESIAN_POINT('Ctrl Pts',(-7.80481195646738,23.457140417653,9.34362673559812));
#6502=CARTESIAN_POINT('Ctrl Pts',(-8.02294340543191,23.4682851887384,9.16141965593453));
#6503=CARTESIAN_POINT('Ctrl Pts',(-8.23468710462325,23.4794299598237,8.97157434171908));
#6504=CARTESIAN_POINT('Ctrl Pts',(-8.43951691801119,23.4905747309091,8.77456576934739));
#6505=CARTESIAN_POINT('Ctrl Pts',(-8.65400555820757,23.5022450378623,8.56826718372596));
#6506=CARTESIAN_POINT('Ctrl Pts',(-8.86091234015456,23.5139153448154,8.35411373254376));
#6507=CARTESIAN_POINT('Ctrl Pts',(-9.05967607823019,23.5255856517686,8.13269448630303));
#6508=CARTESIAN_POINT('Ctrl Pts',(-9.2584398163058,23.5372559587218,7.91127524006232));
#6509=CARTESIAN_POINT('Ctrl Pts',(-9.44906029292414,23.5489262656749,7.68259045429057));
#6510=CARTESIAN_POINT('Ctrl Pts',(-9.631023630308,23.5605965726281,7.44727024368318));
#6511=CARTESIAN_POINT('Ctrl Pts',(-9.8048323458045,23.5717438789489,7.22249582415408));
#6512=CARTESIAN_POINT('Ctrl Pts',(-9.97079470968131,23.5828911852698,6.99160050424424));
#6513=CARTESIAN_POINT('Ctrl Pts',(-10.128490951645,23.5940384915906,6.75515516420202));
#6514=CARTESIAN_POINT('Ctrl Pts',(-10.286160408936,23.6051839045438,6.51874998434983));
#6515=CARTESIAN_POINT('Ctrl Pts',(-10.4355663994461,23.6163293174971,6.27679688823947));
#6516=CARTESIAN_POINT('Ctrl Pts',(-10.5763322111555,23.6274747304504,6.0298961192773));
#6517=CARTESIAN_POINT('Ctrl Pts',(-10.7170823956828,23.6386189060904,5.78302276011893));
#6518=CARTESIAN_POINT('Ctrl Pts',(-10.8491941846832,23.6497630817305,5.53120305658148));
#6519=CARTESIAN_POINT('Ctrl Pts',(-10.9723359885886,23.6609072573705,5.27506333644663));
#6520=CARTESIAN_POINT('Ctrl Pts',(-11.0993557765869,23.6724023856074,5.01085725924436));
#6521=CARTESIAN_POINT('Ctrl Pts',(-11.2168313213538,23.6838975138443,4.74205492746937));
#6522=CARTESIAN_POINT('Ctrl Pts',(-11.3244509997133,23.6953926420812,4.46936906118676));
#6523=CARTESIAN_POINT('Ctrl Pts',(-11.4287905658947,23.7065374132952,4.20499431647958));
#6524=CARTESIAN_POINT('Ctrl Pts',(-11.5238660555388,23.7176821845091,3.93696952183191));
#6525=CARTESIAN_POINT('Ctrl Pts',(-11.6094427838768,23.7288269557231,3.66596351562464));
#6526=CARTESIAN_POINT('Ctrl Pts',(-11.6990549123853,23.7404972624715,3.38217812762871));
#6527=CARTESIAN_POINT('Ctrl Pts',(-11.7782507937505,23.7521675692198,3.09512390584126));
#6528=CARTESIAN_POINT('Ctrl Pts',(-11.8468195663286,23.7638378759682,2.80558664326246));
#6529=CARTESIAN_POINT('Ctrl Pts',(-11.9153883389068,23.7755081827165,2.51604938068365));
#6530=CARTESIAN_POINT('Ctrl Pts',(-11.9733299339243,23.7871784894648,2.22402940580713));
#6531=CARTESIAN_POINT('Ctrl Pts',(-12.0204946704578,23.7988487962132,1.93032591224761));
#6532=CARTESIAN_POINT('Ctrl Pts',(-12.0672414471629,23.8104156841837,1.63922513145235));
#6533=CARTESIAN_POINT('Ctrl Pts',(-12.1034122499846,23.8219825721543,1.34640866791079));
#6534=CARTESIAN_POINT('Ctrl Pts',(-12.1289081894145,23.8335494601249,1.05263307128082));
#6535=CARTESIAN_POINT('Ctrl Pts',(-12.1543967460716,23.8451129987108,0.758942542255195));
#6536=CARTESIAN_POINT('Ctrl Pts',(-12.1692165959912,23.8566765372968,0.464293654495028));
#6537=CARTESIAN_POINT('Ctrl Pts',(-12.1733207336769,23.8682400758828,0.169447823923155));
#6538=CARTESIAN_POINT('Ctrl Pts',(-12.1741055719096,23.8704513825889,0.11306416959796));
#6539=CARTESIAN_POINT('Ctrl Pts',(-12.1744986969062,23.872662689295,0.056673323816421));
#6540=CARTESIAN_POINT('Ctrl Pts',(-12.1744999967658,23.8748739960011,0.000280623926556051));
#6541=CARTESIAN_POINT('',(-12.1744999959752,23.6251260039651,0.000313050724133792));
#6542=CARTESIAN_POINT('Ctrl Pts',(1.5908148051505,22.812547089465,12.070351758578));
#6543=CARTESIAN_POINT('Ctrl Pts',(1.19923622262038,22.8280402873171,12.1223796458547));
#6544=CARTESIAN_POINT('Ctrl Pts',(-1.21473510391254,22.9229508930308,12.3241400337495));
#6545=CARTESIAN_POINT('Ctrl Pts',(-5.69424089117864,23.0972789066063,11.3422716237698));
#6546=CARTESIAN_POINT('Ctrl Pts',(-10.4276708680614,23.3355311301914,7.23430593172712));
#6547=CARTESIAN_POINT('Ctrl Pts',(-12.0452929662932,23.5114801626443,2.89768759261325));
#6548=CARTESIAN_POINT('Ctrl Pts',(-12.1750513728812,23.6080117872355,0.436676266174656));
#6549=CARTESIAN_POINT('Ctrl Pts',(-12.1746001704992,23.6251260039651,0.000313053299986626));
#6550=CARTESIAN_POINT('Ctrl Pts',(-12.1744999959752,23.6251260039651,0.000313050724133792));
#6551=CARTESIAN_POINT('Ctrl Pts',(-12.1745072760035,23.6362300684397,-0.28280626030774));
#6552=CARTESIAN_POINT('Ctrl Pts',(-12.1646342579426,23.6473341329143,-0.565958783664843));
#6553=CARTESIAN_POINT('Ctrl Pts',(-12.1449000764791,23.6584381973888,-0.848441148423234));
#6554=CARTESIAN_POINT('Ctrl Pts',(-12.1251680288802,23.6695410611767,-1.13089296825575));
#6555=CARTESIAN_POINT('Ctrl Pts',(-12.0955769658755,23.6806439249646,-1.41267450420121));
#6556=CARTESIAN_POINT('Ctrl Pts',(-12.0561980343215,23.6917467887524,-1.69308570581112));
#6557=CARTESIAN_POINT('Ctrl Pts',(-12.0168162232634,23.7028504644146,-1.97351741191864));
#6558=CARTESIAN_POINT('Ctrl Pts',(-11.9676451482731,23.7139541400767,-2.25257831493435));
#6559=CARTESIAN_POINT('Ctrl Pts',(-11.9088076155506,23.7250578157389,-2.52957534495496));
#6560=CARTESIAN_POINT('Ctrl Pts',(-11.8499700831609,23.7361614913382,-2.80657237340874));
#6561=CARTESIAN_POINT('Ctrl Pts',(-11.7814661517746,23.7472651669375,-3.08150526454602));
#6562=CARTESIAN_POINT('Ctrl Pts',(-11.7034695576592,23.7583688425369,-3.35369207932761));
#6563=CARTESIAN_POINT('Ctrl Pts',(-11.6254556305768,23.7694749856753,-3.62593938143092));
#6564=CARTESIAN_POINT('Ctrl Pts',(-11.5379448995412,23.7805811288137,-3.89543912724969));
#6565=CARTESIAN_POINT('Ctrl Pts',(-11.4411611446377,23.7916872719521,-4.16152398916932));
#6566=CARTESIAN_POINT('Ctrl Pts',(-11.3820531543148,23.7984700404219,-4.3240279285868));
#6567=CARTESIAN_POINT('Ctrl Pts',(-11.3194874657191,23.8052528088917,-4.48525848955029));
#6568=CARTESIAN_POINT('Ctrl Pts',(-11.2535239975975,23.8120355773616,-4.64506704854697));
#6569=CARTESIAN_POINT('Ctrl Pts',(-11.1451147212248,23.8231828842355,-4.90770833670762));
#6570=CARTESIAN_POINT('Ctrl Pts',(-11.027490726027,23.8343301911093,-5.1665920149544));
#6571=CARTESIAN_POINT('Ctrl Pts',(-10.9009381361996,23.8454774979832,-5.42106982068579));
#6572=CARTESIAN_POINT('Ctrl Pts',(-10.7744070412407,23.8566229114949,-5.67550440354045));
#6573=CARTESIAN_POINT('Ctrl Pts',(-10.6389504981074,23.8677683250065,-5.9255343691766));
#6574=CARTESIAN_POINT('Ctrl Pts',(-10.4949015330221,23.8789137385181,-6.17053417964529));
#6575=CARTESIAN_POINT('Ctrl Pts',(-10.3508685595493,23.8900579147204,-6.41550679143171));
#6576=CARTESIAN_POINT('Ctrl Pts',(-10.1982452040525,23.9012020909227,-6.65545013324551));
#6577=CARTESIAN_POINT('Ctrl Pts',(-10.037409578847,23.9123462671249,-6.88976481430757));
#6578=CARTESIAN_POINT('Ctrl Pts',(-9.87150892940053,23.9238413949434,-7.13145851688982));
#6579=CARTESIAN_POINT('Ctrl Pts',(-9.69687054816424,23.9353365227619,-7.36716304913461));
#6580=CARTESIAN_POINT('Ctrl Pts',(-9.51395741258113,23.9468316505804,-7.59625332658098));
#6581=CARTESIAN_POINT('Ctrl Pts',(-9.33661922343069,23.957976422359,-7.8183612403992));
#6582=CARTESIAN_POINT('Ctrl Pts',(-9.1515033916188,23.9691211941376,-8.03425189815682));
#6583=CARTESIAN_POINT('Ctrl Pts',(-8.95907314105923,23.9802659659162,-8.24338878757706));
#6584=CARTESIAN_POINT('Ctrl Pts',(-8.75756880151721,23.9919362717546,-8.4623875710529));
#6585=CARTESIAN_POINT('Ctrl Pts',(-8.54804383413787,24.003606577593,-8.67398007541675));
#6586=CARTESIAN_POINT('Ctrl Pts',(-8.33107475358735,24.0152768834315,-8.87759222425425));
#6587=CARTESIAN_POINT('Ctrl Pts',(-8.11410567303683,24.0269471892699,-9.08120437309175));
#6588=CARTESIAN_POINT('Ctrl Pts',(-7.88969272996757,24.0386174951083,-9.27683594321905));
#6589=CARTESIAN_POINT('Ctrl Pts',(-7.65845451946485,24.0502878009467,-9.46395924670476));
#6590=CARTESIAN_POINT('Ctrl Pts',(-7.43757914943243,24.0614351070725,-9.64269670021316));
#6591=CARTESIAN_POINT('Ctrl Pts',(-7.21041084144513,24.0725824131983,-9.81372509541071));
#6592=CARTESIAN_POINT('Ctrl Pts',(-6.97751105217776,24.0837297193241,-9.97661213873413));
#6593=CARTESIAN_POINT('Ctrl Pts',(-6.74465082092712,24.0948751320805,-10.139471515702));
#6594=CARTESIAN_POINT('Ctrl Pts',(-6.50606127048044,24.1060205448369,-10.2941921487503));
#6595=CARTESIAN_POINT('Ctrl Pts',(-6.26233416579329,24.1171659575934,-10.4403841426424));
#6596=CARTESIAN_POINT('Ctrl Pts',(-6.01863411861028,24.1283101330354,-10.5865599069465));
#6597=CARTESIAN_POINT('Ctrl Pts',(-5.76979788477571,24.1394543084775,-10.7242087855524));
#6598=CARTESIAN_POINT('Ctrl Pts',(-5.51644430519778,24.1505984839195,-10.8529854177388));
#6599=CARTESIAN_POINT('Ctrl Pts',(-5.25511210174971,24.1620936123039,-10.9858174902043));
#6600=CARTESIAN_POINT('Ctrl Pts',(-4.9889736812031,24.1735887406883,-11.1092093074788));
#6601=CARTESIAN_POINT('Ctrl Pts',(-4.71873469727067,24.1850838690726,-11.2228335596129));
#6602=CARTESIAN_POINT('Ctrl Pts',(-4.45673226505212,24.196228640088,-11.3329946843513));
#6603=CARTESIAN_POINT('Ctrl Pts',(-4.19087578555295,24.2073734111034,-11.4339747257494));
#6604=CARTESIAN_POINT('Ctrl Pts',(-3.92182874309239,24.2185181821189,-11.5255242639914));
#6605=CARTESIAN_POINT('Ctrl Pts',(-3.64009468169887,24.2301884891877,-11.6213908566577));
#6606=CARTESIAN_POINT('Ctrl Pts',(-3.35486221345111,24.2418587962565,-11.7069160450841));
#6607=CARTESIAN_POINT('Ctrl Pts',(-3.06691227567061,24.2535291033253,-11.7818716400808));
#6608=CARTESIAN_POINT('Ctrl Pts',(-2.77896233789011,24.2651994103942,-11.8568272350776));
#6609=CARTESIAN_POINT('Ctrl Pts',(-2.48829525746922,24.276869717463,-11.9212131606227));
#6610=CARTESIAN_POINT('Ctrl Pts',(-2.19570672218016,24.2885400245318,-11.9748620969167));
#6611=CARTESIAN_POINT('Ctrl Pts',(-1.91623044331381,24.2996873307296,-12.0261067742441));
#6612=CARTESIAN_POINT('Ctrl Pts',(-1.63491767399143,24.3108346369273,-12.0675709631649));
#6613=CARTESIAN_POINT('Ctrl Pts',(-1.35246828020352,24.3219819431251,-12.0991437631364));
#6614=CARTESIAN_POINT('Ctrl Pts',(-1.07006686043198,24.3331273559534,-12.1307112004694));
#6615=CARTESIAN_POINT('Ctrl Pts',(-0.786529466626027,24.3442727687818,-12.1523905734547));
#6616=CARTESIAN_POINT('Ctrl Pts',(-0.502562287985054,24.3554181816101,-12.1641227138128));
#6617=CARTESIAN_POINT('Ctrl Pts',(-0.218626634131015,24.3665623571237,-12.1758535517201));
#6618=CARTESIAN_POINT('Ctrl Pts',(0.0657384428316171,24.3777065326373,-12.1776393510993));
#6619=CARTESIAN_POINT('Ctrl Pts',(0.349824290943899,24.388850708151,-12.1694730048374));
#6620=CARTESIAN_POINT('Ctrl Pts',(0.642856581841975,24.4003458364815,-12.1610494836753));
#6621=CARTESIAN_POINT('Ctrl Pts',(0.935591475061742,24.411840964812,-12.1420368316069));
#6622=CARTESIAN_POINT('Ctrl Pts',(1.22725272951155,24.4233360931424,-12.1124853348892));
#6623=CARTESIAN_POINT('Ctrl Pts',(1.51002451090461,24.434480864228,-12.0838345311154));
#6624=CARTESIAN_POINT('Ctrl Pts',(1.79178685310391,24.4456256353135,-12.0452778196722));
#6625=CARTESIAN_POINT('Ctrl Pts',(2.07183781618613,24.456770406399,-11.9969136995071));
#6626=CARTESIAN_POINT('Ctrl Pts',(2.36509468764385,24.468440713352,-11.9462689510859));
#6627=CARTESIAN_POINT('Ctrl Pts',(2.65647458170317,24.480111020305,-11.8848696481258));
#6628=CARTESIAN_POINT('Ctrl Pts',(2.94518258695251,24.4917813272579,-11.8128891376967));
#6629=CARTESIAN_POINT('Ctrl Pts',(3.23389059220187,24.5034516342109,-11.7409086272675));
#6630=CARTESIAN_POINT('Ctrl Pts',(3.51992638522904,24.5151219411639,-11.6583469990491));
#6631=CARTESIAN_POINT('Ctrl Pts',(3.8025112313794,24.5267922481169,-11.5654381060656));
#6632=CARTESIAN_POINT('Ctrl Pts',(4.07243213870612,24.5379395544373,-11.4766928918955));
#6633=CARTESIAN_POINT('Ctrl Pts',(4.33928522123258,24.5490868607576,-11.3784809408964));
#6634=CARTESIAN_POINT('Ctrl Pts',(4.60240288097398,24.560234167078,-11.2710397910398));
#6635=CARTESIAN_POINT('Ctrl Pts',(4.86547585023803,24.5713795800308,-11.1636168900391));
#6636=CARTESIAN_POINT('Ctrl Pts',(5.12481441655924,24.5825249929836,-11.0469680206508));
#6637=CARTESIAN_POINT('Ctrl Pts',(5.37977018586658,24.5936704059364,-10.9213791710233));
#6638=CARTESIAN_POINT('Ctrl Pts',(5.63469765113895,24.604814581576,-10.7958042637012));
#6639=CARTESIAN_POINT('Ctrl Pts',(5.88524305174738,24.6159587572155,-10.6612914757993));
#6640=CARTESIAN_POINT('Ctrl Pts',(6.13078074465165,24.627102932855,-10.5181736870527));
#6641=CARTESIAN_POINT('Ctrl Pts',(6.38405091539444,24.6385980610923,-10.3705488300972));
#6642=CARTESIAN_POINT('Ctrl Pts',(6.63199260058101,24.6500931893295,-10.2137683531929));
#6643=CARTESIAN_POINT('Ctrl Pts',(6.87394827478413,24.6615883175668,-10.0482478754056));
#6644=CARTESIAN_POINT('Ctrl Pts',(7.10852944492335,24.6727330887802,-9.88777225321056));
#6645=CARTESIAN_POINT('Ctrl Pts',(7.33748386258186,24.6838778599937,-9.71908166691572));
#6646=CARTESIAN_POINT('Ctrl Pts',(7.5602423153278,24.6950226312072,-9.54259851316857));
#6647=CARTESIAN_POINT('Ctrl Pts',(7.79350501984766,24.7066929379563,-9.35779323535402));
#6648=CARTESIAN_POINT('Ctrl Pts',(8.01997310417797,24.7183632447054,-9.16444298150568));
#6649=CARTESIAN_POINT('Ctrl Pts',(8.23903153901835,24.7300335514546,-8.96308036051563));
#6650=CARTESIAN_POINT('Ctrl Pts',(8.45808997385872,24.7417038582037,-8.76171773952559));
#6651=CARTESIAN_POINT('Ctrl Pts',(8.66973851814809,24.7533741649529,-8.55234298490495));
#6652=CARTESIAN_POINT('Ctrl Pts',(8.87340530149632,24.765044471702,-8.33553409238886));
#6653=CARTESIAN_POINT('Ctrl Pts',(9.0679448319984,24.7761917778973,-8.12844141156305));
#6654=CARTESIAN_POINT('Ctrl Pts',(9.25526037748929,24.7873390840926,-7.91450441257048));
#6655=CARTESIAN_POINT('Ctrl Pts',(9.43487941609193,24.7984863902879,-7.69425114314608));
#6656=CARTESIAN_POINT('Ctrl Pts',(9.61446794641304,24.8096318031139,-7.47403528372458));
#6657=CARTESIAN_POINT('Ctrl Pts',(9.78636241125291,24.82077721594,-7.24750550239521));
#6658=CARTESIAN_POINT('Ctrl Pts',(9.95013033648356,24.8319226287661,-7.01522319937076));
#6659=CARTESIAN_POINT('Ctrl Pts',(10.1138800809248,24.8430668042778,-6.78296668329837));
#6660=CARTESIAN_POINT('Ctrl Pts',(10.2695049335853,24.8542109797896,-6.54495913870715));
#6661=CARTESIAN_POINT('Ctrl Pts',(10.4166148368308,24.8653551553013,-6.30179225229755));
#6662=CARTESIAN_POINT('Ctrl Pts',(10.5683575310261,24.8768502836335,-6.05096754458694));
#6663=CARTESIAN_POINT('Ctrl Pts',(10.711040117134,24.8883454119656,-5.79465352177918));
#6664=CARTESIAN_POINT('Ctrl Pts',(10.8442841370161,24.8998405402978,-5.53352977814893));
#6665=CARTESIAN_POINT('Ctrl Pts',(10.973467044506,24.9109853113819,-5.28036476221306));
#6666=CARTESIAN_POINT('Ctrl Pts',(11.0937780907119,24.9221300824661,-5.02267912115139));
#6667=CARTESIAN_POINT('Ctrl Pts',(11.2049196053669,24.9332748535502,-4.761116138813));
#6668=CARTESIAN_POINT('Ctrl Pts',(11.3213020399456,24.9449451605064,-4.48721905566886));
#6669=CARTESIAN_POINT('Ctrl Pts',(11.4276292249522,24.9566154674625,-4.20907045001883));
#6670=CARTESIAN_POINT('Ctrl Pts',(11.5236160012059,24.9682857744187,-3.92743230454083));
#6671=CARTESIAN_POINT('Ctrl Pts',(11.6196027774596,24.9799560813748,-3.64579415906282));
#6672=CARTESIAN_POINT('Ctrl Pts',(11.7052490450383,24.991626388331,-3.36066679415267));
#6673=CARTESIAN_POINT('Ctrl Pts',(11.7803292606082,25.0032966952871,-3.07283139167434));
#6674=CARTESIAN_POINT('Ctrl Pts',(11.8520447828511,25.0144440015614,-2.79789523103511));
#6675=CARTESIAN_POINT('Ctrl Pts',(11.9141418832278,25.0255913078357,-2.52040630438659));
#6676=CARTESIAN_POINT('Ctrl Pts',(11.9664583505487,25.03673861411,-2.24105439349054));
#6677=CARTESIAN_POINT('Ctrl Pts',(12.0187659319259,25.047884027016,-1.96174993047246));
#6678=CARTESIAN_POINT('Ctrl Pts',(12.0612961478269,25.0590294399221,-1.680583377044));
#6679=CARTESIAN_POINT('Ctrl Pts',(12.0939379121453,25.0701748528282,-1.39825463602789));
#6680=CARTESIAN_POINT('Ctrl Pts',(12.1265760527213,25.0813190284204,-1.11595723788416));
#6681=CARTESIAN_POINT('Ctrl Pts',(12.1493279031616,25.0924632040126,-0.832498174701055));
#6682=CARTESIAN_POINT('Ctrl Pts',(12.1621341151456,25.1036073796049,-0.548583644680526));
#6683=CARTESIAN_POINT('Ctrl Pts',(12.1753436207048,25.1151025078772,-0.255728070579462));
#6684=CARTESIAN_POINT('Ctrl Pts',(12.1779708973995,25.1265976361494,0.0376118263910138));
#6685=CARTESIAN_POINT('Ctrl Pts',(12.1700088495403,25.1380927644217,0.330658210410661));
#6686=CARTESIAN_POINT('Ctrl Pts',(12.1622894749236,25.1492375355872,0.61477290782209));
#6687=CARTESIAN_POINT('Ctrl Pts',(12.1446167235003,25.1603823067528,0.898611440186133));
#6688=CARTESIAN_POINT('Ctrl Pts',(12.1170370604352,25.1715270779183,1.18146651498856));
#6689=CARTESIAN_POINT('Ctrl Pts',(12.0881568685195,25.1831973847439,1.47765972174982));
#6690=CARTESIAN_POINT('Ctrl Pts',(12.0484129862963,25.1948676915696,1.77277417226269));
#6691=CARTESIAN_POINT('Ctrl Pts',(11.9979196669199,25.2065379983952,2.06600433594332));
#6692=CARTESIAN_POINT('Ctrl Pts',(11.9474263475436,25.2182083052209,2.35923449962396));
#6693=CARTESIAN_POINT('Ctrl Pts',(11.8861836565992,25.2298786120466,2.65058004732725));
#6694=CARTESIAN_POINT('Ctrl Pts',(11.814367381413,25.2415489188722,2.93924711907746));
#6695=CARTESIAN_POINT('Ctrl Pts',(11.7457695266862,25.2526962251084,3.21497768016523));
#6696=CARTESIAN_POINT('Ctrl Pts',(11.6675044717985,25.2638435313446,3.48834690833357));
#6697=CARTESIAN_POINT('Ctrl Pts',(11.5797598749238,25.2749908375808,3.75867150587886));
#6698=CARTESIAN_POINT('Ctrl Pts',(11.4920301814584,25.2861362504483,4.02895018882332));
#6699=CARTESIAN_POINT('Ctrl Pts',(11.3948242428908,25.2972816633159,4.29618501997487));
#6700=CARTESIAN_POINT('Ctrl Pts',(11.2883794518641,25.3084270761834,4.55970828022289));
#6701=CARTESIAN_POINT('Ctrl Pts',(11.1819464778628,25.319571251737,4.82320228529501));
#6702=CARTESIAN_POINT('Ctrl Pts',(11.0662767993538,25.3307154272905,5.08298529497744));
#6703=CARTESIAN_POINT('Ctrl Pts',(10.9416562506894,25.3418596028441,5.33840882115168));
#6704=CARTESIAN_POINT('Ctrl Pts',(10.8131111475577,25.3533547311452,5.60187615351543));
#6705=CARTESIAN_POINT('Ctrl Pts',(10.6750423980179,25.3648498594463,5.86070470407446));
#6706=CARTESIAN_POINT('Ctrl Pts',(10.5278159992574,25.3763449877474,6.11420808737982));
#6707=CARTESIAN_POINT('Ctrl Pts',(10.3850768775203,25.3874897588738,6.35998500371434));
#6708=CARTESIAN_POINT('Ctrl Pts',(10.233730207958,25.3986345300003,6.60075631358498));
#6709=CARTESIAN_POINT('Ctrl Pts',(10.0741552596408,25.4097793011267,6.83592320426813));
#6710=CARTESIAN_POINT('Ctrl Pts',(9.90705549622338,25.4214496080151,7.08217947576419));
#6711=CARTESIAN_POINT('Ctrl Pts',(9.7309329452156,25.4331199149036,7.322289790146));
#6712=CARTESIAN_POINT('Ctrl Pts',(9.54627340902399,25.444790221792,7.55560151478104));
#6713=CARTESIAN_POINT('Ctrl Pts',(9.36161387283237,25.4564605286804,7.7889132394161));
#6714=CARTESIAN_POINT('Ctrl Pts',(9.16841756655482,25.4681308355689,8.01542611667906));
#6715=CARTESIAN_POINT('Ctrl Pts',(8.96721873867355,25.4798011424573,8.2345272082119));
#6716=CARTESIAN_POINT('Ctrl Pts',(8.77503656446375,25.4909484487072,8.44380936251634));
#6717=CARTESIAN_POINT('Ctrl Pts',(8.57549596571777,25.5020957549571,8.64639194661431));
#6718=CARTESIAN_POINT('Ctrl Pts',(8.36908870550682,25.513243061207,8.84176478364802));
#6719=CARTESIAN_POINT('Ctrl Pts',(8.16271650354248,25.5243884740884,9.03710443663048));
#6720=CARTESIAN_POINT('Ctrl Pts',(7.94948016228641,25.5355338869698,9.22523660411167));
#6721=CARTESIAN_POINT('Ctrl Pts',(7.7299076598487,25.5466792998511,9.40568858830721));
#6722=CARTESIAN_POINT('Ctrl Pts',(7.51035953336922,25.5578234754186,9.58612053952967));
#6723=CARTESIAN_POINT('Ctrl Pts',(7.28447685633949,25.568967650986,9.75887384069105));
#6724=CARTESIAN_POINT('Ctrl Pts',(7.0528209389533,25.5801118265534,9.92351586148084));
#6725=CARTESIAN_POINT('Ctrl Pts',(6.81386970621717,25.5916069548442,10.0933427939062));
#6726=CARTESIAN_POINT('Ctrl Pts',(6.56877595494336,25.6031020831349,10.2545391062416));
#6727=CARTESIAN_POINT('Ctrl Pts',(6.31818951893479,25.6145972114257,10.4066772532265));
#6728=CARTESIAN_POINT('Ctrl Pts',(6.075240644456,25.6257419825662,10.5541784195467));
#6729=CARTESIAN_POINT('Ctrl Pts',(5.82712918612156,25.6368867537066,10.6931652624026));
#6730=CARTESIAN_POINT('Ctrl Pts',(5.57447472401569,25.6480315248471,10.8232934821758));
#6731=CARTESIAN_POINT('Ctrl Pts',(5.30990624911035,25.659701831713,10.9595579453506));
#6732=CARTESIAN_POINT('Ctrl Pts',(5.04035628965848,25.6713721385789,11.0861080739867));
#6733=CARTESIAN_POINT('Ctrl Pts',(4.7665637239795,25.6830424454448,11.2026032918801));
#6734=CARTESIAN_POINT('Ctrl Pts',(4.49277115830052,25.6947127523106,11.3190985097735));
#6735=CARTESIAN_POINT('Ctrl Pts',(4.21473629854894,25.7063830591765,11.4255386936461));
#6736=CARTESIAN_POINT('Ctrl Pts',(3.93322156640711,25.7180533660424,11.5216413049335));
#6737=CARTESIAN_POINT('Ctrl Pts',(3.66432536802045,25.7292005664975,11.6134362409698));
#6738=CARTESIAN_POINT('Ctrl Pts',(3.3921740921302,25.7403477669525,11.6958273819203));
#6739=CARTESIAN_POINT('Ctrl Pts',(3.11744366041665,25.7514949674076,11.7686020951568));
#6740=CARTESIAN_POINT('Ctrl Pts',(2.84275170720437,25.7626406065956,11.8413666156312));
#6741=CARTESIAN_POINT('Ctrl Pts',(2.56548157682794,25.7737862457837,11.9045173279686));
#6742=CARTESIAN_POINT('Ctrl Pts',(2.28632311610678,25.7849318849717,11.9578918233423));
#6743=CARTESIAN_POINT('Ctrl Pts',(2.05563452691691,25.7941423232771,12.0019989838584));
#6744=CARTESIAN_POINT('Ctrl Pts',(1.82365674195867,25.8033527615825,12.0394309579504));
#6745=CARTESIAN_POINT('Ctrl Pts',(1.59078448392773,25.8125631998879,12.0701224093086));
#6746=CARTESIAN_POINT('Origin',(0.,13.3748739960349,0.));
#6747=CARTESIAN_POINT('',(1.59078448392773,29.0623127728906,12.0701224093087));
#6748=CARTESIAN_POINT('',(1.59078448392775,28.8125580693322,12.0701224093086));
#6749=CARTESIAN_POINT('',(1.59078448392774,13.3748739960349,12.0701224093086));
#6750=CARTESIAN_POINT('',(-12.1744999986836,26.8748739959973,-0.000179033899940194));
#6751=CARTESIAN_POINT('Ctrl Pts',(-12.1744999986836,26.8748739960349,-0.000179034858391824));
#6752=CARTESIAN_POINT('Ctrl Pts',(-12.1744973429416,26.8819585649631,-0.180771412597766));
#6753=CARTESIAN_POINT('Ctrl Pts',(-12.170475924864,26.8890431338913,-0.361351713761423));
#6754=CARTESIAN_POINT('Ctrl Pts',(-12.1624403133837,26.8961277028195,-0.541752594251753));
#6755=CARTESIAN_POINT('Ctrl Pts',(-12.1497965769811,26.9072750090666,-0.825606683675804));
#6756=CARTESIAN_POINT('Ctrl Pts',(-12.127209485585,26.9184223153137,-1.109060343361));
#6757=CARTESIAN_POINT('Ctrl Pts',(-12.094727685764,26.9295696215608,-1.39140664696373));
#6758=CARTESIAN_POINT('Ctrl Pts',(-12.0622514029725,26.9407150344394,-1.67370499408291));
#6759=CARTESIAN_POINT('Ctrl Pts',(-12.0198837975782,26.9518604473179,-1.95489609573094));
#6760=CARTESIAN_POINT('Ctrl Pts',(-11.9677253505645,26.9630058601965,-2.23427844805787));
#6761=CARTESIAN_POINT('Ctrl Pts',(-11.9155726939485,26.9741500357611,-2.51362978460458));
#6762=CARTESIAN_POINT('Ctrl Pts',(-11.8536314150918,26.9852942113258,-2.79117251064493));
#6763=CARTESIAN_POINT('Ctrl Pts',(-11.7820532854202,26.9964383868904,-3.0662143808806));
#6764=CARTESIAN_POINT('Ctrl Pts',(-11.7082210150325,27.0079335151833,-3.3499178783647));
#6765=CARTESIAN_POINT('Ctrl Pts',(-11.6241351555881,27.0194286434761,-3.63096016396926));
#6766=CARTESIAN_POINT('Ctrl Pts',(-11.530018550358,27.030923771769,-3.90859597277591));
#6767=CARTESIAN_POINT('Ctrl Pts',(-11.4387705017224,27.0420685429066,-4.17776978884194));
#6768=CARTESIAN_POINT('Ctrl Pts',(-11.3380941917879,27.0532133140442,-4.44374143924996));
#6769=CARTESIAN_POINT('Ctrl Pts',(-11.2282428127532,27.0643580851818,-4.70584887006112));
#6770=CARTESIAN_POINT('Ctrl Pts',(-11.1132113520216,27.0760283920523,-4.98031607201867));
#6771=CARTESIAN_POINT('Ctrl Pts',(-10.9881188167639,27.0876986989227,-5.25054555485061));
#6772=CARTESIAN_POINT('Ctrl Pts',(-10.8533121666699,27.0993690057932,-5.51580141618739));
#6773=CARTESIAN_POINT('Ctrl Pts',(-10.7185055165759,27.1110393126637,-5.78105727752418));
#6774=CARTESIAN_POINT('Ctrl Pts',(-10.5739849114736,27.1227096195341,-6.04133922225082));
#6775=CARTESIAN_POINT('Ctrl Pts',(-10.4201526576011,27.1343799264046,-6.29594066381572));
#6776=CARTESIAN_POINT('Ctrl Pts',(-10.2732143410997,27.1455272326517,-6.53913223294777));
#6777=CARTESIAN_POINT('Ctrl Pts',(-10.1177367424751,27.1566745388988,-6.77721387905434));
#6778=CARTESIAN_POINT('Ctrl Pts',(-9.95410087098509,27.167821845146,-7.00958815482435));
#6779=CARTESIAN_POINT('Ctrl Pts',(-9.79049279302736,27.1789672580245,-7.24192296185269));
#6780=CARTESIAN_POINT('Ctrl Pts',(-9.61872936224129,27.190112670903,-7.46855211592874));
#6781=CARTESIAN_POINT('Ctrl Pts',(-9.43923450693786,27.2012580837816,-7.68890773602035));
#6782=CARTESIAN_POINT('Ctrl Pts',(-9.2597595783524,27.2124022593461,-7.9092388932142));
#6783=CARTESIAN_POINT('Ctrl Pts',(-9.07255510757798,27.2235464349107,-8.12329770037941));
#6784=CARTESIAN_POINT('Ctrl Pts',(-8.87808562861877,27.2346906104752,-8.33054895075426));
#6785=CARTESIAN_POINT('Ctrl Pts',(-8.67749191069513,27.2461857387681,-8.54432696404207));
#6786=CARTESIAN_POINT('Ctrl Pts',(-8.46916838599521,27.257680867061,-8.75086148201259));
#6787=CARTESIAN_POINT('Ctrl Pts',(-8.25366736632376,27.2691759953538,-8.94960475418229));
#6788=CARTESIAN_POINT('Ctrl Pts',(-8.04473454861487,27.2803207664914,-9.14229057960626));
#6789=CARTESIAN_POINT('Ctrl Pts',(-7.82905548443714,27.291465537629,-9.32765287209847));
#6790=CARTESIAN_POINT('Ctrl Pts',(-7.60716931389788,27.3026103087666,-9.50523146902223));
#6791=CARTESIAN_POINT('Ctrl Pts',(-7.37482002035491,27.3142806156371,-9.69118384921479));
#6792=CARTESIAN_POINT('Ctrl Pts',(-7.13566438620726,27.3259509225076,-9.86860058581242));
#6793=CARTESIAN_POINT('Ctrl Pts',(-6.89035922507428,27.3376212293782,-10.0370015442578));
#6794=CARTESIAN_POINT('Ctrl Pts',(-6.64505406394129,27.3492915362487,-10.2054025027032));
#6795=CARTESIAN_POINT('Ctrl Pts',(-6.39359965738751,27.3609618431192,-10.3647875003511));
#6796=CARTESIAN_POINT('Ctrl Pts',(-6.13668738798872,27.3726321499897,-10.5147286295035));
#6797=CARTESIAN_POINT('Ctrl Pts',(-5.89128854994562,27.3837794562368,-10.6579502006452));
#6798=CARTESIAN_POINT('Ctrl Pts',(-5.64083698966155,27.3949267624839,-10.7925985197516));
#6799=CARTESIAN_POINT('Ctrl Pts',(-5.38595316180751,27.4060740687311,-10.9183313188791));
#6800=CARTESIAN_POINT('Ctrl Pts',(-5.13111262593913,27.4172194816096,-11.0440427623067));
#6801=CARTESIAN_POINT('Ctrl Pts',(-4.87184156463934,27.4283648944882,-11.1608415910916));
#6802=CARTESIAN_POINT('Ctrl Pts',(-4.60878396953977,27.4395103073668,-11.2684320369834));
#6803=CARTESIAN_POINT('Ctrl Pts',(-4.3457555779199,27.4506544829314,-11.3760105386643));
#6804=CARTESIAN_POINT('Ctrl Pts',(-4.07894173873217,27.461798658496,-11.4743825978158));
#6805=CARTESIAN_POINT('Ctrl Pts',(-3.80900646198326,27.4729428340606,-11.5633005678556));
#6806=CARTESIAN_POINT('Ctrl Pts',(-3.53057037498807,27.4844379623534,-11.6550187454114));
#6807=CARTESIAN_POINT('Ctrl Pts',(-3.24881334259174,27.4959330906463,-11.7366776258322));
#6808=CARTESIAN_POINT('Ctrl Pts',(-2.96448245205888,27.5074282189391,-11.8080605537673));
#6809=CARTESIAN_POINT('Ctrl Pts',(-2.68881761199677,27.5185729900768,-11.877267819202));
#6810=CARTESIAN_POINT('Ctrl Pts',(-2.41073375712401,27.5297177612144,-11.9368161849391));
#6811=CARTESIAN_POINT('Ctrl Pts',(-2.13092449458315,27.540862532352,-11.9865596001682));
#6812=CARTESIAN_POINT('Ctrl Pts',(-1.83792072458815,27.5525328392224,-12.0386486842186));
#6813=CARTESIAN_POINT('Ctrl Pts',(-1.5430252199813,27.5642031460929,-12.0799857998834));
#6814=CARTESIAN_POINT('Ctrl Pts',(-1.24704447022982,27.5758734529634,-12.1104636715226));
#6815=CARTESIAN_POINT('Ctrl Pts',(-0.951063720478334,27.5875437598338,-12.1409415431618));
#6816=CARTESIAN_POINT('Ctrl Pts',(-0.653998060217559,27.5992140667043,-12.1605601451418));
#6817=CARTESIAN_POINT('Ctrl Pts',(-0.356659339898103,27.6108843735748,-12.1692746030839));
#6818=CARTESIAN_POINT('Ctrl Pts',(-0.0726457478549768,27.6220316798219,
-12.177598525714));
#6819=CARTESIAN_POINT('Ctrl Pts',(0.211701791907702,27.633178986069,-12.175976638602));
#6820=CARTESIAN_POINT('Ctrl Pts',(0.495674690478524,27.6443262923161,-12.1644053225474));
#6821=CARTESIAN_POINT('Ctrl Pts',(0.779599356289084,27.6554717051947,-12.1528359718793));
#6822=CARTESIAN_POINT('Ctrl Pts',(1.06314924152558,27.6666171180733,-12.1313205770283));
#6823=CARTESIAN_POINT('Ctrl Pts',(1.34561734240108,27.6777625309519,-12.0999076119543));
#6824=CARTESIAN_POINT('Ctrl Pts',(1.6280540849292,27.6889067065165,-12.0684981342074));
#6825=CARTESIAN_POINT('Ctrl Pts',(1.9094090178618,27.7000508820811,-12.02719330981));
#6826=CARTESIAN_POINT('Ctrl Pts',(2.18898058826488,27.7111950576458,-11.9760934462871));
#6827=CARTESIAN_POINT('Ctrl Pts',(2.47735643537739,27.7226901859386,-11.923384344251));
#6828=CARTESIAN_POINT('Ctrl Pts',(2.76383448278513,27.7341853142314,-11.8602533185206));
#6829=CARTESIAN_POINT('Ctrl Pts',(3.04765506100921,27.7456804425243,-11.7868676449303));
#6830=CARTESIAN_POINT('Ctrl Pts',(3.32282514244449,27.7568252136619,-11.7157186750269));
#6831=CARTESIAN_POINT('Ctrl Pts',(3.59549707841157,27.7679699847995,-11.6349309684199));
#6832=CARTESIAN_POINT('Ctrl Pts',(3.86499194570396,27.7791147559371,-11.5447082037461));
#6833=CARTESIAN_POINT('Ctrl Pts',(4.14719494139433,27.7907850628076,-11.4502309518185));
#6834=CARTESIAN_POINT('Ctrl Pts',(4.42591372566347,27.8024553696781,-11.3454075047072));
#6835=CARTESIAN_POINT('Ctrl Pts',(4.70038881294249,27.8141256765485,-11.2305296071541));
#6836=CARTESIAN_POINT('Ctrl Pts',(4.97486390022151,27.825795983419,-11.115651709601));
#6837=CARTESIAN_POINT('Ctrl Pts',(5.24509498441225,27.8374662902895,-10.9907194992353));
#6838=CARTESIAN_POINT('Ctrl Pts',(5.5103477343262,27.8491365971599,-10.8560820785773));
#6839=CARTESIAN_POINT('Ctrl Pts',(5.76371327723781,27.860283903407,-10.7274783857133));
#6840=CARTESIAN_POINT('Ctrl Pts',(6.01261255303692,27.8714312096541,-10.5899818243253));
#6841=CARTESIAN_POINT('Ctrl Pts',(6.2564216431686,27.8825785159013,-10.4439283065756));
#6842=CARTESIAN_POINT('Ctrl Pts',(6.50018932235742,27.8937239287798,-10.2978995959973));
#6843=CARTESIAN_POINT('Ctrl Pts',(6.73886831324427,27.9048693416584,-10.1433169677941));
#6844=CARTESIAN_POINT('Ctrl Pts',(6.97186101791719,27.916014754537,-9.98056131672196));
#6845=CARTESIAN_POINT('Ctrl Pts',(7.20482785678025,27.9271589301016,-9.81782373405559));
#6846=CARTESIAN_POINT('Ctrl Pts',(7.43210945134621,27.9383031056662,-9.64691509303569));
#6847=CARTESIAN_POINT('Ctrl Pts',(7.6531377944767,27.9494472812308,-9.46825919315438));
#6848=CARTESIAN_POINT('Ctrl Pts',(7.88112676915815,27.9609424095236,-9.28397705604092));
#6849=CARTESIAN_POINT('Ctrl Pts',(8.10246201817212,27.9724375378165,-9.09145197819303));
#6850=CARTESIAN_POINT('Ctrl Pts',(8.31655655151377,27.9839326661093,-8.89119437283166));
#6851=CARTESIAN_POINT('Ctrl Pts',(8.52412575084056,27.9950774372469,-8.69704036919988));
#6852=CARTESIAN_POINT('Ctrl Pts',(8.7248888707482,28.0062222083845,-8.49561840443982));
#6853=CARTESIAN_POINT('Ctrl Pts',(8.91834724194499,28.0173669795222,-8.28743221523363));
#6854=CARTESIAN_POINT('Ctrl Pts',(9.12092821293592,28.0290372863926,-8.06942893062317));
#6855=CARTESIAN_POINT('Ctrl Pts',(9.31549872612246,28.0407075932631,-7.84400836552933));
#6856=CARTESIAN_POINT('Ctrl Pts',(9.50153151667196,28.0523779001336,-7.61179013686593));
#6857=CARTESIAN_POINT('Ctrl Pts',(9.68756430722147,28.0640482070041,-7.37957190820253));
#6858=CARTESIAN_POINT('Ctrl Pts',(9.86505917222155,28.0757185138745,-7.14055628329797));
#6859=CARTESIAN_POINT('Ctrl Pts',(10.0335383821488,28.087388820745,-6.89540120543738));
#6860=CARTESIAN_POINT('Ctrl Pts',(10.194467256614,28.0985361269921,-6.66123266460331));
#6861=CARTESIAN_POINT('Ctrl Pts',(10.3472188441184,28.1096834332392,-6.42139291309911));
#6862=CARTESIAN_POINT('Ctrl Pts',(10.4914060523786,28.1208307394863,-6.1764754750677));
#6863=CARTESIAN_POINT('Ctrl Pts',(10.6355687704599,28.1319761523649,-5.93159963623197));
#6864=CARTESIAN_POINT('Ctrl Pts',(10.7711698782457,28.1431215652434,-5.68164806252201));
#6865=CARTESIAN_POINT('Ctrl Pts',(10.8978669207609,28.154266978122,-5.42724118013789));
#6866=CARTESIAN_POINT('Ctrl Pts',(11.0245498979363,28.1654111536866,-5.1728625408699));
#6867=CARTESIAN_POINT('Ctrl Pts',(11.1423306648156,28.1765553292512,-4.91402981929681));
#6868=CARTESIAN_POINT('Ctrl Pts',(11.250913280774,28.1876995048158,-4.65138695428623));
#6869=CARTESIAN_POINT('Ctrl Pts',(11.3629153838978,28.1991946331086,-4.38047293188917));
#6870=CARTESIAN_POINT('Ctrl Pts',(11.4651304890387,28.2106897614015,-4.10550516952863));
#6871=CARTESIAN_POINT('Ctrl Pts',(11.5572874357625,28.2221848896944,-3.82721274260596));
#6872=CARTESIAN_POINT('Ctrl Pts',(11.6466355538357,28.2333296608319,-3.55740232132468));
#6873=CARTESIAN_POINT('Ctrl Pts',(11.7265294669145,28.2444744319695,-3.28446716262288));
#6874=CARTESIAN_POINT('Ctrl Pts',(11.7967723708194,28.2556192031071,-3.00908821423886));
#6875=CARTESIAN_POINT('Ctrl Pts',(11.8703276043836,28.2672895099776,-2.72072367147365));
#6876=CARTESIAN_POINT('Ctrl Pts',(11.9332996556248,28.2789598168481,-2.42967962578353));
#6877=CARTESIAN_POINT('Ctrl Pts',(11.9855220652797,28.2906301237186,-2.13675245938659));
#6878=CARTESIAN_POINT('Ctrl Pts',(12.0377444749345,28.3023004305891,-1.84382529298966));
#6879=CARTESIAN_POINT('Ctrl Pts',(12.0792171927608,28.3139707374596,-1.54901533771966));
#6880=CARTESIAN_POINT('Ctrl Pts',(12.1098355954862,28.3256410443301,-1.25312892405157));
#6881=CARTESIAN_POINT('Ctrl Pts',(12.1390818454577,28.3367883505772,-0.970502554057997));
#6882=CARTESIAN_POINT('Ctrl Pts',(12.1584339953508,28.3479356568243,-0.686809677550053));
#6883=CARTESIAN_POINT('Ctrl Pts',(12.1678361799058,28.3590829630714,-0.40275668706502));
#6884=CARTESIAN_POINT('Ctrl Pts',(12.177236767501,28.37022837595,-0.118751942944197));
#6885=CARTESIAN_POINT('Ctrl Pts',(12.1766907550221,28.3813737888286,0.165612526537045));
#6886=CARTESIAN_POINT('Ctrl Pts',(12.1661943454187,28.3925192017072,0.449628067964166));
#6887=CARTESIAN_POINT('Ctrl Pts',(12.1556991010799,28.4036633772718,0.733612079254089));
#6888=CARTESIAN_POINT('Ctrl Pts',(12.1352556752733,28.4148075528364,1.0172469733435));
#6889=CARTESIAN_POINT('Ctrl Pts',(12.104912365353,28.425951728401,1.29982571028703));
#6890=CARTESIAN_POINT('Ctrl Pts',(12.07361348296,28.4374468566938,1.59130342572396));
#6891=CARTESIAN_POINT('Ctrl Pts',(12.0317810995415,28.4489419849867,1.88165708895882));
#6892=CARTESIAN_POINT('Ctrl Pts',(11.9795260125188,28.4604371132795,2.1701167630765));
#6893=CARTESIAN_POINT('Ctrl Pts',(11.9288635952924,28.4715818844171,2.44978454655556));
#6894=CARTESIAN_POINT('Ctrl Pts',(11.8684044580646,28.4827266555547,2.727671809539));
#6895=CARTESIAN_POINT('Ctrl Pts',(11.7983016566862,28.4938714266923,3.00308645693653));
#6896=CARTESIAN_POINT('Ctrl Pts',(11.7248931322342,28.5055417335628,3.29148838211453));
#6897=CARTESIAN_POINT('Ctrl Pts',(11.6409096368336,28.5172120404333,3.57717857842725));
#6898=CARTESIAN_POINT('Ctrl Pts',(11.5465861114499,28.5288823473038,3.85937811322915));
#6899=CARTESIAN_POINT('Ctrl Pts',(11.4522625860663,28.5405526541742,4.14157764803105));
#6900=CARTESIAN_POINT('Ctrl Pts',(11.3475991453805,28.5522229610447,4.42028620590779));
#6901=CARTESIAN_POINT('Ctrl Pts',(11.2328897869991,28.5638932679152,4.6947457101671));
#6902=CARTESIAN_POINT('Ctrl Pts',(11.1233210874371,28.5750405741623,4.95690541002459));
#6903=CARTESIAN_POINT('Ctrl Pts',(11.0045543630941,28.5861878804094,5.21526682176328));
#6904=CARTESIAN_POINT('Ctrl Pts',(10.8768785996751,28.5973351866565,5.46918295341547));
#6905=CARTESIAN_POINT('Ctrl Pts',(10.7492245219682,28.6084805995351,5.72305595744509));
#6906=CARTESIAN_POINT('Ctrl Pts',(10.6126645460732,28.6196260124137,5.97248495058034));
#6907=CARTESIAN_POINT('Ctrl Pts',(10.467534458856,28.6307714252922,6.21684587251955));
#6908=CARTESIAN_POINT('Ctrl Pts',(10.3224204833328,28.6419156008568,6.46117966660059));
#6909=CARTESIAN_POINT('Ctrl Pts',(10.1687384324912,28.6530597764214,6.70044628368926));
#6910=CARTESIAN_POINT('Ctrl Pts',(10.0068690633192,28.664203951986,6.93404800961067));
#6911=CARTESIAN_POINT('Ctrl Pts',(9.83990209886954,28.6756990802789,7.17500632845005));
#6912=CARTESIAN_POINT('Ctrl Pts',(9.66422395039496,28.6871942085718,7.40993692714886));
#6913=CARTESIAN_POINT('Ctrl Pts',(9.48030035284617,28.6986893368646,7.63821677290091));
#6914=CARTESIAN_POINT('Ctrl Pts',(9.30198251686694,28.7098341080022,7.85953893403023));
#6915=CARTESIAN_POINT('Ctrl Pts',(9.11591458607458,28.7209788791398,8.0746095348416));
#6916=CARTESIAN_POINT('Ctrl Pts',(8.92256215039984,28.7321236502774,8.28289411511775));
#6917=CARTESIAN_POINT('Ctrl Pts',(8.72009211035867,28.7437939571479,8.50100043046518));
#6918=CARTESIAN_POINT('Ctrl Pts',(8.50963424411612,28.7554642640184,8.71166509837527));
#6919=CARTESIAN_POINT('Ctrl Pts',(8.29176759747592,28.7671345708889,8.91431659519946));
#6920=CARTESIAN_POINT('Ctrl Pts',(8.07390095083574,28.7788048777594,9.11696809202363));
#6921=CARTESIAN_POINT('Ctrl Pts',(7.84862577543433,28.7904751846298,9.31160619568754));
#6922=CARTESIAN_POINT('Ctrl Pts',(7.61656299213793,28.8021454915003,9.49770595653471));
#6923=CARTESIAN_POINT('Ctrl Pts',(7.39490001937539,28.8132927977474,9.67546572324015));
#6924=CARTESIAN_POINT('Ctrl Pts',(7.1669782326602,28.8244401039945,9.84548870117948));
#6925=CARTESIAN_POINT('Ctrl Pts',(6.93336099330262,28.8355874102417,10.0073450818161));
#6926=CARTESIAN_POINT('Ctrl Pts',(6.69978343380331,28.8467328231202,10.1691739711672));
#6927=CARTESIAN_POINT('Ctrl Pts',(6.4605125722004,28.8578782359988,10.3228388806969));
#6928=CARTESIAN_POINT('Ctrl Pts',(6.21614189045049,28.8690236488774,10.4679525336995));
#6929=CARTESIAN_POINT('Ctrl Pts',(5.97179833764248,28.880167824442,10.6130500768324));
#6930=CARTESIAN_POINT('Ctrl Pts',(5.72235632451495,28.8913120000066,10.7495981229213));
#6931=CARTESIAN_POINT('Ctrl Pts',(5.46843621193559,28.9024561755712,10.8772540489772));
#6932=CARTESIAN_POINT('Ctrl Pts',(5.20651963916487,28.913951303864,11.0089301194815));
#6933=CARTESIAN_POINT('Ctrl Pts',(4.93983860834559,28.9254464321569,11.1311447906857));
#6934=CARTESIAN_POINT('Ctrl Pts',(4.66910021250546,28.9369415604497,11.2435738737993));
#6935=CARTESIAN_POINT('Ctrl Pts',(4.40661358487263,28.9480863315873,11.3525762588609));
#6936=CARTESIAN_POINT('Ctrl Pts',(4.14031351438245,28.9592311027249,11.4523806207873));
#6937=CARTESIAN_POINT('Ctrl Pts',(3.87086458095965,28.9703758738625,11.5427404738161));
#6938=CARTESIAN_POINT('Ctrl Pts',(3.58870968516636,28.982046180733,11.6373612785503));
#6939=CARTESIAN_POINT('Ctrl Pts',(3.30310211058205,28.9937164876035,11.7216253225375));
#6940=CARTESIAN_POINT('Ctrl Pts',(3.01482379511558,29.005386794474,11.7953078694202));
#6941=CARTESIAN_POINT('Ctrl Pts',(2.72654547964909,29.0170571013444,11.8689904163028));
#6942=CARTESIAN_POINT('Ctrl Pts',(2.43559675052545,29.0287274082149,11.9320913915042));
#6943=CARTESIAN_POINT('Ctrl Pts',(2.14277402700613,29.0403977150854,11.9844469926312));
#6944=CARTESIAN_POINT('Ctrl Pts',(1.95948187699894,29.0477027343538,12.0172189393578));
#6945=CARTESIAN_POINT('Ctrl Pts',(1.77541980190147,29.0550077536222,12.0457883562595));
#6946=CARTESIAN_POINT('Ctrl Pts',(1.59078448392773,29.0623127728906,12.0701224093086));
#6947=CARTESIAN_POINT('Ctrl Pts',(1.59078448392775,26.0623070005467,12.0701224093086));
#6948=CARTESIAN_POINT('Ctrl Pts',(1.30899806788644,26.0734518121,12.1072605130676));
#6949=CARTESIAN_POINT('Ctrl Pts',(1.02591071152476,26.0845966236534,12.1345265044841));
#6950=CARTESIAN_POINT('Ctrl Pts',(0.742228150596408,26.0957414352068,12.1518536702209));
#6951=CARTESIAN_POINT('Ctrl Pts',(0.458543333616702,26.1068863353918,12.1691809737561));
#6952=CARTESIAN_POINT('Ctrl Pts',(0.174263569054537,26.1180312355769,12.1765692799692));
#6953=CARTESIAN_POINT('Ctrl Pts',(-0.109902562578879,26.129176135762,12.1740039295516));
#6954=CARTESIAN_POINT('Ctrl Pts',(-0.394127988996509,26.1403233614686,12.1714380438419));
#6955=CARTESIAN_POINT('Ctrl Pts',(-0.67823946826702,26.1514705871751,12.1589143533114));
#6956=CARTESIAN_POINT('Ctrl Pts',(-0.961529148741264,26.1626178128817,12.1364703248564));
#6957=CARTESIAN_POINT('Ctrl Pts',(-1.1203906032984,26.1688688859425,12.123884299836));
#6958=CARTESIAN_POINT('Ctrl Pts',(-1.27899367264829,26.1751199590034,12.1081795891686));
#6959=CARTESIAN_POINT('Ctrl Pts',(-1.43721416924489,26.1813710320642,12.089369945606));
#6960=CARTESIAN_POINT('Ctrl Pts',(-1.71936290002593,26.1925183383113,12.0558274073648));
#6961=CARTESIAN_POINT('Ctrl Pts',(-2.00037900433126,26.2036656445584,12.0123981199221));
#6962=CARTESIAN_POINT('Ctrl Pts',(-2.27956106827265,26.2148129508055,11.9591827306892));
#6963=CARTESIAN_POINT('Ctrl Pts',(-2.55869571317684,26.2259583636841,11.9059763800833));
#6964=CARTESIAN_POINT('Ctrl Pts',(-2.83599667771954,26.2371037765627,11.8429872961323));
#6965=CARTESIAN_POINT('Ctrl Pts',(-3.11077177834478,26.2482491894413,11.7703674196286));
#6966=CARTESIAN_POINT('Ctrl Pts',(-3.38551637466469,26.2593933650059,11.6977556050594));
#6967=CARTESIAN_POINT('Ctrl Pts',(-3.6577354091752,26.2705375405705,11.6155152010359));
#6968=CARTESIAN_POINT('Ctrl Pts',(-3.92674971414901,26.2816817161351,11.5238486163447));
#6969=CARTESIAN_POINT('Ctrl Pts',(-4.20423582609698,26.2931768444279,11.4292952646783));
#6970=CARTESIAN_POINT('Ctrl Pts',(-4.47831180682542,26.3046719727208,11.3247124991569));
#6971=CARTESIAN_POINT('Ctrl Pts',(-4.74825085465416,26.3161671010137,11.2103775168937));
#6972=CARTESIAN_POINT('Ctrl Pts',(-5.0099624974065,26.3273118721513,11.0995273221078));
#6973=CARTESIAN_POINT('Ctrl Pts',(-5.26778539315454,26.338456643289,10.9795106872953));
#6974=CARTESIAN_POINT('Ctrl Pts',(-5.52107796274178,26.3496014144266,10.8506289393439));
#6975=CARTESIAN_POINT('Ctrl Pts',(-5.78631463548921,26.3612717212971,10.7156697257349));
#6976=CARTESIAN_POINT('Ctrl Pts',(-6.04658315982574,26.3729420281675,10.5709893503964));
#6977=CARTESIAN_POINT('Ctrl Pts',(-6.30117522427093,26.384612335038,10.4169880984397));
#6978=CARTESIAN_POINT('Ctrl Pts',(-6.5557672887161,26.3962826419084,10.262986846483));
#6979=CARTESIAN_POINT('Ctrl Pts',(-6.80468261074529,26.4079529487789,10.0996648990647));
#6980=CARTESIAN_POINT('Ctrl Pts',(-7.04724619648092,26.4196232556493,9.92747557519963));
#6981=CARTESIAN_POINT('Ctrl Pts',(-7.27893938198356,26.4307705618965,9.76300285422281));
#6982=CARTESIAN_POINT('Ctrl Pts',(-7.50490681694821,26.4419178681436,9.59039094205251));
#6983=CARTESIAN_POINT('Ctrl Pts',(-7.72458077897762,26.4530651743908,9.41006387008343));
#6984=CARTESIAN_POINT('Ctrl Pts',(-7.9442174294129,26.4642105872694,9.22976742664427));
#6985=CARTESIAN_POINT('Ctrl Pts',(-8.15756253496308,26.4753560001481,9.04175860884122));
#6986=CARTESIAN_POINT('Ctrl Pts',(-8.36408102412932,26.4865014130267,8.84650206984658));
#6987=CARTESIAN_POINT('Ctrl Pts',(-8.57057658653295,26.4976455885913,8.65126720736302));
#6988=CARTESIAN_POINT('Ctrl Pts',(-8.77024685209962,26.5087897641558,8.44878641357831));
#6989=CARTESIAN_POINT('Ctrl Pts',(-8.96259232915518,26.5199339397204,8.23956242717833));
#6990=CARTESIAN_POINT('Ctrl Pts',(-9.16099515603928,26.5314290680132,8.0237495524013));
#6991=CARTESIAN_POINT('Ctrl Pts',(-9.35160416569127,26.542924196306,7.80076210097047));
#6992=CARTESIAN_POINT('Ctrl Pts',(-9.53391383017232,26.5544193245989,7.5711912754103));
#6993=CARTESIAN_POINT('Ctrl Pts',(-9.71066692374877,26.5655640957365,7.34861748192455));
#6994=CARTESIAN_POINT('Ctrl Pts',(-9.87961891449672,26.5767088668741,7.11985589637044));
#6995=CARTESIAN_POINT('Ctrl Pts',(-10.0403506524587,26.5878536380117,6.88547812614872));
#6996=CARTESIAN_POINT('Ctrl Pts',(-10.2086617539316,26.5995239448822,6.64004818700301));
#6997=CARTESIAN_POINT('Ctrl Pts',(-10.3679585107329,26.6111942517526,6.38845991414234));
#6998=CARTESIAN_POINT('Ctrl Pts',(-10.5178105333709,26.622864558623,6.13140374091549));
#6999=CARTESIAN_POINT('Ctrl Pts',(-10.6676625560089,26.6345348654935,5.87434756768864));
#7000=CARTESIAN_POINT('Ctrl Pts',(-10.8080696830999,26.6462051723639,5.61182378836291));
#7001=CARTESIAN_POINT('Ctrl Pts',(-10.9386561591369,26.6578754792344,5.34455345956773));
#7002=CARTESIAN_POINT('Ctrl Pts',(-11.0629966322907,26.6689875907038,5.09006677648294));
#7003=CARTESIAN_POINT('Ctrl Pts',(-11.1784731441786,26.6800997021732,4.83119636045063));
#7004=CARTESIAN_POINT('Ctrl Pts',(-11.284791078264,26.6912118136426,4.56858189922576));
#7005=CARTESIAN_POINT('Ctrl Pts',(-11.3910898863404,26.7023219261046,4.30601468089191));
#7006=CARTESIAN_POINT('Ctrl Pts',(-11.4882333044429,26.7134320385665,4.03970501227435));
#7007=CARTESIAN_POINT('Ctrl Pts',(-11.5759747961597,26.7245421510285,3.77031268844835));
#7008=CARTESIAN_POINT('Ctrl Pts',(-11.6637063953042,26.7356510108608,3.50095073774466));
#7009=CARTESIAN_POINT('Ctrl Pts',(-11.742038101081,26.7467598706931,3.22850708261955));
#7010=CARTESIAN_POINT('Ctrl Pts',(-11.8107728310722,26.7578687305254,2.95365796645564));
#7011=CARTESIAN_POINT('Ctrl Pts',(-11.8795114701164,26.7689782221362,2.67879321918694));
#7012=CARTESIAN_POINT('Ctrl Pts',(-11.938651974578,26.780087713747,2.40152299895952));
#7013=CARTESIAN_POINT('Ctrl Pts',(-11.9880477658973,26.7911972053578,2.12253645729935));
#7014=CARTESIAN_POINT('Ctrl Pts',(-12.0374432737353,26.8023066332115,1.84355151673624));
#7015=CARTESIAN_POINT('Ctrl Pts',(-12.0770941352764,26.8134160610651,1.56285054084612));
#7016=CARTESIAN_POINT('Ctrl Pts',(-12.1069051509043,26.8245254889188,1.28113149871751));
#7017=CARTESIAN_POINT('Ctrl Pts',(-12.136721994767,26.8356370887331,0.9993573788041));
#7018=CARTESIAN_POINT('Ctrl Pts',(-12.1566951200387,26.8467486885475,0.716565063644844));
#7019=CARTESIAN_POINT('Ctrl Pts',(-12.1667811943891,26.8578602883618,0.433457746337774));
#7020=CARTESIAN_POINT('Ctrl Pts',(-12.1719290135767,26.8635315242403,0.288962947910597));
#7021=CARTESIAN_POINT('Ctrl Pts',(-12.1745021246081,26.8692027601188,0.144386144645321));
#7022=CARTESIAN_POINT('Ctrl Pts',(-12.1744999986836,26.8748739959973,-0.000179033899942618));
#7023=CARTESIAN_POINT('',(-12.174499996235,26.6251260039329,-0.000302777009382115));
#7024=CARTESIAN_POINT('Ctrl Pts',(1.59078448392773,25.8125631998879,12.0701224093086));
#7025=CARTESIAN_POINT('Ctrl Pts',(1.30903389514245,25.8237068476434,12.1072557912064));
#7026=CARTESIAN_POINT('Ctrl Pts',(1.02597395944363,25.8348504953989,12.1345207225652));
#7027=CARTESIAN_POINT('Ctrl Pts',(0.742310031349682,25.8459941431544,12.1518486687153));
#7028=CARTESIAN_POINT('Ctrl Pts',(0.458617504427568,25.8571389144058,12.1691783618586));
#7029=CARTESIAN_POINT('Ctrl Pts',(0.174321129593775,25.8682836856572,12.1765690496002));
#7030=CARTESIAN_POINT('Ctrl Pts',(-0.109870438808507,25.8794284569086,12.1740042195112));
#7031=CARTESIAN_POINT('Ctrl Pts',(-0.394068654609052,25.8905734888424,12.1714393294294));
#7032=CARTESIAN_POINT('Ctrl Pts',(-0.678161792355716,25.9017185207762,12.1589184614899));
#7033=CARTESIAN_POINT('Ctrl Pts',(-0.961442061063879,25.91286355271,12.1364772241873));
#7034=CARTESIAN_POINT('Ctrl Pts',(-1.24477735406477,25.9240107494521,12.1140316279041));
#7035=CARTESIAN_POINT('Ctrl Pts',(-1.52729919663202,25.9351579461943,12.0816618336698));
#7036=CARTESIAN_POINT('Ctrl Pts',(-1.80830429338909,25.9463051429365,12.0394553793978));
#7037=CARTESIAN_POINT('Ctrl Pts',(-1.89233667555125,25.9496386251668,12.0268338684856));
#7038=CARTESIAN_POINT('Ctrl Pts',(-1.97623346896302,25.9529721073972,12.0133330526306));
#7039=CARTESIAN_POINT('Ctrl Pts',(-2.05997600562754,25.9563055896275,11.9989561673605));
#7040=CARTESIAN_POINT('Ctrl Pts',(-2.34001460716402,25.9674528958737,11.9508792520215));
#7041=CARTESIAN_POINT('Ctrl Pts',(-2.61841122728923,25.9786002021198,11.8929873201509));
#7042=CARTESIAN_POINT('Ctrl Pts',(-2.89447058977853,25.989747508366,11.8254171281569));
#7043=CARTESIAN_POINT('Ctrl Pts',(-3.17048306361892,26.0008929212436,11.7578584129518));
#7044=CARTESIAN_POINT('Ctrl Pts',(-3.44415881339921,26.0120383341212,11.6806247829667));
#7045=CARTESIAN_POINT('Ctrl Pts',(-3.71481443132733,26.0231837469987,11.5939037425193));
#7046=CARTESIAN_POINT('Ctrl Pts',(-3.98544000227735,26.0343279225623,11.5071923294544));
#7047=CARTESIAN_POINT('Ctrl Pts',(-4.25304585691818,26.0454720981259,11.4109956904718));
#7048=CARTESIAN_POINT('Ctrl Pts',(-4.51696419368029,26.0566162736895,11.30555105791));
#7049=CARTESIAN_POINT('Ctrl Pts',(-4.78919385506674,26.0681114019831,11.1967857596382));
#7050=CARTESIAN_POINT('Ctrl Pts',(-5.05749970102558,26.0796065302767,11.0781806539634));
#7051=CARTESIAN_POINT('Ctrl Pts',(-5.32117022412959,26.0911016585703,10.9500501229829));
#7052=CARTESIAN_POINT('Ctrl Pts',(-5.57680439892114,26.1022464297069,10.8258248505966));
#7053=CARTESIAN_POINT('Ctrl Pts',(-5.828081373454,26.1133912008435,10.6926463228308));
#7054=CARTESIAN_POINT('Ctrl Pts',(-6.07437599581028,26.12453597198,10.550848615705));
#7055=CARTESIAN_POINT('Ctrl Pts',(-6.33228473064399,26.1362062788521,10.4023643861377));
#7056=CARTESIAN_POINT('Ctrl Pts',(-6.58472964219707,26.1478765857242,10.2444286953485));
#7057=CARTESIAN_POINT('Ctrl Pts',(-6.83102404874258,26.1595468925963,10.0774778935754));
#7058=CARTESIAN_POINT('Ctrl Pts',(-7.07731845528811,26.1712171994684,9.91052709180227));
#7059=CARTESIAN_POINT('Ctrl Pts',(-7.31746208403958,26.1828875063405,9.73456137455852));
#7060=CARTESIAN_POINT('Ctrl Pts',(-7.55080426673173,26.1945578132126,9.55006833355165));
#7061=CARTESIAN_POINT('Ctrl Pts',(-7.77368930304789,26.2057051194604,9.37384328212515));
#7062=CARTESIAN_POINT('Ctrl Pts',(-7.99043566959423,26.2168524257083,9.18978577348594));
#7063=CARTESIAN_POINT('Ctrl Pts',(-8.20049831293366,26.2279997319561,8.99834860791536));
#7064=CARTESIAN_POINT('Ctrl Pts',(-8.41052527716152,26.2391451448355,8.80694395792146));
#7065=CARTESIAN_POINT('Ctrl Pts',(-8.61387058758587,26.2502905577149,8.60816233308373));
#7066=CARTESIAN_POINT('Ctrl Pts',(-8.81002389705792,26.2614359705943,8.40249541405816));
#7067=CARTESIAN_POINT('Ctrl Pts',(-9.00615543046492,26.2725801461596,8.19685132725613));
#7068=CARTESIAN_POINT('Ctrl Pts',(-9.19509637319099,26.283724321725,7.98432366558186));
#7069=CARTESIAN_POINT('Ctrl Pts',(-9.37637387833569,26.2948684972904,7.76544030584642));
#7070=CARTESIAN_POINT('Ctrl Pts',(-9.56336018036558,26.3063636255827,7.53966386447199));
#7071=CARTESIAN_POINT('Ctrl Pts',(-9.74219235219411,26.3178587538749,7.30712515292804));
#7072=CARTESIAN_POINT('Ctrl Pts',(-9.91239608982264,26.3293538821672,7.06844070559192));
#7073=CARTESIAN_POINT('Ctrl Pts',(-10.0774122300974,26.3404986533055,6.83703106211519));
#7074=CARTESIAN_POINT('Ctrl Pts',(-10.2343179534282,26.3516434244438,6.59984499127896));
#7075=CARTESIAN_POINT('Ctrl Pts',(-10.3827242058869,26.3627881955821,6.35747499519189));
#7076=CARTESIAN_POINT('Ctrl Pts',(-10.5381286090834,26.3744585024514,6.10367595390744));
#7077=CARTESIAN_POINT('Ctrl Pts',(-10.6842124964244,26.3861288093207,5.84419259488536));
#7078=CARTESIAN_POINT('Ctrl Pts',(-10.8205817294359,26.3977991161899,5.57973666821271));
#7079=CARTESIAN_POINT('Ctrl Pts',(-10.9569509624474,26.4094694230592,5.31528074154007));
#7080=CARTESIAN_POINT('Ctrl Pts',(-11.0836053951668,26.4211397299285,5.04585254943003));
#7081=CARTESIAN_POINT('Ctrl Pts',(-11.2002070324854,26.4328100367977,4.77219160129437));
#7082=CARTESIAN_POINT('Ctrl Pts',(-11.311144830923,26.4439134670834,4.51182353269197));
#7083=CARTESIAN_POINT('Ctrl Pts',(-11.4130186487047,26.4550168973691,4.24754059388121));
#7084=CARTESIAN_POINT('Ctrl Pts',(-11.5055675162661,26.4661203276549,3.97999577620921));
#7085=CARTESIAN_POINT('Ctrl Pts',(-11.5980993129953,26.4772217098896,3.71250030773821));
#7086=CARTESIAN_POINT('Ctrl Pts',(-11.6813095047598,26.4883230921244,3.44174441751769));
#7087=CARTESIAN_POINT('Ctrl Pts',(-11.7549861724547,26.4994244743592,3.16839870208905));
#7088=CARTESIAN_POINT('Ctrl Pts',(-11.8286604607754,26.5105254980769,2.89506181430902));
#7089=CARTESIAN_POINT('Ctrl Pts',(-11.8928017662328,26.5216265217947,2.61913552911646));
#7090=CARTESIAN_POINT('Ctrl Pts',(-11.9472483674234,26.5327275455124,2.34130448619971));
#7091=CARTESIAN_POINT('Ctrl Pts',(-12.0016914005901,26.5438278417519,2.06349165025601));
#7092=CARTESIAN_POINT('Ctrl Pts',(-12.0464409474768,26.5549281379914,1.78377457205652));
#7093=CARTESIAN_POINT('Ctrl Pts',(-12.0813864435219,26.5660284342308,1.50284791389073));
#7094=CARTESIAN_POINT('Ctrl Pts',(-12.1163370539098,26.5771303550208,1.22188014154935));
#7095=CARTESIAN_POINT('Ctrl Pts',(-12.1414807111354,26.5882322758107,0.939702704299309));
#7096=CARTESIAN_POINT('Ctrl Pts',(-12.1567585846212,26.5993341966006,0.657016716103665));
#7097=CARTESIAN_POINT('Ctrl Pts',(-12.1685896895518,26.6079314657114,0.438106172572895));
#7098=CARTESIAN_POINT('Ctrl Pts',(-12.1745054475292,26.6165287348221,0.218890818353648));
#7099=CARTESIAN_POINT('Ctrl Pts',(-12.174499996235,26.6251260039329,-0.000302777009381836));
#7100=CARTESIAN_POINT('Ctrl Pts',(-12.174499996235,26.6251260039651,-0.000302777830488094));
#7101=CARTESIAN_POINT('Ctrl Pts',(-12.1744924727439,26.6369913152146,-0.302817471666667));
#7102=CARTESIAN_POINT('Ctrl Pts',(-12.1632051823574,26.648856626464,-0.605278801658912));
#7103=CARTESIAN_POINT('Ctrl Pts',(-12.1406760102577,26.6607219377135,-0.906882717860236));
#7104=CARTESIAN_POINT('Ctrl Pts',(-12.1341314731588,26.6641687119366,-0.994496146796198));
#7105=CARTESIAN_POINT('Ctrl Pts',(-12.1266386202186,26.6676154861597,-1.08203724349874));
#7106=CARTESIAN_POINT('Ctrl Pts',(-12.1181992022146,26.6710622603828,-1.16948635966588));
#7107=CARTESIAN_POINT('Ctrl Pts',(-12.0909050509449,26.6822095666301,-1.45230792437143));
#7108=CARTESIAN_POINT('Ctrl Pts',(-12.0537015189063,26.6933568728774,-1.73421580133404));
#7109=CARTESIAN_POINT('Ctrl Pts',(-12.0066737159719,26.7045041791248,-2.01450652225056));
#7110=CARTESIAN_POINT('Ctrl Pts',(-11.9596539007038,26.7156495920035,-2.29474963582362));
#7111=CARTESIAN_POINT('Ctrl Pts',(-11.9028131901233,26.7267950048823,-2.57337587876628));
#7112=CARTESIAN_POINT('Ctrl Pts',(-11.8362881790818,26.737940417761,-2.84968987641259));
#7113=CARTESIAN_POINT('Ctrl Pts',(-11.7697705533498,26.7490845933258,-3.12597319891336));
#7114=CARTESIAN_POINT('Ctrl Pts',(-11.6935708363978,26.7602287688906,-3.39994452942677));
#7115=CARTESIAN_POINT('Ctrl Pts',(-11.6078763665936,26.7713729444554,-3.67092038974925));
#7116=CARTESIAN_POINT('Ctrl Pts',(-11.5194832038473,26.7828680727481,-3.95042983039985));
#7117=CARTESIAN_POINT('Ctrl Pts',(-11.4209876598191,26.7943632010408,-4.22675179091095));
#7118=CARTESIAN_POINT('Ctrl Pts',(-11.3126507894069,26.8058583293335,-4.49915351671094));
#7119=CARTESIAN_POINT('Ctrl Pts',(-11.2076158915104,26.8170031004714,-4.763252778092));
#7120=CARTESIAN_POINT('Ctrl Pts',(-11.0933307897004,26.8281478716092,-5.02366697453654));
#7121=CARTESIAN_POINT('Ctrl Pts',(-10.9700825475829,26.839292642747,-5.27974801948126));
#7122=CARTESIAN_POINT('Ctrl Pts',(-10.8410224898273,26.8509629496171,-5.54790465914499));
#7123=CARTESIAN_POINT('Ctrl Pts',(-10.7021337694083,26.8626332564873,-5.81130936507168));
#7124=CARTESIAN_POINT('Ctrl Pts',(-10.553800908055,26.8743035633574,-6.06924514607354));
#7125=CARTESIAN_POINT('Ctrl Pts',(-10.4054680467018,26.8859738702276,-6.32718092707538));
#7126=CARTESIAN_POINT('Ctrl Pts',(-10.2476912192782,26.8976441770977,-6.57964749669029));
#7127=CARTESIAN_POINT('Ctrl Pts',(-10.0809087053182,26.9093144839679,-6.82596000025198));
#7128=CARTESIAN_POINT('Ctrl Pts',(-9.92160048999432,26.9204617902149,-7.06123409717429));
#7129=CARTESIAN_POINT('Ctrl Pts',(-9.75402843997352,26.931609096462,-7.29096385566852));
#7130=CARTESIAN_POINT('Ctrl Pts',(-9.57860392681835,26.9427564027091,-7.51457231405355));
#7131=CARTESIAN_POINT('Ctrl Pts',(-9.40320920949447,26.9539018155876,-7.73814279257031));
#7132=CARTESIAN_POINT('Ctrl Pts',(-9.2199648564318,26.9650472284661,-7.95559383695199));
#7133=CARTESIAN_POINT('Ctrl Pts',(-9.02932357316257,26.9761926413446,-8.16638023001199));
#7134=CARTESIAN_POINT('Ctrl Pts',(-8.83870345403747,26.9873368169091,-8.37714322250773));
#7135=CARTESIAN_POINT('Ctrl Pts',(-8.64068822334226,26.9984809924736,-8.58124284331955));
#7136=CARTESIAN_POINT('Ctrl Pts',(-8.43576944971309,27.0096251680382,-8.77816860405902));
#7137=CARTESIAN_POINT('Ctrl Pts',(-8.22439736760149,27.0211202963311,-8.98129595706688));
#7138=CARTESIAN_POINT('Ctrl Pts',(-8.00568009069493,27.032615424624,-9.17679007677322));
#7139=CARTESIAN_POINT('Ctrl Pts',(-7.78019749632778,27.0441105529169,-9.36413248347838));
#7140=CARTESIAN_POINT('Ctrl Pts',(-7.56158732985657,27.0552553240544,-9.54576492757846));
#7141=CARTESIAN_POINT('Ctrl Pts',(-7.3366183506728,27.066400095192,-9.71973503020182));
#7142=CARTESIAN_POINT('Ctrl Pts',(-7.10585275617098,27.0775448663295,-9.88561110188022));
#7143=CARTESIAN_POINT('Ctrl Pts',(-6.86420532619913,27.0892151732001,-10.0593091199987));
#7144=CARTESIAN_POINT('Ctrl Pts',(-6.61620170182717,27.1008854800707,-10.2241312000397));
#7145=CARTESIAN_POINT('Ctrl Pts',(-6.3625226287518,27.1125557869413,-10.3796317877187));
#7146=CARTESIAN_POINT('Ctrl Pts',(-6.10884355567643,27.1242260938118,-10.5351323753978));
#7147=CARTESIAN_POINT('Ctrl Pts',(-5.84948932452369,27.1358964006824,-10.6813113028628));
#7148=CARTESIAN_POINT('Ctrl Pts',(-5.58517250510067,27.147566707553,-10.8177769591662));
#7149=CARTESIAN_POINT('Ctrl Pts',(-5.33270094929267,27.1587140138001,-10.9481269559485));
#7150=CARTESIAN_POINT('Ctrl Pts',(-5.07562641811087,27.1698613200473,-11.0696540694031));
#7151=CARTESIAN_POINT('Ctrl Pts',(-4.81458622303291,27.1810086262944,-11.1820485489458));
#7152=CARTESIAN_POINT('Ctrl Pts',(-4.55359036559887,27.192154039173,-11.2944239383005));
#7153=CARTESIAN_POINT('Ctrl Pts',(-4.28863043395543,27.2032994520515,-11.397669685218));
#7154=CARTESIAN_POINT('Ctrl Pts',(-4.02036484236643,27.2144448649301,-11.4915236928905));
#7155=CARTESIAN_POINT('Ctrl Pts',(-3.75212903242545,27.2255890404947,-11.5853672813102));
#7156=CARTESIAN_POINT('Ctrl Pts',(-3.48058854705728,27.2367332160593,-11.6698211243842));
#7157=CARTESIAN_POINT('Ctrl Pts',(-3.20641930561617,27.2478773916239,-11.7446722170766));
#7158=CARTESIAN_POINT('Ctrl Pts',(-2.92361591777954,27.2593725199168,-11.8218805227401));
#7159=CARTESIAN_POINT('Ctrl Pts',(-2.63801580485302,27.2708676482096,-11.8888713695227));
#7160=CARTESIAN_POINT('Ctrl Pts',(-2.35037625108813,27.2823627765025,-11.9454669949869));
#7161=CARTESIAN_POINT('Ctrl Pts',(-2.07150359171745,27.2935075476401,-12.0003376564636));
#7162=CARTESIAN_POINT('Ctrl Pts',(-1.79071424363557,27.3046523187777,-12.0454373261581));
#7163=CARTESIAN_POINT('Ctrl Pts',(-1.50870843413845,27.3157970899153,-12.0806559884288));
#7164=CARTESIAN_POINT('Ctrl Pts',(-1.21340453821725,27.3274673967858,-12.1175353995168));
#7165=CARTESIAN_POINT('Ctrl Pts',(-0.916767010429212,27.3391377036562,-12.1435794559706));
#7166=CARTESIAN_POINT('Ctrl Pts',(-0.619606806006443,27.3508080105267,-12.1587226983738));
#7167=CARTESIAN_POINT('Ctrl Pts',(-0.322446601583674,27.3624783173972,-12.173865940777));
#7168=CARTESIAN_POINT('Ctrl Pts',(-0.0247640560390245,27.3741486242676,
-12.1781083608214));
#7169=CARTESIAN_POINT('Ctrl Pts',(0.272627745971015,27.3858189311381,-12.1714470940035));
#7170=CARTESIAN_POINT('Ctrl Pts',(0.556692040867883,27.3969662373852,-12.1650843494728));
#7171=CARTESIAN_POINT('Ctrl Pts',(0.840575917591387,27.4081135436323,-12.1487718259602));
#7172=CARTESIAN_POINT('Ctrl Pts',(1.12357154681536,27.4192608498795,-12.1225425232988));
#7173=CARTESIAN_POINT('Ctrl Pts',(1.40651910926765,27.430406262758,-12.0963176756811));
#7174=CARTESIAN_POINT('Ctrl Pts',(1.68857845992167,27.4415516756366,-12.0601794363548));
#7175=CARTESIAN_POINT('Ctrl Pts',(1.96904604421539,27.4526970885152,-12.0142127468162));
#7176=CARTESIAN_POINT('Ctrl Pts',(2.24948249224993,27.4638412640798,-11.9682511602942));
#7177=CARTESIAN_POINT('Ctrl Pts',(2.52832726361977,27.4749854396443,-11.9124633454658));
#7178=CARTESIAN_POINT('Ctrl Pts',(2.80488492567751,27.4861296152089,-11.8469857264921));
#7179=CARTESIAN_POINT('Ctrl Pts',(3.09015195034895,27.4976247435018,-11.7794460842771));
#7180=CARTESIAN_POINT('Ctrl Pts',(3.37298518903564,27.5091198717946,-11.7015965039929));
#7181=CARTESIAN_POINT('Ctrl Pts',(3.65263463056838,27.5206150000875,-11.6136432916451));
#7182=CARTESIAN_POINT('Ctrl Pts',(3.92376070634925,27.5317597712251,-11.5283707833737));
#7183=CARTESIAN_POINT('Ctrl Pts',(4.19189392120749,27.5429045423627,-11.4336014988325));
#7184=CARTESIAN_POINT('Ctrl Pts',(4.4563667833834,27.5540493135003,-11.329573925879));
#7185=CARTESIAN_POINT('Ctrl Pts',(4.73331095948184,27.5657196203708,-11.2206408949203));
#7186=CARTESIAN_POINT('Ctrl Pts',(5.00624097019272,27.5773899272413,-11.1015555262876));
#7187=CARTESIAN_POINT('Ctrl Pts',(5.27441341956718,27.5890602341118,-10.9726484191142));
#7188=CARTESIAN_POINT('Ctrl Pts',(5.54258586894163,27.6007305409822,-10.8437413119408));
#7189=CARTESIAN_POINT('Ctrl Pts',(5.80600045840199,27.6124008478527,-10.7050126194888));
#7190=CARTESIAN_POINT('Ctrl Pts',(6.06394187656684,27.6240711547232,-10.5568489222693));
#7191=CARTESIAN_POINT('Ctrl Pts',(6.31032374244294,27.6352184609703,-10.4153251280848));
#7192=CARTESIAN_POINT('Ctrl Pts',(6.55178579543794,27.6463657672174,-10.2651511261732));
#7193=CARTESIAN_POINT('Ctrl Pts',(6.78772230773284,27.6575130734645,-10.1066946190684));
#7194=CARTESIAN_POINT('Ctrl Pts',(7.02361874624126,27.6686584863431,-9.94826502578106));
#7195=CARTESIAN_POINT('Ctrl Pts',(7.25399129643232,27.6798038992216,-9.78155588460602));
#7196=CARTESIAN_POINT('Ctrl Pts',(7.47826284030866,27.6909493121002,-9.60697846053892));
#7197=CARTESIAN_POINT('Ctrl Pts',(7.70250948655965,27.7020934876648,-9.43242041727788));
#7198=CARTESIAN_POINT('Ctrl Pts',(7.92065626853127,27.7132376632294,-9.24999599917782));
#7199=CARTESIAN_POINT('Ctrl Pts',(8.13215783644281,27.724381838794,-9.06015778964041));
#7200=CARTESIAN_POINT('Ctrl Pts',(8.35032001839985,27.7358769670868,-8.86434118922249));
#7201=CARTESIAN_POINT('Ctrl Pts',(8.56141143418563,27.7473720953797,-8.66063647097069));
#7202=CARTESIAN_POINT('Ctrl Pts',(8.76487225201568,27.7588672236726,-8.44958369719158));
#7203=CARTESIAN_POINT('Ctrl Pts',(8.96213183819983,27.7700119948102,-8.24496354839487));
#7204=CARTESIAN_POINT('Ctrl Pts',(9.15221888712477,27.7811567659477,-8.03343683132685));
#7205=CARTESIAN_POINT('Ctrl Pts',(9.33466142474239,27.7923015370853,-7.81553237696745));
#7206=CARTESIAN_POINT('Ctrl Pts',(9.52570710651933,27.8039718439558,-7.58735255887823));
#7207=CARTESIAN_POINT('Ctrl Pts',(9.70836976594012,27.8156421508263,-7.35217928526387));
#7208=CARTESIAN_POINT('Ctrl Pts',(9.8821548593783,27.8273124576968,-7.11065859012131));
#7209=CARTESIAN_POINT('Ctrl Pts',(10.0559399528165,27.8389827645673,-6.86913789497875));
#7210=CARTESIAN_POINT('Ctrl Pts',(10.2208472914441,27.8506530714378,-6.62127005576414));
#7211=CARTESIAN_POINT('Ctrl Pts',(10.3764337811701,27.8623233783083,-6.36773682205794));
#7212=CARTESIAN_POINT('Ctrl Pts',(10.5250477180731,27.8734706845554,-6.12556558943235));
#7213=CARTESIAN_POINT('Ctrl Pts',(10.6652022492297,27.8846179908025,-5.87815325893289));
#7214=CARTESIAN_POINT('Ctrl Pts',(10.7965414680425,27.8957652970496,-5.62611256364813));
#7215=CARTESIAN_POINT('Ctrl Pts',(10.9278583789057,27.9069107099282,-5.37411467744332));
#7216=CARTESIAN_POINT('Ctrl Pts',(11.0503628435203,27.9180561228068,-5.11749023242191));
#7217=CARTESIAN_POINT('Ctrl Pts',(11.1637449230495,27.9292015356854,-4.85687652129296));
#7218=CARTESIAN_POINT('Ctrl Pts',(11.2771144154065,27.94034571125,-4.59629174233456));
#7219=CARTESIAN_POINT('Ctrl Pts',(11.3813634385435,27.9514898868146,-4.33171882614916));
#7220=CARTESIAN_POINT('Ctrl Pts',(11.4762297207817,27.9626340623792,-4.06381614321401));
#7221=CARTESIAN_POINT('Ctrl Pts',(11.5740835349712,27.974129190672,-3.78747666054106));
#7222=CARTESIAN_POINT('Ctrl Pts',(11.6619539607177,27.9856243189649,-3.50759456690958));
#7223=CARTESIAN_POINT('Ctrl Pts',(11.7396078726036,27.9971194472577,-3.22491197515578));
#7224=CARTESIAN_POINT('Ctrl Pts',(11.8148949902295,28.0082642183954,-2.95084519578453));
#7225=CARTESIAN_POINT('Ctrl Pts',(11.8805790712358,28.019408989533,-2.67414637087711));
#7226=CARTESIAN_POINT('Ctrl Pts',(11.9364987602759,28.0305537606706,-2.39550570776437));
#7227=CARTESIAN_POINT('Ctrl Pts',(11.9950553625732,28.042224067541,-2.1037256429279));
#7228=CARTESIAN_POINT('Ctrl Pts',(12.0429044652634,28.0538943744115,-1.80981650877137));
#7229=CARTESIAN_POINT('Ctrl Pts',(12.0799209821079,28.065564681282,-1.51458222491547));
#7230=CARTESIAN_POINT('Ctrl Pts',(12.1169374989523,28.0772349881525,-1.21934794105957));
#7231=CARTESIAN_POINT('Ctrl Pts',(12.1431213969226,28.0889052950229,-0.922788841490883));
#7232=CARTESIAN_POINT('Ctrl Pts',(12.158409857211,28.1005756018934,-0.625715585608539));
#7233=CARTESIAN_POINT('Ctrl Pts',(12.1730131706264,28.1117229081405,-0.34195556130913));
#7234=CARTESIAN_POINT('Ctrl Pts',(12.1776804928749,28.1228702143876,-0.0576417030646985));
#7235=CARTESIAN_POINT('Ctrl Pts',(12.1723925340344,28.1340175206348,0.226517653580774));
#7236=CARTESIAN_POINT('Ctrl Pts',(12.167105473353,28.1451629335133,0.510628745795714));
#7237=CARTESIAN_POINT('Ctrl Pts',(12.1518665124317,28.1563083463919,0.794585122204064));
#7238=CARTESIAN_POINT('Ctrl Pts',(12.126708476824,28.1674537592705,1.07767887987282));
#7239=CARTESIAN_POINT('Ctrl Pts',(12.1015532341492,28.1785979348351,1.36074120973675));
#7240=CARTESIAN_POINT('Ctrl Pts',(12.0664811392585,28.1897421103997,1.64294084645477));
#7241=CARTESIAN_POINT('Ctrl Pts',(12.0215769591466,28.2008862859643,1.92357419022913));
#7242=CARTESIAN_POINT('Ctrl Pts',(11.9752586551788,28.2123814142571,2.21304524811395));
#7243=CARTESIAN_POINT('Ctrl Pts',(11.9184790037928,28.22387654255,2.50084946845287));
#7244=CARTESIAN_POINT('Ctrl Pts',(11.8513884385692,28.2353716708428,2.78622366800464));
#7245=CARTESIAN_POINT('Ctrl Pts',(11.7863427099908,28.2465164419804,3.06290001832938));
#7246=CARTESIAN_POINT('Ctrl Pts',(11.711605351783,28.257661213118,3.33729201072506));
#7247=CARTESIAN_POINT('Ctrl Pts',(11.6273649772611,28.2688059842556,3.60871638336431));
#7248=CARTESIAN_POINT('Ctrl Pts',(11.5391522172666,28.2804762911261,3.89293987092784));
#7249=CARTESIAN_POINT('Ctrl Pts',(11.4405187337417,28.2921465979966,4.1739088224095));
#7250=CARTESIAN_POINT('Ctrl Pts',(11.3317394027964,28.3038169048671,4.4508574855988));
#7251=CARTESIAN_POINT('Ctrl Pts',(11.2229600718511,28.3154872117375,4.72780614878812));
#7252=CARTESIAN_POINT('Ctrl Pts',(11.1040350243111,28.327157518608,5.00073421461789));
#7253=CARTESIAN_POINT('Ctrl Pts',(10.9752970363654,28.3388278254785,5.26889981054376));
#7254=CARTESIAN_POINT('Ctrl Pts',(10.8523283952496,28.3499751317256,5.52504766131596));
#7255=CARTESIAN_POINT('Ctrl Pts',(10.7203702820013,28.3611224379727,5.77692701782369));
#7256=CARTESIAN_POINT('Ctrl Pts',(10.5797447276347,28.3722697442198,6.02390668487535));
#7257=CARTESIAN_POINT('Ctrl Pts',(10.4391430585005,28.3834151570984,6.2708444024621));
#7258=CARTESIAN_POINT('Ctrl Pts',(10.2898770193584,28.394560569977,6.51288386038532));
#7259=CARTESIAN_POINT('Ctrl Pts',(10.1323141949373,28.4057059828556,6.74941918279437));
#7260=CARTESIAN_POINT('Ctrl Pts',(9.97476886243759,28.4168501584201,6.98592824610783));
#7261=CARTESIAN_POINT('Ctrl Pts',(9.80892873173758,28.4279943339847,7.21693417212062));
#7262=CARTESIAN_POINT('Ctrl Pts',(9.63520493625646,28.4391385095493,7.44185971960901));
#7263=CARTESIAN_POINT('Ctrl Pts',(9.45601022553033,28.4506336378422,7.67386862953109));
#7264=CARTESIAN_POINT('Ctrl Pts',(9.26842743225017,28.462128766135,7.89940774747224));
#7265=CARTESIAN_POINT('Ctrl Pts',(9.07295386254082,28.4736238944279,8.11787893838075));
#7266=CARTESIAN_POINT('Ctrl Pts',(8.88343808312899,28.4847686655655,8.32969140021698));
#7267=CARTESIAN_POINT('Ctrl Pts',(8.68650559273321,28.4959134367031,8.53486019031224));
#7268=CARTESIAN_POINT('Ctrl Pts',(8.48264897593018,28.5070582078407,8.73287562038706));
#7269=CARTESIAN_POINT('Ctrl Pts',(8.26917942628235,28.5187285147112,8.94022854002387));
#7270=CARTESIAN_POINT('Ctrl Pts',(8.04811724601421,28.5303988215817,9.13973700657147));
#7271=CARTESIAN_POINT('Ctrl Pts',(7.82007023915216,28.5420691284521,9.33086018032243));
#7272=CARTESIAN_POINT('Ctrl Pts',(7.59202323229009,28.5537394353226,9.5219833540734));
#7273=CARTESIAN_POINT('Ctrl Pts',(7.35699166160939,28.5654097421931,9.70472102625257));
#7274=CARTESIAN_POINT('Ctrl Pts',(7.1156227436877,28.5770800490636,9.87858103269464));
#7275=CARTESIAN_POINT('Ctrl Pts',(6.88507088945431,28.5882273455408,10.0446494196576));
#7276=CARTESIAN_POINT('Ctrl Pts',(6.64866836787934,28.5993746420181,10.202667962098));
#7277=CARTESIAN_POINT('Ctrl Pts',(6.4069999951961,28.6105219384953,10.3522365366889));
#7278=CARTESIAN_POINT('Ctrl Pts',(6.1653727278874,28.6216673389289,10.5017796711604));
#7279=CARTESIAN_POINT('Ctrl Pts',(5.91848162441142,28.6328127393624,10.6428755669444));
#7280=CARTESIAN_POINT('Ctrl Pts',(5.66693938316602,28.6439581397959,10.7751681322159));
#7281=CARTESIAN_POINT('Ctrl Pts',(5.41542512736357,28.655102300243,10.9074459792198));
#7282=CARTESIAN_POINT('Ctrl Pts',(5.15926100311546,28.6662464606901,11.0309223273304));
#7283=CARTESIAN_POINT('Ctrl Pts',(4.89908424391283,28.6773906211372,11.1452870676822));
#7284=CARTESIAN_POINT('Ctrl Pts',(4.63611072826147,28.6886545751535,11.2608811658217));
#7285=CARTESIAN_POINT('Ctrl Pts',(4.36903806075543,28.6999185291697,11.3671665133374));
#7286=CARTESIAN_POINT('Ctrl Pts',(4.09854619613597,28.711182483186,11.4638723530986));
#7287=CARTESIAN_POINT('Ctrl Pts',(3.83091820433177,28.7223271784151,11.5595543054096));
#7288=CARTESIAN_POINT('Ctrl Pts',(3.5599433215539,28.7334718736442,11.6458585229986));
#7289=CARTESIAN_POINT('Ctrl Pts',(3.28629764156213,28.7446165688734,11.7225721606251));
#7290=CARTESIAN_POINT('Ctrl Pts',(3.00825955990872,28.7559401522832,11.8005171610467));
#7291=CARTESIAN_POINT('Ctrl Pts',(2.72746448770561,28.767263735693,11.8685610136402));
#7292=CARTESIAN_POINT('Ctrl Pts',(2.44463594005741,28.7785873191028,11.9265336695362));
#7293=CARTESIAN_POINT('Ctrl Pts',(2.16180739240921,28.7899109025126,11.9845063254321));
#7294=CARTESIAN_POINT('Ctrl Pts',(1.87694565348214,28.8012344859224,12.0324077339315));
#7295=CARTESIAN_POINT('Ctrl Pts',(1.59078448392775,28.8125580693322,12.0701224093086));
#7296=CARTESIAN_POINT('Origin',(0.,13.3748739960349,0.));
#7297=CARTESIAN_POINT('',(1.59071714630986,32.0622959365534,12.0696162300787));
#7298=CARTESIAN_POINT('',(1.59078448392771,31.8125557231064,12.0701224093087));
#7299=CARTESIAN_POINT('',(1.59078448392774,13.3748739960349,12.0701224093086));
#7300=CARTESIAN_POINT('',(-12.174396721221,29.8748739960031,-4.71261348963091E-6));
#7301=CARTESIAN_POINT('Ctrl Pts',(-12.1734593809614,29.8748739960349,-4.71306082890088E-6));
#7302=CARTESIAN_POINT('Ctrl Pts',(-12.1734729483294,29.9143848671652,-1.00768895467666));
#7303=CARTESIAN_POINT('Ctrl Pts',(-11.8010964029253,30.0333131461572,-4.04082287428804));
#7304=CARTESIAN_POINT('Ctrl Pts',(-9.30992091872449,30.2316588330109,-8.62536224638919));
#7305=CARTESIAN_POINT('Ctrl Pts',(-4.04710485413492,30.469911056596,-12.0288172192438));
#7306=CARTESIAN_POINT('Ctrl Pts',(2.2026844913737,30.7081632801811,-12.4987872382004));
#7307=CARTESIAN_POINT('Ctrl Pts',(7.91530200229061,30.9464155037662,-9.92066003887209));
#7308=CARTESIAN_POINT('Ctrl Pts',(11.6976034309138,31.1846677273513,-4.92316720896363));
#7309=CARTESIAN_POINT('Ctrl Pts',(12.6271934885173,31.4229199509364,1.27494548820119));
#7310=CARTESIAN_POINT('Ctrl Pts',(10.4773717109103,31.6611721745215,7.16213539565936));
#7311=CARTESIAN_POINT('Ctrl Pts',(6.26861872634805,31.8742975030605,10.866008505099));
#7312=CARTESIAN_POINT('Ctrl Pts',(2.96313964180942,32.0080054237378,11.8875089580627));
#7313=CARTESIAN_POINT('Ctrl Pts',(1.59071714630986,32.0622959365534,12.0696162300787));
#7314=CARTESIAN_POINT('Ctrl Pts',(1.59078448392773,29.0623127728906,12.0701224093086));
#7315=CARTESIAN_POINT('Ctrl Pts',(1.30906809259831,29.0734587642939,12.107251284145));
#7316=CARTESIAN_POINT('Ctrl Pts',(1.02601695318895,29.0846047556973,12.1345174913886));
#7317=CARTESIAN_POINT('Ctrl Pts',(0.742335843504071,29.0957507471006,12.1518470919218));
#7318=CARTESIAN_POINT('Ctrl Pts',(0.458691979131175,29.1068952751145,12.1691744172018));
#7319=CARTESIAN_POINT('Ctrl Pts',(0.174418575804354,29.1180398031285,12.176567724411));
#7320=CARTESIAN_POINT('Ctrl Pts',(-0.109776022248343,29.1291843311424,12.1740050712549));
#7321=CARTESIAN_POINT('Ctrl Pts',(-0.3939500234525,29.1403280514627,12.1714426038256));
#7322=CARTESIAN_POINT('Ctrl Pts',(-0.67804496411194,29.1514717717831,12.1589256196025));
#7323=CARTESIAN_POINT('Ctrl Pts',(-0.961352806067982,29.1626154921034,12.1364842945667));
#7324=CARTESIAN_POINT('Ctrl Pts',(-1.24468790631768,29.1737602846101,12.1140408103524));
#7325=CARTESIAN_POINT('Ctrl Pts',(-1.52723549039379,29.1849050771168,12.0816710959945));
#7326=CARTESIAN_POINT('Ctrl Pts',(-1.80829146499432,29.1960498696235,12.0394573061924));
#7327=CARTESIAN_POINT('Ctrl Pts',(-2.08935117658927,29.2071948103143,11.9972429551045));
#7328=CARTESIAN_POINT('Ctrl Pts',(-2.36891897565992,29.2183397510051,11.945184309298));
#7329=CARTESIAN_POINT('Ctrl Pts',(-2.64629886222554,29.2294846916959,11.8834150218607));
#7330=CARTESIAN_POINT('Ctrl Pts',(-2.92373516566913,29.2406318991796,11.8216331710381));
#7331=CARTESIAN_POINT('Ctrl Pts',(-3.19898240695043,29.2517791066633,11.7501367899863));
#7332=CARTESIAN_POINT('Ctrl Pts',(-3.47135621080027,29.262926314147,11.6691103477402));
#7333=CARTESIAN_POINT('Ctrl Pts',(-3.59942127187903,29.2681675223215,11.6310132322006));
#7334=CARTESIAN_POINT('Ctrl Pts',(-3.72685129803498,29.273408730496,11.5908100241812));
#7335=CARTESIAN_POINT('Ctrl Pts',(-3.85357632161499,29.2786499386705,11.5485237058028));
#7336=CARTESIAN_POINT('Ctrl Pts',(-4.12310246901941,29.2897972449176,11.4585867055287));
#7337=CARTESIAN_POINT('Ctrl Pts',(-4.38951899259722,29.3009445511647,11.3591966162271));
#7338=CARTESIAN_POINT('Ctrl Pts',(-4.6521593504558,29.3120918574118,11.2505939233432));
#7339=CARTESIAN_POINT('Ctrl Pts',(-4.91475509888349,29.3232372702904,11.1420096766126));
#7340=CARTESIAN_POINT('Ctrl Pts',(-5.17357571569878,29.334382683169,11.0242160522333));
#7341=CARTESIAN_POINT('Ctrl Pts',(-5.42797407681333,29.3455280960475,10.8975019005019));
#7342=CARTESIAN_POINT('Ctrl Pts',(-5.6823441957571,29.3566722716121,10.7708018160101));
#7343=CARTESIAN_POINT('Ctrl Pts',(-5.93229280062091,29.3678164471767,10.6351833005704));
#7344=CARTESIAN_POINT('Ctrl Pts',(-6.17719572531667,29.3789606227413,10.4909819950818));
#7345=CARTESIAN_POINT('Ctrl Pts',(-6.42981114063938,29.3904557510341,10.3422394975337));
#7346=CARTESIAN_POINT('Ctrl Pts',(-6.67705766802888,29.401950879327,10.1843650133687));
#7347=CARTESIAN_POINT('Ctrl Pts',(-6.91827962488502,29.4134460076199,10.0177770628968));
#7348=CARTESIAN_POINT('Ctrl Pts',(-7.15214943773397,29.4245907787575,9.85626650512033));
#7349=CARTESIAN_POINT('Ctrl Pts',(-7.38035625506969,29.435735549895,9.68656592549784));
#7350=CARTESIAN_POINT('Ctrl Pts',(-7.60233273639457,29.4468803210327,9.50910023162778));
#7351=CARTESIAN_POINT('Ctrl Pts',(-7.83477659936034,29.4585506279031,9.32326607847403));
#7352=CARTESIAN_POINT('Ctrl Pts',(-8.06038815211785,29.4702209347736,9.1289170547268));
#7353=CARTESIAN_POINT('Ctrl Pts',(-8.27855472469357,29.4818912416441,8.92658848162353));
#7354=CARTESIAN_POINT('Ctrl Pts',(-8.49672129726929,29.4935615485146,8.72425990852026));
#7355=CARTESIAN_POINT('Ctrl Pts',(-8.70744264963627,29.5052318553851,8.51395202063495));
#7356=CARTESIAN_POINT('Ctrl Pts',(-8.91014947085614,29.5169021622556,8.29624533490916));
#7357=CARTESIAN_POINT('Ctrl Pts',(-9.10377205847044,29.5280494685027,8.08829509634546));
#7358=CARTESIAN_POINT('Ctrl Pts',(-9.29014048970121,29.5391967747498,7.87353252575311));
#7359=CARTESIAN_POINT('Ctrl Pts',(-9.46878458047568,29.550344080997,7.65248775357047));
#7360=CARTESIAN_POINT('Ctrl Pts',(-9.64739832857408,29.5614894938755,7.43148052581425));
#7361=CARTESIAN_POINT('Ctrl Pts',(-9.81829018797549,29.5726349067541,7.2041934341806));
#7362=CARTESIAN_POINT('Ctrl Pts',(-9.98103016933431,29.5837803196327,6.97118978430787));
#7363=CARTESIAN_POINT('Ctrl Pts',(-10.143752084027,29.5949244951972,6.73821200146009));
#7364=CARTESIAN_POINT('Ctrl Pts',(-10.2983237750866,29.6060686707618,6.49951914625352));
#7365=CARTESIAN_POINT('Ctrl Pts',(-10.4443578030689,29.6172128463264,6.2557046230999));
#7366=CARTESIAN_POINT('Ctrl Pts',(-10.594990739265,29.6287079746193,6.00421188529549));
#7367=CARTESIAN_POINT('Ctrl Pts',(-10.7365394011799,29.6402031029121,5.74726991837197));
#7368=CARTESIAN_POINT('Ctrl Pts',(-10.868628337183,29.651698231205,5.48555998218799));
#7369=CARTESIAN_POINT('Ctrl Pts',(-10.9966913673694,29.6628430023426,5.23182663803549));
#7370=CARTESIAN_POINT('Ctrl Pts',(-11.1158626482813,29.6739877734802,4.97361191341933));
#7371=CARTESIAN_POINT('Ctrl Pts',(-11.2258473549232,29.6851325446178,4.71156040117959));
#7372=CARTESIAN_POINT('Ctrl Pts',(-11.341018430374,29.6968028514883,4.43715175465375));
#7373=CARTESIAN_POINT('Ctrl Pts',(-11.4461155690856,29.7084731583587,4.15853605659713));
#7374=CARTESIAN_POINT('Ctrl Pts',(-11.5408569815104,29.7201434652292,3.8764765422123));
#7375=CARTESIAN_POINT('Ctrl Pts',(-11.6355983939352,29.7318137720997,3.59441702782744));
#7376=CARTESIAN_POINT('Ctrl Pts',(-11.7199839815676,29.7434840789702,3.30891401794856));
#7377=CARTESIAN_POINT('Ctrl Pts',(-11.7937916549543,29.7551543858407,3.02074968336178));
#7378=CARTESIAN_POINT('Ctrl Pts',(-11.8651552549867,29.7664382412116,2.74212764620159));
#7379=CARTESIAN_POINT('Ctrl Pts',(-11.9266493212993,29.7777220965825,2.46094394049381));
#7380=CARTESIAN_POINT('Ctrl Pts',(-11.9781123416308,29.7890059519535,2.17790610019643));
#7381=CARTESIAN_POINT('Ctrl Pts',(-12.0295653763274,29.8002876178598,1.89492317918895));
#7382=CARTESIAN_POINT('Ctrl Pts',(-12.0709912069458,29.8115692837662,1.61008709067454));
#7383=CARTESIAN_POINT('Ctrl Pts',(-12.1022795090425,29.8228509496725,1.32411515171836));
#7384=CARTESIAN_POINT('Ctrl Pts',(-12.1335625490621,29.8341307182245,1.03819130761862));
#7385=CARTESIAN_POINT('Ctrl Pts',(-12.1547114378685,29.8454104867765,0.751132245746415));
#7386=CARTESIAN_POINT('Ctrl Pts',(-12.1656676092229,29.8566902553285,0.463661376334469));
#7387=CARTESIAN_POINT('Ctrl Pts',(-12.1715549693444,29.8627515022189,0.309187292468078));
#7388=CARTESIAN_POINT('Ctrl Pts',(-12.1745000598421,29.8688127491093,0.154594386717212));
#7389=CARTESIAN_POINT('Ctrl Pts',(-12.1744999999991,29.8748739959996,-4.71256420053583E-6));
#7390=CARTESIAN_POINT('',(-12.1744999986658,29.6251260039304,0.000180241411394071));
#7391=CARTESIAN_POINT('Ctrl Pts',(1.59078448392775,28.8125580693322,12.0701224093086));
#7392=CARTESIAN_POINT('Ctrl Pts',(1.56741528365208,28.813482803771,12.0732023582884));
#7393=CARTESIAN_POINT('Ctrl Pts',(1.5440374216093,28.8144075382099,12.0762144014192));
#7394=CARTESIAN_POINT('Ctrl Pts',(1.52065129953035,28.8153322726487,12.0791584920158));
#7395=CARTESIAN_POINT('Ctrl Pts',(1.2387408895783,28.8264795788958,12.114648334419));
#7396=CARTESIAN_POINT('Ctrl Pts',(0.955545409716462,28.8376268851429,12.1402700844111));
#7397=CARTESIAN_POINT('Ctrl Pts',(0.671769844144576,28.84877419139,12.1559522673667));
#7398=CARTESIAN_POINT('Ctrl Pts',(0.388042477816675,28.8599196042686,12.1716317867055));
#7399=CARTESIAN_POINT('Ctrl Pts',(0.103735488728669,28.8710650171472,12.1773750948538));
#7400=CARTESIAN_POINT('Ctrl Pts',(-0.180442727021527,28.8822104300257,12.1731627226561));
#7401=CARTESIAN_POINT('Ctrl Pts',(-0.464589394575869,28.8933546055903,12.1689508180973));
#7402=CARTESIAN_POINT('Ctrl Pts',(-0.748607050689398,28.9044987811549,12.154785444124));
#7403=CARTESIAN_POINT('Ctrl Pts',(-1.03178776018544,28.9156429567196,12.1306992489276));
#7404=CARTESIAN_POINT('Ctrl Pts',(-1.32388640551311,28.9271380850124,12.1058545305126));
#7405=CARTESIAN_POINT('Ctrl Pts',(-1.61509423925263,28.9386332133053,12.0704540273365));
#7406=CARTESIAN_POINT('Ctrl Pts',(-1.90463906235076,28.9501283415981,12.0245914813006));
#7407=CARTESIAN_POINT('Ctrl Pts',(-2.18535892082461,28.9612731127357,11.9801267683947));
#7408=CARTESIAN_POINT('Ctrl Pts',(-2.46451536486885,28.9724178838733,11.9258283526591));
#7409=CARTESIAN_POINT('Ctrl Pts',(-2.74141308360023,28.9835626550109,11.8618339456876));
#7410=CARTESIAN_POINT('Ctrl Pts',(-3.03136801487957,28.9952329618814,11.7948218592005));
#7411=CARTESIAN_POINT('Ctrl Pts',(-3.31884576343318,29.0069032687519,11.717177414097));
#7412=CARTESIAN_POINT('Ctrl Pts',(-3.60306239103951,29.0185735756224,11.6291182665014));
#7413=CARTESIAN_POINT('Ctrl Pts',(-3.88727901864584,29.0302438824928,11.5410591189058));
#7414=CARTESIAN_POINT('Ctrl Pts',(-4.16823420743134,29.0419141893633,11.442585376495));
#7415=CARTESIAN_POINT('Ctrl Pts',(-4.44516356389173,29.0535844962338,11.3339741988523));
#7416=CARTESIAN_POINT('Ctrl Pts',(-4.70968243040855,29.0647318024809,11.2302303922428));
#7417=CARTESIAN_POINT('Ctrl Pts',(-4.97060736729662,29.075879108728,11.117206805338));
#7418=CARTESIAN_POINT('Ctrl Pts',(-5.22728514945102,29.0870264149751,10.9951780438667));
#7419=CARTESIAN_POINT('Ctrl Pts',(-5.48391933491689,29.0981718278537,10.873170008965));
#7420=CARTESIAN_POINT('Ctrl Pts',(-5.73630756506488,29.1093172407323,10.7421599676865));
#7421=CARTESIAN_POINT('Ctrl Pts',(-5.98381850576247,29.1204626536109,10.6024698226448));
#7422=CARTESIAN_POINT('Ctrl Pts',(-6.2313019689003,29.1316068291754,10.4627951853795));
#7423=CARTESIAN_POINT('Ctrl Pts',(-6.47390899154312,29.14275100474,10.3144424996335));
#7424=CARTESIAN_POINT('Ctrl Pts',(-6.71103358465277,29.1538951803046,10.1577792098304));
#7425=CARTESIAN_POINT('Ctrl Pts',(-6.95562571292541,29.1653903085975,9.99618227476502));
#7426=CARTESIAN_POINT('Ctrl Pts',(-7.19438425759036,29.1768854368903,9.82574297352866));
#7427=CARTESIAN_POINT('Ctrl Pts',(-7.42667603774404,29.1883805651832,9.64691314775864));
#7428=CARTESIAN_POINT('Ctrl Pts',(-7.65188785452438,29.1995253363208,9.47353383175558));
#7429=CARTESIAN_POINT('Ctrl Pts',(-7.87102104620591,29.2106701074584,9.29226805311522));
#7430=CARTESIAN_POINT('Ctrl Pts',(-8.08353098601621,29.221814878596,9.10356946741858));
#7431=CARTESIAN_POINT('Ctrl Pts',(-8.30606190926227,29.2334851854665,8.90597273134222));
#7432=CARTESIAN_POINT('Ctrl Pts',(-8.52132966920872,29.245155492337,8.70022553865971));
#7433=CARTESIAN_POINT('Ctrl Pts',(-8.7287500754548,29.2568257992075,8.4868941533548));
#7434=CARTESIAN_POINT('Ctrl Pts',(-8.93617048170086,29.2684961060779,8.27356276804991));
#7435=CARTESIAN_POINT('Ctrl Pts',(-9.13574330666112,29.2801664129484,8.05264743678594));
#7436=CARTESIAN_POINT('Ctrl Pts',(-9.32692999639901,29.2918367198189,7.82475731842672));
#7437=CARTESIAN_POINT('Ctrl Pts',(-9.50954872309849,29.302984026066,7.6070800141164));
#7438=CARTESIAN_POINT('Ctrl Pts',(-9.68457097741769,29.3141313323131,7.38297431499236));
#7439=CARTESIAN_POINT('Ctrl Pts',(-9.85155459629223,29.3252786385603,7.1529939386437));
#7440=CARTESIAN_POINT('Ctrl Pts',(-10.0185098530204,29.3364240514388,6.9230526244327));
#7441=CARTESIAN_POINT('Ctrl Pts',(-10.1774290435821,29.3475694643174,6.68723884089972));
#7442=CARTESIAN_POINT('Ctrl Pts',(-10.3279118601732,29.358714877196,6.44613735957391));
#7443=CARTESIAN_POINT('Ctrl Pts',(-10.4783779708334,29.3698590527605,6.20506264425865));
#7444=CARTESIAN_POINT('Ctrl Pts',(-10.6204094365009,29.3810032283251,5.95870162955929));
#7445=CARTESIAN_POINT('Ctrl Pts',(-10.753649997694,29.3921474038897,5.70766694693163));
#7446=CARTESIAN_POINT('Ctrl Pts',(-10.8910865748418,29.4036425321825,5.44872667216268));
#7447=CARTESIAN_POINT('Ctrl Pts',(-11.019169440786,29.4151376604754,5.18481385036724));
#7448=CARTESIAN_POINT('Ctrl Pts',(-11.1375588475103,29.4266327887682,4.91662823164873));
#7449=CARTESIAN_POINT('Ctrl Pts',(-11.2523398929623,29.4377775599059,4.6566165756786));
#7450=CARTESIAN_POINT('Ctrl Pts',(-11.3580095056908,29.4489223310435,4.39258898024842));
#7451=CARTESIAN_POINT('Ctrl Pts',(-11.4543065619484,29.4600671021811,4.12520441128752));
#7452=CARTESIAN_POINT('Ctrl Pts',(-11.5551445408871,29.4717374090516,3.84521122581278));
#7453=CARTESIAN_POINT('Ctrl Pts',(-11.6457046540313,29.483407715922,3.56153714931589));
#7454=CARTESIAN_POINT('Ctrl Pts',(-11.7257449261543,29.4950780227925,3.274958958028));
#7455=CARTESIAN_POINT('Ctrl Pts',(-11.8057851982772,29.506748329663,2.98838076674009));
#7456=CARTESIAN_POINT('Ctrl Pts',(-11.8753055475832,29.5184186365335,2.69889878615673));
#7457=CARTESIAN_POINT('Ctrl Pts',(-11.9341245976263,29.530088943404,2.4073056179742));
#7458=CARTESIAN_POINT('Ctrl Pts',(-11.9917048891097,29.5415134677853,2.12185354749385));
#7459=CARTESIAN_POINT('Ctrl Pts',(-12.0390440781821,29.5529379921666,1.83431123741328));
#7460=CARTESIAN_POINT('Ctrl Pts',(-12.0760155945832,29.5643625165479,1.54541179281881));
#7461=CARTESIAN_POINT('Ctrl Pts',(-12.1129779697708,29.5757842162137,1.25658377865915));
#7462=CARTESIAN_POINT('Ctrl Pts',(-12.1395777632545,29.5872059158794,0.966399535564798));
#7463=CARTESIAN_POINT('Ctrl Pts',(-12.1557400447632,29.5986276155452,0.675599151968931));
#7464=CARTESIAN_POINT('Ctrl Pts',(-12.168238897098,29.6074604116736,0.450713138721019));
#7465=CARTESIAN_POINT('Ctrl Pts',(-12.1744966634544,29.616293207802,0.225458828196562));
#7466=CARTESIAN_POINT('Ctrl Pts',(-12.1744999986658,29.6251260039304,0.000180241411402181));
#7467=CARTESIAN_POINT('Ctrl Pts',(-12.1744999986658,29.6251260039651,0.00018024052605028));
#7468=CARTESIAN_POINT('Ctrl Pts',(-12.1745042222142,29.6363114795878,-0.285102936417017));
#7469=CARTESIAN_POINT('Ctrl Pts',(-12.1644766085762,29.6474969552104,-0.570385273907491));
#7470=CARTESIAN_POINT('Ctrl Pts',(-12.1444433863984,29.6586824308331,-0.854953264549404));
#7471=CARTESIAN_POINT('Ctrl Pts',(-12.1244071877467,29.6698695683589,-1.13956353541974));
#7472=CARTESIAN_POINT('Ctrl Pts',(-12.0943624266308,29.6810567058848,-1.42345898533909));
#7473=CARTESIAN_POINT('Ctrl Pts',(-12.0543873318725,29.6922438434107,-1.70592974743708));
#7474=CARTESIAN_POINT('Ctrl Pts',(-12.0144104223308,29.7034314888086,-1.98841333310159));
#7475=CARTESIAN_POINT('Ctrl Pts',(-11.9645023183561,29.7146191342066,-2.2694718422521));
#7476=CARTESIAN_POINT('Ctrl Pts',(-11.9047927944751,29.7258067796045,-2.54840318054546));
#7477=CARTESIAN_POINT('Ctrl Pts',(-11.8450710809749,29.7369967089452,-2.8273914622972));
#7478=CARTESIAN_POINT('Ctrl Pts',(-11.7755440050082,29.7481866382859,-3.10425144891475));
#7479=CARTESIAN_POINT('Ctrl Pts',(-11.6963922226106,29.7593765676266,-3.37829235337227));
#7480=CARTESIAN_POINT('Ctrl Pts',(-11.6752552402276,29.7623647674141,-3.4514732419674));
#7481=CARTESIAN_POINT('Ctrl Pts',(-11.6534321750649,29.7653529672017,-3.52445317187036));
#7482=CARTESIAN_POINT('Ctrl Pts',(-11.6309270707671,29.7683411669892,-3.59721916547995));
#7483=CARTESIAN_POINT('Ctrl Pts',(-11.5469730825569,29.7794884732363,-3.86866849043174));
#7484=CARTESIAN_POINT('Ctrl Pts',(-11.4534995431357,29.7906357794834,-4.13721802276228));
#7485=CARTESIAN_POINT('Ctrl Pts',(-11.3507321374569,29.8017830857305,-4.40219606488654));
#7486=CARTESIAN_POINT('Ctrl Pts',(-11.247982186809,29.8129284986091,-4.66712910052394));
#7487=CARTESIAN_POINT('Ctrl Pts',(-11.1359416179192,29.8240739114877,-4.92849160846213));
#7488=CARTESIAN_POINT('Ctrl Pts',(-11.0148848982189,29.8352193243662,-5.18563023450271));
#7489=CARTESIAN_POINT('Ctrl Pts',(-10.8938416176952,29.8463634999308,-5.44274031416114));
#7490=CARTESIAN_POINT('Ctrl Pts',(-10.7637842986543,29.8575076754954,-5.69562720699591));
#7491=CARTESIAN_POINT('Ctrl Pts',(-10.6250346954393,29.86865185106,-5.94365947634216));
#7492=CARTESIAN_POINT('Ctrl Pts',(-10.4819155853449,29.8801469793528,-6.19950278573525));
#7493=CARTESIAN_POINT('Ctrl Pts',(-10.329547980573,29.8916421076457,-6.45018048931594));
#7494=CARTESIAN_POINT('Ctrl Pts',(-10.1683357975651,29.9031372359385,-6.69502780860221));
#7495=CARTESIAN_POINT('Ctrl Pts',(-10.0120371605734,29.9142820070761,-6.93241248736197));
#7496=CARTESIAN_POINT('Ctrl Pts',(-9.84742525859584,29.9254267782137,-7.16431669157156));
#7497=CARTESIAN_POINT('Ctrl Pts',(-9.67491234763068,29.9365715493513,-7.39016382197738));
#7498=CARTESIAN_POINT('Ctrl Pts',(-9.49426452765975,29.9482418562218,-7.62666085588776));
#7499=CARTESIAN_POINT('Ctrl Pts',(-9.30495281210028,29.9599121630923,-7.85651557113396));
#7500=CARTESIAN_POINT('Ctrl Pts',(-9.10749884104637,29.9715824699628,-8.07910360809534));
#7501=CARTESIAN_POINT('Ctrl Pts',(-8.91004486999248,29.9832527768333,-8.30169164505669));
#7502=CARTESIAN_POINT('Ctrl Pts',(-8.70444887265217,29.9949230837037,-8.51701275857697));
#7503=CARTESIAN_POINT('Ctrl Pts',(-8.49127863272491,30.0065933905742,-8.7244849378877));
#7504=CARTESIAN_POINT('Ctrl Pts',(-8.28766154076552,30.0177406968213,-8.92265932577667));
#7505=CARTESIAN_POINT('Ctrl Pts',(-8.07707334551595,30.0288880030684,-9.11373199757563));
#7506=CARTESIAN_POINT('Ctrl Pts',(-7.86003364885051,30.0400353093155,-9.29722115951523));
#7507=CARTESIAN_POINT('Ctrl Pts',(-7.64303081634977,30.0511807221941,-9.48067915584417));
#7508=CARTESIAN_POINT('Ctrl Pts',(-7.41957887379889,30.0623261350727,-9.656556041771));
#7509=CARTESIAN_POINT('Ctrl Pts',(-7.19023147912979,30.0734715479513,-9.82440947469776));
#7510=CARTESIAN_POINT('Ctrl Pts',(-6.96090954558389,30.0846157235159,-9.99224427328623));
#7511=CARTESIAN_POINT('Ctrl Pts',(-6.72569368202658,30.0957598990805,-10.1520572400168));
#7512=CARTESIAN_POINT('Ctrl Pts',(-6.48516857886181,30.1069040746452,-10.3034479061013));
#7513=CARTESIAN_POINT('Ctrl Pts',(-6.2370688515653,30.118399202938,-10.4596061718149));
#7514=CARTESIAN_POINT('Ctrl Pts',(-5.98332031440759,30.1298943312309,-10.6068029039343));
#7515=CARTESIAN_POINT('Ctrl Pts',(-5.72459575688008,30.1413894595237,-10.7446476754853));
#7516=CARTESIAN_POINT('Ctrl Pts',(-5.47375680077022,30.1525342306613,-10.8782911105402));
#7517=CARTESIAN_POINT('Ctrl Pts',(-5.21824090472264,30.1636790017989,-11.0031440843534));
#7518=CARTESIAN_POINT('Ctrl Pts',(-4.95868598336946,30.1748237729366,-11.1188975878158));
#7519=CARTESIAN_POINT('Ctrl Pts',(-4.68689165538149,30.186494079807,-11.240109489797));
#7520=CARTESIAN_POINT('Ctrl Pts',(-4.4106685032706,30.1981643866775,-11.3513429650037));
#7521=CARTESIAN_POINT('Ctrl Pts',(-4.13077334331136,30.2098346935479,-11.4522994126153));
#7522=CARTESIAN_POINT('Ctrl Pts',(-3.85087818335214,30.2215050004184,-11.5532558602268));
#7523=CARTESIAN_POINT('Ctrl Pts',(-3.56731133412171,30.2331753072889,-11.643935174666));
#7524=CARTESIAN_POINT('Ctrl Pts',(-3.28084986321212,30.2448456141593,-11.7240980218122));
#7525=CARTESIAN_POINT('Ctrl Pts',(-3.00722606054148,30.2559929204064,-11.8006683996693));
#7526=CARTESIAN_POINT('Ctrl Pts',(-2.730879655486,30.2671402266535,-11.8676670436835));
#7527=CARTESIAN_POINT('Ctrl Pts',(-2.4524974507845,30.2782875329007,-11.9249195596405));
#7528=CARTESIAN_POINT('Ctrl Pts',(-2.1741625292645,30.2894329457793,-11.982162351265));
#7529=CARTESIAN_POINT('Ctrl Pts',(-1.89379275962855,30.3005783586578,-12.0296622660807));
#7530=CARTESIAN_POINT('Ctrl Pts',(-1.61208596895292,30.3117237715364,-12.0672958478155));
#7531=CARTESIAN_POINT('Ctrl Pts',(-1.33041045210901,30.322867947101,-12.1049252516379));
#7532=CARTESIAN_POINT('Ctrl Pts',(-1.04739847494732,30.3340121226655,-12.1326904742397));
#7533=CARTESIAN_POINT('Ctrl Pts',(-0.76375507464333,30.3451562982301,-12.1505196776087));
#7534=CARTESIAN_POINT('Ctrl Pts',(-0.471179167432266,30.3566514265229,-12.1689103588125));
#7535=CARTESIAN_POINT('Ctrl Pts',(-0.177931718560721,30.3681465548158,-12.1767290407253));
#7536=CARTESIAN_POINT('Ctrl Pts',(0.11520968357079,30.3796416831087,-12.1739548618685));
#7537=CARTESIAN_POINT('Ctrl Pts',(0.399416501840013,30.3907864542463,-12.1712652365189));
#7538=CARTESIAN_POINT('Ctrl Pts',(0.683523362930164,30.4019312253839,-12.1586189056607));
#7539=CARTESIAN_POINT('Ctrl Pts',(0.966822262734164,30.4130759965215,-12.136049808825));
#7540=CARTESIAN_POINT('Ctrl Pts',(1.26348022510641,30.4247463033919,-12.1124164580266));
#7541=CARTESIAN_POINT('Ctrl Pts',(1.55925187642808,30.4364166102624,-12.0779020256309));
#7542=CARTESIAN_POINT('Ctrl Pts',(1.85332979011732,30.4480869171329,-12.0326064898285));
#7543=CARTESIAN_POINT('Ctrl Pts',(2.14740770380658,30.4597572240034,-11.9873109540262));
#7544=CARTESIAN_POINT('Ctrl Pts',(2.43979154960908,30.4714275308739,-11.9312343745664));
#7545=CARTESIAN_POINT('Ctrl Pts',(2.72968448063129,30.4830978377444,-11.8645384607325));
#7546=CARTESIAN_POINT('Ctrl Pts',(3.00658596375755,30.4942451439915,-11.8008315003939));
#7547=CARTESIAN_POINT('Ctrl Pts',(3.28129758340433,30.5053924502386,-11.7274170609569));
#7548=CARTESIAN_POINT('Ctrl Pts',(3.55313282753996,30.5165397564857,-11.6444706775301));
#7549=CARTESIAN_POINT('Ctrl Pts',(3.8249219004943,30.5276851693643,-11.5615383825358));
#7550=CARTESIAN_POINT('Ctrl Pts',(4.09383531829407,30.5388305822429,-11.4690774537046));
#7551=CARTESIAN_POINT('Ctrl Pts',(4.35920126481122,30.5499759951215,-11.3673134285489));
#7552=CARTESIAN_POINT('Ctrl Pts',(4.62453775158353,30.561120170686,-11.2655607007818));
#7553=CARTESIAN_POINT('Ctrl Pts',(4.8863273044804,30.5722643462505,-11.1545070344914));
#7554=CARTESIAN_POINT('Ctrl Pts',(5.14391647798478,30.583408521815,-11.0344267416806));
#7555=CARTESIAN_POINT('Ctrl Pts',(5.40961765786553,30.5949036501079,-10.9105648765014));
#7556=CARTESIAN_POINT('Ctrl Pts',(5.67084934137553,30.6063987784008,-10.7770987550051));
#7557=CARTESIAN_POINT('Ctrl Pts',(5.92691877280664,30.6178939066936,-10.6343821687276));
#7558=CARTESIAN_POINT('Ctrl Pts',(6.17518352774736,30.6290386778313,-10.4960154057753));
#7559=CARTESIAN_POINT('Ctrl Pts',(6.41859580509325,30.6401834489689,-10.3489538491387));
#7560=CARTESIAN_POINT('Ctrl Pts',(6.65655017324196,30.6513282201065,-10.1935661101065));
#7561=CARTESIAN_POINT('Ctrl Pts',(6.90572536609043,30.662998526977,-10.0308510057743));
#7562=CARTESIAN_POINT('Ctrl Pts',(7.14891525866527,30.6746688338475,-9.85900575003922));
#7563=CARTESIAN_POINT('Ctrl Pts',(7.38545872235907,30.686339140718,-9.67850451827814));
#7564=CARTESIAN_POINT('Ctrl Pts',(7.62200218605287,30.6980094475885,-9.49800328651705));
#7565=CARTESIAN_POINT('Ctrl Pts',(7.85189895947368,30.709679754459,-9.30884628923451));
#7566=CARTESIAN_POINT('Ctrl Pts',(8.07452674462437,30.7213500613295,-9.11155684284227));
#7567=CARTESIAN_POINT('Ctrl Pts',(8.28717754530411,30.7324973675766,-8.92310885234291));
#7568=CARTESIAN_POINT('Ctrl Pts',(8.49326006179604,30.7436446738237,-8.72718501437767));
#7569=CARTESIAN_POINT('Ctrl Pts',(8.69225549345207,30.7547919800708,-8.5242679853787));
#7570=CARTESIAN_POINT('Ctrl Pts',(8.89121712575945,30.7659373929494,-8.32138542181121));
#7571=CARTESIAN_POINT('Ctrl Pts',(9.08309388979978,30.7770828058279,-8.11151222901553));
#7572=CARTESIAN_POINT('Ctrl Pts',(9.26740381715853,30.7882282187065,-7.89516793613129));
#7573=CARTESIAN_POINT('Ctrl Pts',(9.45169328325129,30.799372394271,-7.67884766082539));
#7574=CARTESIAN_POINT('Ctrl Pts',(9.62841741714045,30.8105165698356,-7.45605792294662));
#7575=CARTESIAN_POINT('Ctrl Pts',(9.79713372166527,30.8216607454001,-7.22735228765066));
#7576=CARTESIAN_POINT('Ctrl Pts',(9.97116324537299,30.833155873693,-6.99144424727527));
#7577=CARTESIAN_POINT('Ctrl Pts',(10.1366722171862,30.8446510019859,-6.74924189735682));
#7578=CARTESIAN_POINT('Ctrl Pts',(10.2932216574201,30.8561461302788,-6.50138740279476));
#7579=CARTESIAN_POINT('Ctrl Pts',(10.4449996662147,30.8672909014164,-6.26108720370593));
#7580=CARTESIAN_POINT('Ctrl Pts',(10.5883560576881,30.878435672554,-6.0154745345967));
#7581=CARTESIAN_POINT('Ctrl Pts',(10.7229356202183,30.8895804436917,-5.76516278474886));
#7582=CARTESIAN_POINT('Ctrl Pts',(10.863861330924,30.9012507505621,-5.50304749337706));
#7583=CARTESIAN_POINT('Ctrl Pts',(10.9951623959182,30.9129210574326,-5.23577956394943));
#7584=CARTESIAN_POINT('Ctrl Pts',(11.1164852149522,30.9245913643031,-4.96409173119816));
#7585=CARTESIAN_POINT('Ctrl Pts',(11.2378080339862,30.9362616711736,-4.69240389844691));
#7586=CARTESIAN_POINT('Ctrl Pts',(11.3491524782764,30.9479319780441,-4.41629647229572));
#7587=CARTESIAN_POINT('Ctrl Pts',(11.4502225594297,30.9596022849146,-4.13652675435896));
#7588=CARTESIAN_POINT('Ctrl Pts',(11.5467632210884,30.9707495911617,-3.86929481614853));
#7589=CARTESIAN_POINT('Ctrl Pts',(11.6339589947617,30.9818968974088,-3.59864180777725));
#7590=CARTESIAN_POINT('Ctrl Pts',(11.7115853118451,30.993044203656,-3.32523980088261));
#7591=CARTESIAN_POINT('Ctrl Pts',(11.7891984441082,31.0041896165345,-3.05188423128495));
#7592=CARTESIAN_POINT('Ctrl Pts',(11.8572452920049,31.015335029413,-2.77578085187103));
#7593=CARTESIAN_POINT('Ctrl Pts',(11.9155512731645,31.0264804422916,-2.49761648508908));
#7594=CARTESIAN_POINT('Ctrl Pts',(11.9738507814546,31.0376246178562,-2.21948299887197));
#7595=CARTESIAN_POINT('Ctrl Pts',(12.022411527657,31.0487687934208,-1.9392892431739));
#7596=CARTESIAN_POINT('Ctrl Pts',(12.0611098753863,31.0599129689854,-1.65773303757252));
#7597=CARTESIAN_POINT('Ctrl Pts',(12.1010269127024,31.0714080972782,-1.36731005506706));
#7598=CARTESIAN_POINT('Ctrl Pts',(12.1304502618443,31.0829032255711,-1.07543771211255));
#7599=CARTESIAN_POINT('Ctrl Pts',(12.1493017737572,31.094398353864,-0.782889941294685));
#7600=CARTESIAN_POINT('Ctrl Pts',(12.1675787151288,31.1055431250016,-0.499258661197821));
#7601=CARTESIAN_POINT('Ctrl Pts',(12.17591869138,31.1166878961392,-0.214992794448297));
#7602=CARTESIAN_POINT('Ctrl Pts',(12.1743033368384,31.1278326672768,0.069199079805505));
#7603=CARTESIAN_POINT('Ctrl Pts',(12.1726118096663,31.1395029741473,0.366792125161997));
#7604=CARTESIAN_POINT('Ctrl Pts',(12.1600034675358,31.1511732810177,0.664303713974559));
#7605=CARTESIAN_POINT('Ctrl Pts',(12.136518471558,31.1628435878882,0.960921245228644));
#7606=CARTESIAN_POINT('Ctrl Pts',(12.1130334755802,31.1745138947587,1.25753877648276));
#7607=CARTESIAN_POINT('Ctrl Pts',(12.0786718609865,31.1861842016292,1.55326191641704));
#7608=CARTESIAN_POINT('Ctrl Pts',(12.0335361321028,31.1978545084997,1.84728406244831));
#7609=CARTESIAN_POINT('Ctrl Pts',(11.9904231447464,31.2090018147468,2.12812971129163));
#7610=CARTESIAN_POINT('Ctrl Pts',(11.9374676168789,31.2201491209939,2.40750735169076));
#7611=CARTESIAN_POINT('Ctrl Pts',(11.8747939778081,31.231296427241,2.68471939587967));
#7612=CARTESIAN_POINT('Ctrl Pts',(11.8121309838468,31.2424418401196,2.96188435563876));
#7613=CARTESIAN_POINT('Ctrl Pts',(11.7397532329452,31.2535872529982,3.2368841934707));
#7614=CARTESIAN_POINT('Ctrl Pts',(11.6578361044304,31.2647326658768,3.50903228999679));
#7615=CARTESIAN_POINT('Ctrl Pts',(11.5759280699893,31.2758768414414,3.7811501738566));
#7616=CARTESIAN_POINT('Ctrl Pts',(11.4844828494922,31.287021017006,4.0504166932242));
#7617=CARTESIAN_POINT('Ctrl Pts',(11.383725818712,31.2981651925706,4.31615995236384));
#7618=CARTESIAN_POINT('Ctrl Pts',(11.2797957443419,31.3096603208635,4.59027200659853));
#7619=CARTESIAN_POINT('Ctrl Pts',(11.1659579563437,31.3211554491563,4.8606350145712));
#7620=CARTESIAN_POINT('Ctrl Pts',(11.0425141946155,31.3326505774492,5.12653201606268));
#7621=CARTESIAN_POINT('Ctrl Pts',(10.922832844588,31.3437953485868,5.38432480900107));
#7622=CARTESIAN_POINT('Ctrl Pts',(10.7941225236154,31.3549401197244,5.63791954766483));
#7623=CARTESIAN_POINT('Ctrl Pts',(10.6567061908373,31.366084890862,5.88668526525489));
#7624=CARTESIAN_POINT('Ctrl Pts',(10.5128099409518,31.3777551977325,6.14718162065625));
#7625=CARTESIAN_POINT('Ctrl Pts',(10.3593670062242,31.3894255046029,6.40238228983842));
#7626=CARTESIAN_POINT('Ctrl Pts',(10.1968015149776,31.4010958114734,6.65159297568257));
#7627=CARTESIAN_POINT('Ctrl Pts',(10.0342360237311,31.4127661183439,6.90080366152668));
#7628=CARTESIAN_POINT('Ctrl Pts',(9.86254816662018,31.4244364252143,7.14402408782862));
#7629=CARTESIAN_POINT('Ctrl Pts',(9.68221394281234,31.4361067320848,7.38059505836828));
#7630=CARTESIAN_POINT('Ctrl Pts',(9.50996133266801,31.4472540383319,7.60656418557765));
#7631=CARTESIAN_POINT('Ctrl Pts',(9.32976884399584,31.4584013445791,7.82653423106822));
#7632=CARTESIAN_POINT('Ctrl Pts',(9.1420795592616,31.4695486508262,8.0399522126771));
#7633=CARTESIAN_POINT('Ctrl Pts',(8.95442215352886,31.4806940637047,8.25333394526852));
#7634=CARTESIAN_POINT('Ctrl Pts',(8.75927067002798,31.4918394765833,8.4601656355874));
#7635=CARTESIAN_POINT('Ctrl Pts',(8.557107679775,31.5029848894619,8.65992831417996));
#7636=CARTESIAN_POINT('Ctrl Pts',(8.35496713275467,31.5141290650264,8.85966881601174));
#7637=CARTESIAN_POINT('Ctrl Pts',(8.14581682298889,31.525273240591,9.05234168573748));
#7638=CARTESIAN_POINT('Ctrl Pts',(7.93017617569519,31.5364174161556,9.23746480764265));
#7639=CARTESIAN_POINT('Ctrl Pts',(7.70774456633725,31.5479125444485,9.42841783274024));
#7640=CARTESIAN_POINT('Ctrl Pts',(7.47840742626827,31.5594076727413,9.61133769016819));
#7641=CARTESIAN_POINT('Ctrl Pts',(7.24277279859588,31.5709028010342,9.78573923819348));
#7642=CARTESIAN_POINT('Ctrl Pts',(7.01432002011553,31.5820475721717,9.95482524482681));
#7643=CARTESIAN_POINT('Ctrl Pts',(6.7799481729941,31.5931923433093,10.1159043417915));
#7644=CARTESIAN_POINT('Ctrl Pts',(6.54024278067394,31.6043371144468,10.2685770494184));
#7645=CARTESIAN_POINT('Ctrl Pts',(6.28923399347095,31.6160074213174,10.4284490940541));
#7646=CARTESIAN_POINT('Ctrl Pts',(6.03237681530382,31.6276777281879,10.5791026894094));
#7647=CARTESIAN_POINT('Ctrl Pts',(5.77037590892342,31.6393480350584,10.7201311614978));
#7648=CARTESIAN_POINT('Ctrl Pts',(5.50837500254302,31.6510183419289,10.8611596335862));
#7649=CARTESIAN_POINT('Ctrl Pts',(5.24123066753183,31.6626886487994,10.9925628311192));
#7650=CARTESIAN_POINT('Ctrl Pts',(4.96967631529749,31.6743589556699,11.1139897233699));
#7651=CARTESIAN_POINT('Ctrl Pts',(4.70170325855833,31.6858753529563,11.2338152213559));
#7652=CARTESIAN_POINT('Ctrl Pts',(4.429353113389,31.6973917502427,11.3439629082076));
#7653=CARTESIAN_POINT('Ctrl Pts',(4.15334703314022,31.708908147529,11.4441320628655));
#7654=CARTESIAN_POINT('Ctrl Pts',(3.88623292576372,31.7200535258431,11.5410741096094));
#7655=CARTESIAN_POINT('Ctrl Pts',(3.61569501806569,31.7311989041571,11.628670387502));
#7656=CARTESIAN_POINT('Ctrl Pts',(3.34240593741423,31.7423442824711,11.7066977751857));
#7657=CARTESIAN_POINT('Ctrl Pts',(3.0554705590327,31.7540461892436,11.7886213484063));
#7658=CARTESIAN_POINT('Ctrl Pts',(2.76550256063917,31.7657480960162,11.8599959936606));
#7659=CARTESIAN_POINT('Ctrl Pts',(2.47329796532737,31.7774500027887,11.9206227783916));
#7660=CARTESIAN_POINT('Ctrl Pts',(2.18109337001554,31.7891519095613,11.9812495631225));
#7661=CARTESIAN_POINT('Ctrl Pts',(1.88665251084213,31.8008538163338,12.0311284164936));
#7662=CARTESIAN_POINT('Ctrl Pts',(1.59078448392773,31.8125557231064,12.0701224093086));
#7663=CARTESIAN_POINT('Origin',(0.,13.3748739960349,0.));
#7664=CARTESIAN_POINT('',(1.59078448392775,35.0623145891265,12.0701224093086));
#7665=CARTESIAN_POINT('',(1.59078448392778,34.8125669141531,12.0701224093086));
#7666=CARTESIAN_POINT('',(1.59078448392774,13.3748739960349,12.0701224093086));
#7667=CARTESIAN_POINT('',(-12.1744999985554,32.8748739960349,0.000187550598588881));
#7668=CARTESIAN_POINT('Ctrl Pts',(-12.1744999985554,32.8748739960349,0.000187550598588881));
#7669=CARTESIAN_POINT('Ctrl Pts',(-12.1745043615588,32.8859843814439,-0.283028740965722));
#7670=CARTESIAN_POINT('Ctrl Pts',(-12.1646216592697,32.8970947668528,-0.566289459754149));
#7671=CARTESIAN_POINT('Ctrl Pts',(-12.1448686657604,32.9082051522618,-0.848890653400877));
#7672=CARTESIAN_POINT('Ctrl Pts',(-12.125118898305,32.9193137231254,-1.13144569269124));
#7673=CARTESIAN_POINT('Ctrl Pts',(-12.0955020767017,32.930422293989,-1.4133411523803));
#7674=CARTESIAN_POINT('Ctrl Pts',(-12.0560869992745,32.9415308648526,-1.69387618081272));
#7675=CARTESIAN_POINT('Ctrl Pts',(-12.0166757019596,32.9526383703461,-1.97438430446705));
#7676=CARTESIAN_POINT('Ctrl Pts',(-11.9674680629165,32.9637458758396,-2.2535319898437));
#7677=CARTESIAN_POINT('Ctrl Pts',(-11.9085845275246,32.9748533813331,-2.5306253774118));
#7678=CARTESIAN_POINT('Ctrl Pts',(-11.849696245945,32.9859617821245,-2.80774109952985));
#7679=CARTESIAN_POINT('Ctrl Pts',(-11.7811305632598,32.9970701829159,-3.08280192803896));
#7680=CARTESIAN_POINT('Ctrl Pts',(-11.703058959395,33.0081785837073,-3.35512462405274));
#7681=CARTESIAN_POINT('Ctrl Pts',(-11.6249866141567,33.0192870899849,-3.62744990606199));
#7682=CARTESIAN_POINT('Ctrl Pts',(-11.5374082443903,33.0303955962625,-3.89703674452342));
#7683=CARTESIAN_POINT('Ctrl Pts',(-11.4405453455313,33.0415041025401,-4.16321659859816));
#7684=CARTESIAN_POINT('Ctrl Pts',(-11.3436617578851,33.0526149814652,-4.4294533055898));
#7685=CARTESIAN_POINT('Ctrl Pts',(-11.2374897710976,33.0637258603903,-4.6922813200952));
#7686=CARTESIAN_POINT('Ctrl Pts',(-11.1222997533272,33.0748367393155,-4.95105023678181));
#7687=CARTESIAN_POINT('Ctrl Pts',(-11.067529982669,33.0801196648877,-5.07408793132099));
#7688=CARTESIAN_POINT('Ctrl Pts',(-11.0107221639337,33.0854025904599,-5.19620826044135));
#7689=CARTESIAN_POINT('Ctrl Pts',(-10.9519091180938,33.0906855160321,-5.31734303191104));
#7690=CARTESIAN_POINT('Ctrl Pts',(-10.8278098809659,33.1018328222794,-5.5729450418798));
#7691=CARTESIAN_POINT('Ctrl Pts',(-10.6947401199187,33.1129801285267,-5.82423887901939));
#7692=CARTESIAN_POINT('Ctrl Pts',(-10.5530246517763,33.124127434774,-6.07059477720272));
#7693=CARTESIAN_POINT('Ctrl Pts',(-10.4113332539878,33.1352728476528,-6.31690883186865));
#7694=CARTESIAN_POINT('Ctrl Pts',(-10.2609992138668,33.1464182605315,-6.55828639092668));
#7695=CARTESIAN_POINT('Ctrl Pts',(-10.1023927896335,33.1575636734103,-6.7941232086239));
#7696=CARTESIAN_POINT('Ctrl Pts',(-9.94380397317836,33.168707848975,-7.02993384476881));
#7697=CARTESIAN_POINT('Ctrl Pts',(-9.77694475525955,33.1798520245398,-7.26020474653669));
#7698=CARTESIAN_POINT('Ctrl Pts',(-9.60222881583929,33.1909962001045,-7.48436049494315));
#7699=CARTESIAN_POINT('Ctrl Pts',(-9.42201071655001,33.2024913283972,-7.71557536324092));
#7700=CARTESIAN_POINT('Ctrl Pts',(-9.2334332035449,33.21398645669,-7.94028343973844));
#7701=CARTESIAN_POINT('Ctrl Pts',(-9.03699622097056,33.2254815849827,-8.15788879258377));
#7702=CARTESIAN_POINT('Ctrl Pts',(-8.84654639230963,33.2366263561204,-8.36886180602542));
#7703=CARTESIAN_POINT('Ctrl Pts',(-8.64870928031278,33.2477711272582,-8.57315844163609));
#7704=CARTESIAN_POINT('Ctrl Pts',(-8.44397971682008,33.258915898396,-8.77027119261035));
#7705=CARTESIAN_POINT('Ctrl Pts',(-8.22959605637275,33.2705862052662,-8.97667886697739));
#7706=CARTESIAN_POINT('Ctrl Pts',(-8.00765450035677,33.2822565121364,-9.1752086165817));
#7707=CARTESIAN_POINT('Ctrl Pts',(-7.77876523658056,33.2939268190066,-9.36532229259441));
#7708=CARTESIAN_POINT('Ctrl Pts',(-7.54987597280433,33.3055971258768,-9.55543596860713));
#7709=CARTESIAN_POINT('Ctrl Pts',(-7.31403926496306,33.317267432747,-9.73713336341621));
#7710=CARTESIAN_POINT('Ctrl Pts',(-7.07190449795741,33.3289377396172,-9.90992517740522));
#7711=CARTESIAN_POINT('Ctrl Pts',(-6.8406209138327,33.3400850458639,-10.0749733881227));
#7712=CARTESIAN_POINT('Ctrl Pts',(-6.60352227774398,33.3512323521105,-10.2319459674008));
#7713=CARTESIAN_POINT('Ctrl Pts',(-6.36119516972689,33.3623796583572,-10.3804453788189));
#7714=CARTESIAN_POINT('Ctrl Pts',(-6.1189092209383,33.3735250712353,-10.5289195676309));
#7715=CARTESIAN_POINT('Ctrl Pts',(-5.87139680057618,33.3846704841134,-10.6689233225553));
#7716=CARTESIAN_POINT('Ctrl Pts',(-5.61927217655415,33.3958158969915,-10.8001032613491));
#7717=CARTESIAN_POINT('Ctrl Pts',(-5.36717554228243,33.4069600725556,-10.9312686371318));
#7718=CARTESIAN_POINT('Ctrl Pts',(-5.11046796335894,33.4181042481198,-11.0536120297623));
#7719=CARTESIAN_POINT('Ctrl Pts',(-4.84978803993833,33.4292484236839,-11.1668261479111));
#7720=CARTESIAN_POINT('Ctrl Pts',(-4.58089877613062,33.4407435519771,-11.2836056086468));
#7721=CARTESIAN_POINT('Ctrl Pts',(-4.30778318746436,33.4522386802703,-11.3906713514839));
#7722=CARTESIAN_POINT('Ctrl Pts',(-4.03116543587642,33.4637338085635,-11.4877393545726));
#7723=CARTESIAN_POINT('Ctrl Pts',(-3.76297864793515,33.4748785797007,-11.5818488461391));
#7724=CARTESIAN_POINT('Ctrl Pts',(-3.49150028225666,33.4860233508378,-11.6665609182723));
#7725=CARTESIAN_POINT('Ctrl Pts',(-3.2174076966831,33.497168121975,-11.7416667455402));
#7726=CARTESIAN_POINT('Ctrl Pts',(-2.9303901756055,33.5088384288462,-11.8203142153935));
#7727=CARTESIAN_POINT('Ctrl Pts',(-2.64050625979877,33.5205087357174,-11.8884275851291));
#7728=CARTESIAN_POINT('Ctrl Pts',(-2.34854926057755,33.5321790425887,-11.9458263264054));
#7729=CARTESIAN_POINT('Ctrl Pts',(-2.05659226135631,33.5438493494599,-12.0032250676818));
#7730=CARTESIAN_POINT('Ctrl Pts',(-1.7625625096131,33.5555196563311,-12.0499091243916));
#7731=CARTESIAN_POINT('Ctrl Pts',(-1.46726435779509,33.5671899632023,-12.0857596184247));
#7732=CARTESIAN_POINT('Ctrl Pts',(-1.18519988690535,33.5783372694502,-12.1200034854056));
#7733=CARTESIAN_POINT('Ctrl Pts',(-0.901893961090877,33.5894845756981,-12.1443736781868));
#7734=CARTESIAN_POINT('Ctrl Pts',(-0.618051873482272,33.600631881946,-12.1588018378328));
#7735=CARTESIAN_POINT('Ctrl Pts',(-0.334257996414995,33.6117772948253,-12.1732275468577));
#7736=CARTESIAN_POINT('Ctrl Pts',(-0.0499284056711118,33.6229227077047,
-12.1777145806061));
#7737=CARTESIAN_POINT('Ctrl Pts',(0.234228423541575,33.6340681205841,-12.1722466001805));
#7738=CARTESIAN_POINT('Ctrl Pts',(0.518353706932561,33.6452122961495,-12.1667792267857));
#7739=CARTESIAN_POINT('Ctrl Pts',(0.802306000460723,33.656356471715,-12.1513590511788));
#7740=CARTESIAN_POINT('Ctrl Pts',(1.08537752011688,33.6675006472804,-12.1260218492639));
#7741=CARTESIAN_POINT('Ctrl Pts',(1.37736353695788,33.6789957755727,-12.0998867273907));
#7742=CARTESIAN_POINT('Ctrl Pts',(1.66841210987824,33.6904909038649,-12.0631998598761));
#7743=CARTESIAN_POINT('Ctrl Pts',(1.95775146156407,33.7019860321572,-12.0160583996893));
#7744=CARTESIAN_POINT('Ctrl Pts',(2.23827211117223,33.7131308032956,-11.9703537523331));
#7745=CARTESIAN_POINT('Ctrl Pts',(2.5171859111229,33.7242755744339,-11.91482240613));
#7746=CARTESIAN_POINT('Ctrl Pts',(2.79379816580269,33.7354203455723,-11.84960514358));
#7747=CARTESIAN_POINT('Ctrl Pts',(3.08345417181668,33.7470906524415,-11.7813125373277));
#7748=CARTESIAN_POINT('Ctrl Pts',(3.37058603991502,33.7587609593107,-11.7023986217524));
#7749=CARTESIAN_POINT('Ctrl Pts',(3.65441080124873,33.7704312661799,-11.6130845147065));
#7750=CARTESIAN_POINT('Ctrl Pts',(3.93823556258241,33.782101573049,-11.5237704076606));
#7751=CARTESIAN_POINT('Ctrl Pts',(4.21875289975679,33.7937718799182,-11.4240562182245));
#7752=CARTESIAN_POINT('Ctrl Pts',(4.49519965136699,33.8054421867874,-11.3142224807695));
#7753=CARTESIAN_POINT('Ctrl Pts',(4.75925754080382,33.8165894930335,-11.2093109029254));
#7754=CARTESIAN_POINT('Ctrl Pts',(5.01968053272849,33.8277367992797,-11.0951355152522));
#7755=CARTESIAN_POINT('Ctrl Pts',(5.27581662176582,33.8388841055259,-10.9719738070914));
#7756=CARTESIAN_POINT('Ctrl Pts',(5.53190920612139,33.8500295184035,-10.8488330179308));
#7757=CARTESIAN_POINT('Ctrl Pts',(5.78371610099243,33.8611749312811,-10.7167090711419));
#7758=CARTESIAN_POINT('Ctrl Pts',(6.03060740074508,33.8723203441587,-10.575926655763));
#7759=CARTESIAN_POINT('Ctrl Pts',(6.27747129172809,33.8834645197224,-10.4351598694193));
#7760=CARTESIAN_POINT('Ctrl Pts',(6.51942044562115,33.894608695286,-10.2857366659969));
#7761=CARTESIAN_POINT('Ctrl Pts',(6.75585050286505,33.9057528708497,-10.1280271639119));
#7762=CARTESIAN_POINT('Ctrl Pts',(6.9997262229621,33.9172479991433,-9.96535106919086));
#7763=CARTESIAN_POINT('Ctrl Pts',(7.23772934615604,33.9287431274368,-9.79385847046579));
#7764=CARTESIAN_POINT('Ctrl Pts',(7.46922869419891,33.9402382557304,-9.61400400269085));
#7765=CARTESIAN_POINT('Ctrl Pts',(7.69367223117651,33.951383026867,-9.4396312745173));
#7766=CARTESIAN_POINT('Ctrl Pts',(7.91200235583995,33.9625277980037,-9.25739901926732));
#7767=CARTESIAN_POINT('Ctrl Pts',(8.12367645122317,33.9736725691403,-9.06776329454195));
#7768=CARTESIAN_POINT('Ctrl Pts',(8.3453321155427,33.9853428760124,-8.86918522826218));
#7769=CARTESIAN_POINT('Ctrl Pts',(8.55968867444274,33.9970131828844,-8.66248887742566));
#7770=CARTESIAN_POINT('Ctrl Pts',(8.76616444527815,34.0086834897564,-8.44824308175026));
#7771=CARTESIAN_POINT('Ctrl Pts',(8.97264021611356,34.0203537966285,-8.23399728607487));
#7772=CARTESIAN_POINT('Ctrl Pts',(9.17123497239103,34.0320241035005,-8.01220229322709));
#7773=CARTESIAN_POINT('Ctrl Pts',(9.36141285701635,34.0436944103725,-7.78346963574016));
#7774=CARTESIAN_POINT('Ctrl Pts',(9.54306798782396,34.0548417166199,-7.56498755041451));
#7775=CARTESIAN_POINT('Ctrl Pts',(9.71709831636459,34.0659890228673,-7.34011069825151));
#7776=CARTESIAN_POINT('Ctrl Pts',(9.88306413050669,34.0771363291148,-7.10939474514478));
#7777=CARTESIAN_POINT('Ctrl Pts',(10.049001755376,34.0882817419936,-6.87871797911381));
#7778=CARTESIAN_POINT('Ctrl Pts',(10.2068774448557,34.0994271548725,-6.64220430866783));
#7779=CARTESIAN_POINT('Ctrl Pts',(10.3562934788784,34.1105725677513,-6.40044026839876));
#7780=CARTESIAN_POINT('Ctrl Pts',(10.5056929254003,34.1217167433162,-6.15870306769375));
#7781=CARTESIAN_POINT('Ctrl Pts',(10.6466344516049,34.1328609188811,-5.91171688792114));
#7782=CARTESIAN_POINT('Ctrl Pts',(10.7787645084178,34.1440050944459,-5.66009592869888));
#7783=CARTESIAN_POINT('Ctrl Pts',(10.9150556091398,34.1555002227386,-5.40055091430656));
#7784=CARTESIAN_POINT('Ctrl Pts',(11.04197111863,34.1669953510312,-5.13607473106159));
#7785=CARTESIAN_POINT('Ctrl Pts',(11.1591743840538,34.1784904793238,-4.86736862342257));
#7786=CARTESIAN_POINT('Ctrl Pts',(11.2728054403158,34.1896352504617,-4.60685234237289));
#7787=CARTESIAN_POINT('Ctrl Pts',(11.3773074082572,34.2007800215996,-4.34236042018421));
#7788=CARTESIAN_POINT('Ctrl Pts',(11.4724220783389,34.2119247927375,-4.07455297013576));
#7789=CARTESIAN_POINT('Ctrl Pts',(11.5720219152455,34.2235950996075,-3.79411696248015));
#7790=CARTESIAN_POINT('Ctrl Pts',(11.6613277225691,34.2352654064775,-3.5100455127702));
#7791=CARTESIAN_POINT('Ctrl Pts',(11.7401009596523,34.2469357133476,-3.2231164588285));
#7792=CARTESIAN_POINT('Ctrl Pts',(11.8188741967355,34.2586060202176,-2.93618740488681));
#7793=CARTESIAN_POINT('Ctrl Pts',(11.8871147832217,34.2702763270876,-2.64640107256719));
#7794=CARTESIAN_POINT('Ctrl Pts',(11.9446448465681,34.2819466339576,-2.35455085724545));
#7795=CARTESIAN_POINT('Ctrl Pts',(11.9995967207427,34.2930939402076,-2.07577980473253));
#7796=CARTESIAN_POINT('Ctrl Pts',(12.0447933593859,34.3042412464575,-1.79504252936051));
#7797=CARTESIAN_POINT('Ctrl Pts',(12.0801145768396,34.3153885527074,-1.51303736253506));
#7798=CARTESIAN_POINT('Ctrl Pts',(12.1154297949892,34.3265339655889,-1.23108009425072));
#7799=CARTESIAN_POINT('Ctrl Pts',(12.1408729076176,34.3376793784703,-0.947855629040423));
#7800=CARTESIAN_POINT('Ctrl Pts',(12.1563753727891,34.3488247913517,-0.664069308015263));
#7801=CARTESIAN_POINT('Ctrl Pts',(12.1718761169461,34.3599689669192,-0.380314491679434));
#7802=CARTESIAN_POINT('Ctrl Pts',(12.1774384027462,34.3711131424867,-0.0959982103629502));
#7803=CARTESIAN_POINT('Ctrl Pts',(12.1730457121208,34.3822573180542,0.188171040858175));
#7804=CARTESIAN_POINT('Ctrl Pts',(12.1685146867457,34.3937524463449,0.481289358968064));
#7805=CARTESIAN_POINT('Ctrl Pts',(12.1533915147295,34.4052475746356,0.774250939540593));
#7806=CARTESIAN_POINT('Ctrl Pts',(12.1277161686617,34.4167427029263,1.06627894210765));
#7807=CARTESIAN_POINT('Ctrl Pts',(12.1028233750677,34.4278874740667,1.34940629596561));
#7808=CARTESIAN_POINT('Ctrl Pts',(12.0680121410407,34.4390322452072,1.63165585970076));
#7809=CARTESIAN_POINT('Ctrl Pts',(12.0233716344006,34.4501770163476,1.91232444713011));
#7810=CARTESIAN_POINT('Ctrl Pts',(11.9766260884783,34.4618473232134,2.20622806360036));
#7811=CARTESIAN_POINT('Ctrl Pts',(11.9191020086131,34.4735176300793,2.49839769914427));
#7812=CARTESIAN_POINT('Ctrl Pts',(11.8509621693877,34.4851879369452,2.78803621026358));
#7813=CARTESIAN_POINT('Ctrl Pts',(11.7828223301624,34.496858243811,3.07767472138287));
#7814=CARTESIAN_POINT('Ctrl Pts',(11.7040668169537,34.5085285506769,3.36478178350285));
#7815=CARTESIAN_POINT('Ctrl Pts',(11.6149191198025,34.5201988575427,3.64857562487699));
#7816=CARTESIAN_POINT('Ctrl Pts',(11.5297665448279,34.5313461637786,3.91965134670903));
#7817=CARTESIAN_POINT('Ctrl Pts',(11.4351073244025,34.5424934700145,4.18778524183307));
#7818=CARTESIAN_POINT('Ctrl Pts',(11.3311701091902,34.5536407762504,4.45230661641746));
#7819=CARTESIAN_POINT('Ctrl Pts',(11.2272505477016,34.5647861891177,4.71678306207768));
#7820=CARTESIAN_POINT('Ctrl Pts',(11.1140562351574,34.575931601985,4.97764796404744));
#7821=CARTESIAN_POINT('Ctrl Pts',(10.9918645231726,34.5870770148522,5.2342491872493));
#7822=CARTESIAN_POINT('Ctrl Pts',(10.8696863763659,34.5982211904055,5.49082192372942));
#7823=CARTESIAN_POINT('Ctrl Pts',(10.7385129393202,34.6093653659588,5.743131685842));
#7824=CARTESIAN_POINT('Ctrl Pts',(10.5986687532571,34.6205095415121,5.99054846476783));
#7825=CARTESIAN_POINT('Ctrl Pts',(10.4544205894249,34.6320046698134,6.24575690114288));
#7826=CARTESIAN_POINT('Ctrl Pts',(10.3009468455545,34.6434997981147,6.49575891739394));
#7827=CARTESIAN_POINT('Ctrl Pts',(10.1386543714878,34.6549949264161,6.73989152624218));
#7828=CARTESIAN_POINT('Ctrl Pts',(9.98130836963331,34.6661396975425,6.97658327763416));
#7829=CARTESIAN_POINT('Ctrl Pts',(9.81567339958986,34.6772844686689,7.20775787559392));
#7830=CARTESIAN_POINT('Ctrl Pts',(9.64216426105065,34.6884292397953,7.43284054806221));
#7831=CARTESIAN_POINT('Ctrl Pts',(9.46047323556585,34.7000995466841,7.66853707634841));
#7832=CARTESIAN_POINT('Ctrl Pts',(9.27014774830922,34.7117698535728,7.89755306912699));
#7833=CARTESIAN_POINT('Ctrl Pts',(9.07171219303635,34.7234401604616,8.11926647775005));
#7834=CARTESIAN_POINT('Ctrl Pts',(8.87327663776348,34.7351104673503,8.3409798863731));
#7835=CARTESIAN_POINT('Ctrl Pts',(8.66673124476339,34.7467807742391,8.55539046669953));
#7836=CARTESIAN_POINT('Ctrl Pts',(8.45264636382744,34.7584510811278,8.76191872240749));
#7837=CARTESIAN_POINT('Ctrl Pts',(8.24815561997432,34.769598387403,8.95919148847938));
#7838=CARTESIAN_POINT('Ctrl Pts',(8.03672521997992,34.7807456936781,9.14933180573395));
#7839=CARTESIAN_POINT('Ctrl Pts',(7.81887688946857,34.7918929999533,9.33186018097862));
#7840=CARTESIAN_POINT('Ctrl Pts',(7.60106556046604,34.80303841286,9.514357553804));
#7841=CARTESIAN_POINT('Ctrl Pts',(7.37683868168676,34.8141838257667,9.68924539461946));
#7842=CARTESIAN_POINT('Ctrl Pts',(7.14675186016405,34.8253292386734,9.85608381149641));
#7843=CARTESIAN_POINT('Ctrl Pts',(6.91669058185407,34.8364734142661,10.0229037067164));
#7844=CARTESIAN_POINT('Ctrl Pts',(6.68077087572966,34.8476175898588,10.1816758058499));
#7845=CARTESIAN_POINT('Ctrl Pts',(6.43957919597263,34.8587617654515,10.332002227487));
#7846=CARTESIAN_POINT('Ctrl Pts',(6.19079190131524,34.8702568937233,10.4870627328589));
#7847=CARTESIAN_POINT('Ctrl Pts',(5.93639544874949,34.8817520219951,10.6331368327251));
#7848=CARTESIAN_POINT('Ctrl Pts',(5.67706434630601,34.8932471502669,10.7698370766647));
#7849=CARTESIAN_POINT('Ctrl Pts',(5.4256373309246,34.9043919214323,10.9023708684537));
#7850=CARTESIAN_POINT('Ctrl Pts',(5.16957226213629,34.9155366925976,11.0260936195786));
#7851=CARTESIAN_POINT('Ctrl Pts',(4.90950841371425,34.926681463763,11.1406991425884));
#7852=CARTESIAN_POINT('Ctrl Pts',(4.63718116175636,34.938351770588,11.2607089299149));
#7853=CARTESIAN_POINT('Ctrl Pts',(4.36046921890012,34.950022077413,11.3707208190695));
#7854=CARTESIAN_POINT('Ctrl Pts',(4.08013071339716,34.961692384238,11.4704395561632));
#7855=CARTESIAN_POINT('Ctrl Pts',(3.79979220789422,34.9733626910629,11.5701582932569));
#7856=CARTESIAN_POINT('Ctrl Pts',(3.51582745878504,34.9850329978879,11.6595837741214));
#7857=CARTESIAN_POINT('Ctrl Pts',(3.22901458356905,34.9967033047129,11.7384801004686));
#7858=CARTESIAN_POINT('Ctrl Pts',(2.95505255715356,35.007850715387,11.8138414224685));
#7859=CARTESIAN_POINT('Ctrl Pts',(2.6784101976567,35.0189981260611,11.8796188945309));
#7860=CARTESIAN_POINT('Ctrl Pts',(2.39977509106479,35.0301455367353,11.9356411542198));
#7861=CARTESIAN_POINT('Ctrl Pts',(2.13174790508044,35.040868554199,11.9895305897635));
#7862=CARTESIAN_POINT('Ctrl Pts',(1.86187710718966,35.0515915716628,12.0343936963621));
#7863=CARTESIAN_POINT('Ctrl Pts',(1.59078448392775,35.0623145891265,12.0701224093086));
#7864=CARTESIAN_POINT('Ctrl Pts',(1.59071714630986,32.0622959365534,12.0696162300787));
#7865=CARTESIAN_POINT('Ctrl Pts',(0.955528524672293,32.0874228315995,12.1538996540835));
#7866=CARTESIAN_POINT('Ctrl Pts',(-1.71425060518447,32.1919671345073,12.2972187210211));
#7867=CARTESIAN_POINT('Ctrl Pts',(-6.36996413642198,32.3759288452768,10.9770241092494));
#7868=CARTESIAN_POINT('Ctrl Pts',(-10.8462127664019,32.6141810688619,6.59023292610109));
#7869=CARTESIAN_POINT('Ctrl Pts',(-12.1244826930503,32.7804961191146,2.40607098746999));
#7870=CARTESIAN_POINT('Ctrl Pts',(-12.1754508005637,32.8673937615056,0.190879886591904));
#7871=CARTESIAN_POINT('Ctrl Pts',(-12.175309711376,32.8748739960349,0.000187563072374733));
#7872=CARTESIAN_POINT('',(-12.1744999999831,32.6251260039388,-2.02629457301205E-5));
#7873=CARTESIAN_POINT('Ctrl Pts',(1.59078448392773,31.8125557231064,12.0701224093086));
#7874=CARTESIAN_POINT('Ctrl Pts',(1.30900267453901,31.8237005044403,12.1072599059328));
#7875=CARTESIAN_POINT('Ctrl Pts',(1.02592669881683,31.8348452857743,12.1345247267504));
#7876=CARTESIAN_POINT('Ctrl Pts',(0.742262345110562,31.8459900671082,12.1518515815916));
#7877=CARTESIAN_POINT('Ctrl Pts',(0.458530536541289,31.8571374986507,12.1691825567272));
#7878=CARTESIAN_POINT('Ctrl Pts',(0.174210336700322,31.8682849301933,12.1765708248781));
#7879=CARTESIAN_POINT('Ctrl Pts',(-0.109989332035699,31.8794323617358,12.1740031459187));
#7880=CARTESIAN_POINT('Ctrl Pts',(-0.391949916769597,31.8904919675755,12.1714556965708));
#7881=CARTESIAN_POINT('Ctrl Pts',(-0.673791604467417,31.9015515734153,12.1591086355011));
#7882=CARTESIAN_POINT('Ctrl Pts',(-0.95482342212009,31.912611179255,12.1369997315058));
#7883=CARTESIAN_POINT('Ctrl Pts',(-1.23808376448244,31.9237584855021,12.1147155084335));
#7884=CARTESIAN_POINT('Ctrl Pts',(-1.52060594814084,31.9349057917492,12.0825072854502));
#7885=CARTESIAN_POINT('Ctrl Pts',(-1.80168510862511,31.9460530979963,12.0404477084267));
#7886=CARTESIAN_POINT('Ctrl Pts',(-2.08271652784791,31.9571985108748,11.9983952752174));
#7887=CARTESIAN_POINT('Ctrl Pts',(-2.36230514952321,31.9683439237533,11.9464948680741));
#7888=CARTESIAN_POINT('Ctrl Pts',(-2.63975329031857,31.9794893366318,11.884870753031));
#7889=CARTESIAN_POINT('Ctrl Pts',(-2.91717063006565,31.9906335121966,11.8232534792208));
#7890=CARTESIAN_POINT('Ctrl Pts',(-3.19244770310074,32.0017776877613,11.7519147108885));
#7891=CARTESIAN_POINT('Ctrl Pts',(-3.46489782258198,32.0129218633261,11.6710296601914));
#7892=CARTESIAN_POINT('Ctrl Pts',(-3.74592794981203,32.0244169916189,11.5875973749286));
#7893=CARTESIAN_POINT('Ctrl Pts',(-4.02394989801848,32.0359121199117,11.4940078756693));
#7894=CARTESIAN_POINT('Ctrl Pts',(-4.2982264070027,32.0474072482046,11.3905092074123));
#7895=CARTESIAN_POINT('Ctrl Pts',(-4.56414331051031,32.0585520193422,11.2901650493144));
#7896=CARTESIAN_POINT('Ctrl Pts',(-4.82653944546965,32.0696967904798,11.1805069143616));
#7897=CARTESIAN_POINT('Ctrl Pts',(-5.08476174610048,32.0808415616174,11.0618103507244));
#7898=CARTESIAN_POINT('Ctrl Pts',(-5.35516061315147,32.0925118684879,10.9375166074964));
#7899=CARTESIAN_POINT('Ctrl Pts',(-5.6209822480959,32.1041821753583,10.803311636784));
#7900=CARTESIAN_POINT('Ctrl Pts',(-5.88150296641289,32.1158524822288,10.6595672100736));
#7901=CARTESIAN_POINT('Ctrl Pts',(-6.14202368472985,32.1275227890992,10.5158227833632));
#7902=CARTESIAN_POINT('Ctrl Pts',(-6.39724319690724,32.1391930959697,10.362539070421));
#7903=CARTESIAN_POINT('Ctrl Pts',(-6.64646899845364,32.1508634028401,10.2001421609012));
#7904=CARTESIAN_POINT('Ctrl Pts',(-6.88452583494995,32.1620107090872,10.0450230107282));
#7905=CARTESIAN_POINT('Ctrl Pts',(-7.11718546291348,32.1731580153343,9.88154319117064));
#7906=CARTESIAN_POINT('Ctrl Pts',(-7.3438637301814,32.1843053215814,9.71010379772154));
#7907=CARTESIAN_POINT('Ctrl Pts',(-7.57050349617527,32.19545073446,9.53869352323099));
#7908=CARTESIAN_POINT('Ctrl Pts',(-7.79116371711331,32.2065961473386,9.3593265348274));
#7909=CARTESIAN_POINT('Ctrl Pts',(-8.00529124878566,32.2177415602172,9.17244581734423));
#7910=CARTESIAN_POINT('Ctrl Pts',(-8.2193950089754,32.2288857357819,8.98558584652402));
#7911=CARTESIAN_POINT('Ctrl Pts',(-8.42696732714878,32.2400299113465,8.79121398762406));
#7912=CARTESIAN_POINT('Ctrl Pts',(-8.627489094617,32.2511740869111,8.58981269715847));
#7913=CARTESIAN_POINT('Ctrl Pts',(-8.83432569990824,32.2626692152039,8.3820688709039));
#7914=CARTESIAN_POINT('Ctrl Pts',(-9.03366027000809,32.2741643434968,8.16684589996586));
#7915=CARTESIAN_POINT('Ctrl Pts',(-9.22496414319454,32.2856594717896,7.94471439428599));
#7916=CARTESIAN_POINT('Ctrl Pts',(-9.41043731322679,32.2968042429273,7.72935317950114));
#7917=CARTESIAN_POINT('Ctrl Pts',(-9.58836188649626,32.3079490140649,7.50749853242398));
#7918=CARTESIAN_POINT('Ctrl Pts',(-9.75829629083444,32.3190937852025,7.27970492192416));
#7919=CARTESIAN_POINT('Ctrl Pts',(-9.93624401376104,32.3307640920729,7.04116962094411));
#7920=CARTESIAN_POINT('Ctrl Pts',(-10.1054296870796,32.3424343989434,6.79612202615387));
#7921=CARTESIAN_POINT('Ctrl Pts',(-10.2653957777935,32.3541047058139,6.54523489076284));
#7922=CARTESIAN_POINT('Ctrl Pts',(-10.4253618685074,32.3657750126843,6.2943477553718));
#7923=CARTESIAN_POINT('Ctrl Pts',(-10.576108203647,32.3774453195548,6.03762136698964));
#7924=CARTESIAN_POINT('Ctrl Pts',(-10.7172306218485,32.3891156264253,5.77576125269328));
#7925=CARTESIAN_POINT('Ctrl Pts',(-10.8519688998768,32.4002579882968,5.52574724829742));
#7926=CARTESIAN_POINT('Ctrl Pts',(-10.9779752599429,32.4114003501683,5.27097837052066));
#7927=CARTESIAN_POINT('Ctrl Pts',(-11.0949288753281,32.4225427120399,5.0120857436213));
#7928=CARTESIAN_POINT('Ctrl Pts',(-11.2118624589273,32.4336831654505,4.75323745978609));
#7929=CARTESIAN_POINT('Ctrl Pts',(-11.3197462835136,32.4448236188611,4.49026708040664));
#7930=CARTESIAN_POINT('Ctrl Pts',(-11.418306790496,32.4559640722717,4.22382768210448));
#7931=CARTESIAN_POINT('Ctrl Pts',(-11.5168563332357,32.4671032863762,3.9574179235265));
#7932=CARTESIAN_POINT('Ctrl Pts',(-11.6060845367131,32.4782425004807,3.68754016717926));
#7933=CARTESIAN_POINT('Ctrl Pts',(-11.6857666143717,32.4893817145852,3.41486586624351));
#7934=CARTESIAN_POINT('Ctrl Pts',(-11.7666848528916,32.500693738698,3.13796138822696));
#7935=CARTESIAN_POINT('Ctrl Pts',(-11.8377582625043,32.5120057628108,2.85817315383455));
#7936=CARTESIAN_POINT('Ctrl Pts',(-11.8988041826084,32.5233177869236,2.57621995837733));
#7937=CARTESIAN_POINT('Ctrl Pts',(-11.9589208024357,32.5344576084204,2.29855892826241));
#7938=CARTESIAN_POINT('Ctrl Pts',(-12.009312981119,32.5455974299172,2.01879864552249));
#7939=CARTESIAN_POINT('Ctrl Pts',(-12.0498576548315,32.556737251414,1.73763654090826));
#7940=CARTESIAN_POINT('Ctrl Pts',(-12.0913424556654,32.5681353768348,1.44995500733155));
#7941=CARTESIAN_POINT('Ctrl Pts',(-12.1225175320442,32.5795335022556,1.16080614795246));
#7942=CARTESIAN_POINT('Ctrl Pts',(-12.1433070423736,32.5909316276764,0.870944501468714));
#7943=CARTESIAN_POINT('Ctrl Pts',(-12.1640965527031,32.6023297530972,0.581082854984967));
#7944=CARTESIAN_POINT('Ctrl Pts',(-12.1745004835326,32.613727878518,0.290508720558424));
#7945=CARTESIAN_POINT('Ctrl Pts',(-12.1744999999831,32.6251260039388,-2.02629457920173E-5));
#7946=CARTESIAN_POINT('Ctrl Pts',(-12.1744999999831,32.6251260039651,-2.02636154117562E-5));
#7947=CARTESIAN_POINT('Ctrl Pts',(-12.1744999682797,32.6258732859801,-0.0190678768165046));
#7948=CARTESIAN_POINT('Ctrl Pts',(-12.1744552351083,32.6266205679952,-0.0381154725570181));
#7949=CARTESIAN_POINT('Ctrl Pts',(-12.1743658010439,32.6273678500103,-0.057162858329975));
#7950=CARTESIAN_POINT('Ctrl Pts',(-12.1730317010868,32.6385151562574,-0.341295271704965));
#7951=CARTESIAN_POINT('Ctrl Pts',(-12.1617461874558,32.6496624625045,-0.625423396093907));
#7952=CARTESIAN_POINT('Ctrl Pts',(-12.1405297269587,32.6608097687516,-0.908838928981096));
#7953=CARTESIAN_POINT('Ctrl Pts',(-12.1193168700748,32.6719551816302,-1.19220632377607));
#7954=CARTESIAN_POINT('Ctrl Pts',(-12.0881764538661,32.6831005945087,-1.47486110281071));
#7955=CARTESIAN_POINT('Ctrl Pts',(-12.0471809543266,32.6942460073873,-1.75609831834951));
#7956=CARTESIAN_POINT('Ctrl Pts',(-12.0061900059243,32.7053901829519,-2.03730431218924));
#7957=CARTESIAN_POINT('Ctrl Pts',(-11.9553461973366,32.7165343585165,-2.31709279288919));
#7958=CARTESIAN_POINT('Ctrl Pts',(-11.8947736229075,32.7276785340811,-2.59476602216561));
#7959=CARTESIAN_POINT('Ctrl Pts',(-11.8322934950546,32.739173662374,-2.88118374553293));
#7960=CARTESIAN_POINT('Ctrl Pts',(-11.7594619685466,32.7506687906668,-3.16535053951657));
#7961=CARTESIAN_POINT('Ctrl Pts',(-11.6764720426416,32.7621639189597,-3.44651285902283));
#7962=CARTESIAN_POINT('Ctrl Pts',(-11.5960115460404,32.7733086900973,-3.71910570214559));
#7963=CARTESIAN_POINT('Ctrl Pts',(-11.506002790155,32.7844534612349,-3.98887423638641));
#7964=CARTESIAN_POINT('Ctrl Pts',(-11.4066724115637,32.7955982323725,-4.25514685354945));
#7965=CARTESIAN_POINT('Ctrl Pts',(-11.3026580728741,32.807268539243,-4.53397565273587));
#7966=CARTESIAN_POINT('Ctrl Pts',(-11.1884219401367,32.8189388461134,-4.80897060131908));
#7967=CARTESIAN_POINT('Ctrl Pts',(-11.0642814033507,32.8306091529839,-5.07938256852815));
#7968=CARTESIAN_POINT('Ctrl Pts',(-10.9401408665647,32.8422794598544,-5.34979453573721));
#7969=CARTESIAN_POINT('Ctrl Pts',(-10.8060960736838,32.8539497667249,-5.61562322032863));
#7970=CARTESIAN_POINT('Ctrl Pts',(-10.6625208843845,32.8656200735954,-5.87614658088653));
#7971=CARTESIAN_POINT('Ctrl Pts',(-10.5253799657805,32.8767673798425,-6.12499468033231));
#7972=CARTESIAN_POINT('Ctrl Pts',(-10.3795031187475,32.8879146860897,-6.3690768373752));
#7973=CARTESIAN_POINT('Ctrl Pts',(-10.2252472674586,32.8990619923368,-6.60778091111761));
#7974=CARTESIAN_POINT('Ctrl Pts',(-10.0710176165062,32.9102074052154,-6.84644444100378));
#7975=CARTESIAN_POINT('Ctrl Pts',(-9.9084119473859,32.921352818094,-7.07973148737207));
#7976=CARTESIAN_POINT('Ctrl Pts',(-9.73783124627379,32.9324982309726,-7.30705774365399));
#7977=CARTESIAN_POINT('Ctrl Pts',(-9.56726948226978,32.9436424065372,-7.53435876318956));
#7978=CARTESIAN_POINT('Ctrl Pts',(-9.3887346142411,32.9547865821018,-7.75570010072467));
#7979=CARTESIAN_POINT('Ctrl Pts',(-9.20266950256293,32.9659307576664,-7.97052848163773));
#7980=CARTESIAN_POINT('Ctrl Pts',(-9.01074482252143,32.9774258859592,-8.19212224469573));
#7981=CARTESIAN_POINT('Ctrl Pts',(-8.81080811489427,32.9889210142521,-8.40678596077151));
#7982=CARTESIAN_POINT('Ctrl Pts',(-8.60338944894226,33.0004161425449,-8.6139503272209));
#7983=CARTESIAN_POINT('Ctrl Pts',(-8.40229264490357,33.0115609136825,-8.81480058248823));
#7984=CARTESIAN_POINT('Ctrl Pts',(-8.19416340784828,33.0227056848202,-9.00860166320182));
#7985=CARTESIAN_POINT('Ctrl Pts',(-7.97952213246204,33.0338504559578,-9.19487230947491));
#7986=CARTESIAN_POINT('Ctrl Pts',(-7.75475936973759,33.0455207628282,-9.38992661576092));
#7987=CARTESIAN_POINT('Ctrl Pts',(-7.52285587600274,33.0571910696987,-9.57672298982141));
#7988=CARTESIAN_POINT('Ctrl Pts',(-7.28444883114305,33.0688613765691,-9.75475553135283));
#7989=CARTESIAN_POINT('Ctrl Pts',(-7.04604178628334,33.0805316834396,-9.93278807288427));
#7990=CARTESIAN_POINT('Ctrl Pts',(-6.80113146436942,33.09220199031,-10.1020565881776));
#7991=CARTESIAN_POINT('Ctrl Pts',(-6.55039166588011,33.1038722971805,-10.2621059862763));
#7992=CARTESIAN_POINT('Ctrl Pts',(-6.31088868167215,33.1150196034276,-10.4149828279117));
#7993=CARTESIAN_POINT('Ctrl Pts',(-6.06599569770914,33.1261669096747,-10.5594943509551));
#7994=CARTESIAN_POINT('Ctrl Pts',(-5.81631905191834,33.1373142159218,-10.695273859808));
#7995=CARTESIAN_POINT('Ctrl Pts',(-5.56668481367376,33.1484596288003,-10.8310303065287));
#7996=CARTESIAN_POINT('Ctrl Pts',(-5.31226877001417,33.1596050416789,-10.9580575727416));
#7997=CARTESIAN_POINT('Ctrl Pts',(-5.05370262822269,33.1707504545575,-11.0760344887281));
#7998=CARTESIAN_POINT('Ctrl Pts',(-4.79516519128955,33.1818946301221,-11.1939983074444));
#7999=CARTESIAN_POINT('Ctrl Pts',(-4.53247881883711,33.1930388056867,-11.3029136715195));
#8000=CARTESIAN_POINT('Ctrl Pts',(-4.26629713627511,33.2041829812513,-11.4025066978718));
#8001=CARTESIAN_POINT('Ctrl Pts',(-3.9917328517731,33.2156781095442,-11.5052361109501));
#8002=CARTESIAN_POINT('Ctrl Pts',(-3.71344981544439,33.227173237837,-11.5980463999713));
#8003=CARTESIAN_POINT('Ctrl Pts',(-3.43218589779943,33.2386683661299,-11.6806913413953));
#8004=CARTESIAN_POINT('Ctrl Pts',(-3.15949455312228,33.2498131372675,-11.7608173682115));
#8005=CARTESIAN_POINT('Ctrl Pts',(-2.8840016112494,33.2609579084051,-11.8313884471381));
#8006=CARTESIAN_POINT('Ctrl Pts',(-2.60639431557328,33.2721026795427,-11.8922310321381));
#8007=CARTESIAN_POINT('Ctrl Pts',(-2.31569634698968,33.2837729864132,-11.9559426713433));
#8008=CARTESIAN_POINT('Ctrl Pts',(-2.02268013077371,33.2954432932836,-12.0089861705082));
#8009=CARTESIAN_POINT('Ctrl Pts',(-1.7281472467221,33.3071136001541,-12.0512222344311));
#8010=CARTESIAN_POINT('Ctrl Pts',(-1.43361436267048,33.3187839070246,-12.0934582983541));
#8011=CARTESIAN_POINT('Ctrl Pts',(-1.13756514413288,33.3304542138951,-12.1248868881006));
#8012=CARTESIAN_POINT('Ctrl Pts',(-0.840809011698687,33.3421245207656,-12.1454308468595));
#8013=CARTESIAN_POINT('Ctrl Pts',(-0.557351899073608,33.3532718270128,-12.1650541354633));
#8014=CARTESIAN_POINT('Ctrl Pts',(-0.273165182359102,33.3644191332599,-12.1747527915611));
#8015=CARTESIAN_POINT('Ctrl Pts',(0.0110432552658722,33.375566439507,-12.1744949914365));
#8016=CARTESIAN_POINT('Ctrl Pts',(0.295203420124147,33.3867118523856,-12.1742372350993));
#8017=CARTESIAN_POINT('Ctrl Pts',(0.579385031881237,33.3978572652642,-12.1640263990678));
#8018=CARTESIAN_POINT('Ctrl Pts',(0.862879717510703,33.4090026781428,-12.1438827745951));
#8019=CARTESIAN_POINT('Ctrl Pts',(1.1463429308258,33.4201468537074,-12.1237413863777));
#8020=CARTESIAN_POINT('Ctrl Pts',(1.42911910428315,33.431291029272,-12.0936694305245));
#8021=CARTESIAN_POINT('Ctrl Pts',(1.71050324800708,33.4424352048366,-12.0537392077545));
#8022=CARTESIAN_POINT('Ctrl Pts',(2.00074875005636,33.4539303331295,-12.0125515011501));
#8023=CARTESIAN_POINT('Ctrl Pts',(2.28951283081747,33.4654254614223,-11.9608745844622));
#8024=CARTESIAN_POINT('Ctrl Pts',(2.57602976407282,33.4769205897152,-11.8988453601436));
#8025=CARTESIAN_POINT('Ctrl Pts',(2.85381401900525,33.4880653608528,-11.8387067091201));
#8026=CARTESIAN_POINT('Ctrl Pts',(3.12948580577546,33.4992101319904,-11.7688375157537));
#8027=CARTESIAN_POINT('Ctrl Pts',(3.40235863131859,33.510354903128,-11.689414270779));
#8028=CARTESIAN_POINT('Ctrl Pts',(3.68809887410845,33.5220252099984,-11.6062457938262));
#8029=CARTESIAN_POINT('Ctrl Pts',(3.97076952676866,33.5336955168689,-11.5126006236718));
#8030=CARTESIAN_POINT('Ctrl Pts',(4.24960009200912,33.5453658237393,-11.4087400403373));
#8031=CARTESIAN_POINT('Ctrl Pts',(4.5284306572496,33.5570361306098,-11.3048794570028));
#8032=CARTESIAN_POINT('Ctrl Pts',(4.80342082373608,33.5687064374802,-11.1908035858234));
#8033=CARTESIAN_POINT('Ctrl Pts',(5.07382294533181,33.5803767443507,-11.0668320204756));
#8034=CARTESIAN_POINT('Ctrl Pts',(5.33210709267749,33.5915240505978,-10.9484161964355));
#8035=CARTESIAN_POINT('Ctrl Pts',(5.58628251884841,33.6026713568449,-10.8209367603774));
#8036=CARTESIAN_POINT('Ctrl Pts',(5.83571242790281,33.6138186630921,-10.6847045213623));
#8037=CARTESIAN_POINT('Ctrl Pts',(6.0850999713191,33.6249640759706,-10.5484954213756));
#8038=CARTESIAN_POINT('Ctrl Pts',(6.32974337283193,33.6361094888492,-10.4035366143671));
#8039=CARTESIAN_POINT('Ctrl Pts',(6.56903034562025,33.6472549017278,-10.2501849041039));
#8040=CARTESIAN_POINT('Ctrl Pts',(6.80829075383676,33.6583990772924,-10.0968502182633));
#8041=CARTESIAN_POINT('Ctrl Pts',(7.04219569621666,33.669543252857,-9.93512463360258));
#8042=CARTESIAN_POINT('Ctrl Pts',(7.27016074531316,33.6806874284215,-9.76540900256142));
#8043=CARTESIAN_POINT('Ctrl Pts',(7.50530487692386,33.6921825567144,-9.59034868151615));
#8044=CARTESIAN_POINT('Ctrl Pts',(7.73412869047147,33.7036776850073,-9.40678708310855));
#8045=CARTESIAN_POINT('Ctrl Pts',(7.95602534278516,33.7151728133001,-9.21521084918627));
#8046=CARTESIAN_POINT('Ctrl Pts',(8.17115886224074,33.7263175844377,-9.02947361963365));
#8047=CARTESIAN_POINT('Ctrl Pts',(8.37978101882481,33.7374623555753,-8.83620325463972));
#8048=CARTESIAN_POINT('Ctrl Pts',(8.5813734858511,33.7486071267129,-8.63588324066113));
#8049=CARTESIAN_POINT('Ctrl Pts',(8.79247211891656,33.7602774335834,-8.42611706362923));
#8050=CARTESIAN_POINT('Ctrl Pts',(8.9958619094496,33.7719477404539,-8.20862060647202));
#8051=CARTESIAN_POINT('Ctrl Pts',(9.19099134494893,33.7836180473244,-7.98399200569952));
#8052=CARTESIAN_POINT('Ctrl Pts',(9.38612078044827,33.7952883541949,-7.75936340492701));
#8053=CARTESIAN_POINT('Ctrl Pts',(9.5729896475206,33.8069586610653,-7.52760291957819));
#8054=CARTESIAN_POINT('Ctrl Pts',(9.75109440402037,33.8186289679358,-7.28934895404814));
#8055=CARTESIAN_POINT('Ctrl Pts',(9.92121745963443,33.8297762741829,-7.0617722546679));
#8056=CARTESIAN_POINT('Ctrl Pts',(10.0833954685513,33.8409235804299,-6.82820331985479));
#8057=CARTESIAN_POINT('Ctrl Pts',(10.2372180184085,33.852070886677,-6.58921979399478));
#8058=CARTESIAN_POINT('Ctrl Pts',(10.3910144415251,33.8632162995555,-6.35027685945628));
#8059=CARTESIAN_POINT('Ctrl Pts',(10.5364580946447,33.874361712434,-6.10592139420272));
#8060=CARTESIAN_POINT('Ctrl Pts',(10.6731820964191,33.8855071253125,-5.85675970026768));
#8061=CARTESIAN_POINT('Ctrl Pts',(10.8098909197054,33.8966513008771,-5.60762566715114));
#8062=CARTESIAN_POINT('Ctrl Pts',(10.9378818963315,33.9077954764416,-5.35368670459261));
#8063=CARTESIAN_POINT('Ctrl Pts',(11.0568336864415,33.9189396520062,-5.09557446029115));
#8064=CARTESIAN_POINT('Ctrl Pts',(11.1795315100773,33.9304347802991,-4.82933373705156));
#8065=CARTESIAN_POINT('Ctrl Pts',(11.2926114639304,33.941929908592,-4.55865288790684));
#8066=CARTESIAN_POINT('Ctrl Pts',(11.3957735795933,33.9534250368849,-4.28424961605228));
#8067=CARTESIAN_POINT('Ctrl Pts',(11.4957914427987,33.9645698080224,-4.01820981325158));
#8068=CARTESIAN_POINT('Ctrl Pts',(11.5864869838508,33.97571457916,-3.7486713984846));
#8069=CARTESIAN_POINT('Ctrl Pts',(11.6676364475165,33.9868593502975,-3.47630694539264));
#8070=CARTESIAN_POINT('Ctrl Pts',(11.7526125436312,33.9985296571681,-3.19109904753701));
#8071=CARTESIAN_POINT('Ctrl Pts',(11.8271205113252,34.0101999640387,-2.90279247716342));
#8072=CARTESIAN_POINT('Ctrl Pts',(11.8909623210325,34.0218702709092,-2.61217635885952));
#8073=CARTESIAN_POINT('Ctrl Pts',(11.9548041307399,34.0335405777798,-2.32156024055564));
#8074=CARTESIAN_POINT('Ctrl Pts',(12.0079797190489,34.0452108846504,-2.02863490389215));
#8075=CARTESIAN_POINT('Ctrl Pts',(12.0503524473524,34.056881191521,-1.73420187538456));
#8076=CARTESIAN_POINT('Ctrl Pts',(12.0908262570107,34.0680284977683,-1.45296375761318));
#8077=CARTESIAN_POINT('Ctrl Pts',(12.1214562644126,34.0791758040156,-1.17026611606645));
#8078=CARTESIAN_POINT('Ctrl Pts',(12.142158528628,34.0903231102629,-0.886812559488088));
#8079=CARTESIAN_POINT('Ctrl Pts',(12.1628572765665,34.1014685231416,-0.603407147460176));
#8080=CARTESIAN_POINT('Ctrl Pts',(12.1736316284451,34.1126139360204,-0.319246342673114));
#8081=CARTESIAN_POINT('Ctrl Pts',(12.1744495802706,34.1237593488991,-0.0350380856780686));
#8082=CARTESIAN_POINT('Ctrl Pts',(12.1752674412908,34.1349035244639,0.249138619785386));
#8083=CARTESIAN_POINT('Ctrl Pts',(12.1661311086289,34.1460477000287,0.533362500259884));
#8084=CARTESIAN_POINT('Ctrl Pts',(12.1470606956327,34.1571918755935,0.816925153619469));
#8085=CARTESIAN_POINT('Ctrl Pts',(12.1273897165896,34.1686870038862,1.10941777099075));
#8086=CARTESIAN_POINT('Ctrl Pts',(12.0971488397799,34.1801821321789,1.40120654292002));
#8087=CARTESIAN_POINT('Ctrl Pts',(12.0564181252866,34.1916772604716,1.69151773217481));
#8088=CARTESIAN_POINT('Ctrl Pts',(12.0169288321053,34.2028220316094,1.97298059892988));
#8089=CARTESIAN_POINT('Ctrl Pts',(11.9675797055986,34.2139668027472,2.25305434264466));
#8090=CARTESIAN_POINT('Ctrl Pts',(11.9084961294965,34.225111573885,2.53104132399424));
#8091=CARTESIAN_POINT('Ctrl Pts',(11.8466264458957,34.2367818807552,2.82213688245413));
#8092=CARTESIAN_POINT('Ctrl Pts',(11.7740822255187,34.2484521876253,3.11094382810151));
#8093=CARTESIAN_POINT('Ctrl Pts',(11.6910672154904,34.2601224944955,3.39667449321921));
#8094=CARTESIAN_POINT('Ctrl Pts',(11.608052205462,34.2717928013657,3.68240515833693));
#8095=CARTESIAN_POINT('Ctrl Pts',(11.5145665078164,34.2834631082358,3.96505922319547));
#8096=CARTESIAN_POINT('Ctrl Pts',(11.4108737097382,34.295133415106,4.24386750858299));
#8097=CARTESIAN_POINT('Ctrl Pts',(11.3118278672755,34.3062807213527,4.51018110049645));
#8098=CARTESIAN_POINT('Ctrl Pts',(11.2034400892115,34.3174280275994,4.77306556836597));
#8099=CARTESIAN_POINT('Ctrl Pts',(11.0859733768434,34.3285753338461,5.03186292916634));
#8100=CARTESIAN_POINT('Ctrl Pts',(10.9685266161816,34.3397207467242,5.29061633326782));
#8101=CARTESIAN_POINT('Ctrl Pts',(10.8420041101378,34.3508661596023,5.54528377345437));
#8102=CARTESIAN_POINT('Ctrl Pts',(10.7067165369335,34.3620115724805,5.79522831713764));
#8103=CARTESIAN_POINT('Ctrl Pts',(10.5714439827516,34.3731557480446,6.04514511309366));
#8104=CARTESIAN_POINT('Ctrl Pts',(10.4274084313955,34.3842999236088,6.29033982499244));
#8105=CARTESIAN_POINT('Ctrl Pts',(10.2749665443453,34.395444099173,6.53020005532642));
#8106=CARTESIAN_POINT('Ctrl Pts',(10.117723952571,34.4069392274662,6.77761397161364));
#8107=CARTESIAN_POINT('Ctrl Pts',(9.95153713121388,34.4184343557593,7.01935171891168));
#8108=CARTESIAN_POINT('Ctrl Pts',(9.77684664447996,34.4299294840525,7.25477221836227));
#8109=CARTESIAN_POINT('Ctrl Pts',(9.60748050563951,34.4410742551897,7.48301739496749));
#8110=CARTESIAN_POINT('Ctrl Pts',(9.43012155403504,34.4522190263269,7.7053244809599));
#8111=CARTESIAN_POINT('Ctrl Pts',(9.24521373484962,34.4633637974641,7.92114090563651));
#8112=CARTESIAN_POINT('Ctrl Pts',(9.05158652023803,34.4750341043353,8.14713423226626));
#8113=CARTESIAN_POINT('Ctrl Pts',(8.84968157512732,34.4867044112064,8.36600978804986));
#8114=CARTESIAN_POINT('Ctrl Pts',(8.64005473522879,34.4983747180776,8.5771734517993));
#8115=CARTESIAN_POINT('Ctrl Pts',(8.43042789533026,34.5100450249488,8.78833711554873));
#8116=CARTESIAN_POINT('Ctrl Pts',(8.21307940324054,34.52171533182,8.99178865534857));
#8117=CARTESIAN_POINT('Ctrl Pts',(7.98860879055077,34.5333856386912,9.18697882013097));
#8118=CARTESIAN_POINT('Ctrl Pts',(7.77419774798598,34.5445329449391,9.37342160757606));
#8119=CARTESIAN_POINT('Ctrl Pts',(7.55322486774204,34.5556802511869,9.55238288856828));
#8120=CARTESIAN_POINT('Ctrl Pts',(7.32623595483955,34.5668275574348,9.72341076906742));
#8121=CARTESIAN_POINT('Ctrl Pts',(7.09928559597489,34.5779729703142,9.89440960050293));
#8122=CARTESIAN_POINT('Ctrl Pts',(6.8663214574821,34.5891183831935,10.0574775612436));
#8123=CARTESIAN_POINT('Ctrl Pts',(6.62792113425293,34.6002637960728,10.21220405633));
#8124=CARTESIAN_POINT('Ctrl Pts',(6.38954727716328,34.6114079716382,10.3669133743718));
#8125=CARTESIAN_POINT('Ctrl Pts',(6.14573866412806,34.6225521472035,10.5132829307159));
#8126=CARTESIAN_POINT('Ctrl Pts',(5.89710152521208,34.6336963227689,10.6509456787339));
#8127=CARTESIAN_POINT('Ctrl Pts',(5.64063429770819,34.6451914510612,10.7929437063363));
#8128=CARTESIAN_POINT('Ctrl Pts',(5.37902975093839,34.6566865793535,10.925677496898));
#8129=CARTESIAN_POINT('Ctrl Pts',(5.11298151220474,34.6681817076457,11.0487949707582));
#8130=CARTESIAN_POINT('Ctrl Pts',(4.85504209151608,34.6793264787841,11.1681599777785));
#8131=CARTESIAN_POINT('Ctrl Pts',(4.59292609736622,34.6904712499225,11.2784860573086));
#8132=CARTESIAN_POINT('Ctrl Pts',(4.327287770841,34.7016160210608,11.3795004634795));
#8133=CARTESIAN_POINT('Ctrl Pts',(4.04912317254728,34.7132863279301,11.4852782406623));
#8134=CARTESIAN_POINT('Ctrl Pts',(3.7670963520758,34.7249566347993,11.5808449099814));
#8135=CARTESIAN_POINT('Ctrl Pts',(3.48197968126939,34.7366269416685,11.6659447859669));
#8136=CARTESIAN_POINT('Ctrl Pts',(3.19686301046297,34.7482972485378,11.7510446619523));
#8137=CARTESIAN_POINT('Ctrl Pts',(2.90865681331852,34.759967555407,11.8256776570603));
#8138=CARTESIAN_POINT('Ctrl Pts',(2.61815035720158,34.7716378622762,11.8896483950151));
#8139=CARTESIAN_POINT('Ctrl Pts',(2.34066544362123,34.7827850640849,11.9507517347836));
#8140=CARTESIAN_POINT('Ctrl Pts',(2.06099907596949,34.7939322658936,12.0021458934422));
#8141=CARTESIAN_POINT('Ctrl Pts',(1.77984673713931,34.8050794677023,12.0436952735568));
#8142=CARTESIAN_POINT('Ctrl Pts',(1.71689781304658,34.8075752831859,12.0529980194839));
#8143=CARTESIAN_POINT('Ctrl Pts',(1.65387443840511,34.8100710986695,12.0618074546403));
#8144=CARTESIAN_POINT('Ctrl Pts',(1.59078448392778,34.8125669141531,12.0701224093086));
#8145=CARTESIAN_POINT('Origin',(0.,13.3748739960349,0.));
#8146=CARTESIAN_POINT('',(1.59078448392772,38.0622997972676,12.0701224093087));
#8147=CARTESIAN_POINT('',(1.59078448392769,37.8125509746976,12.0701224093087));
#8148=CARTESIAN_POINT('',(1.59078448392774,13.3748739960349,12.0701224093086));
#8149=CARTESIAN_POINT('',(-12.1744999966649,35.8748739960676,-0.000284967810357368));
#8150=CARTESIAN_POINT('Ctrl Pts',(-12.1744999966649,35.8748739960676,-0.000284967810371163));
#8151=CARTESIAN_POINT('Ctrl Pts',(-12.1744930883501,35.8864472961776,-0.295424542797684));
#8152=CARTESIAN_POINT('Ctrl Pts',(-12.163749488268,35.8980205962875,-0.590512724686085));
#8153=CARTESIAN_POINT('Ctrl Pts',(-12.1423063610032,35.9095938963975,-0.884786124179511));
#8154=CARTESIAN_POINT('Ctrl Pts',(-12.1208567139894,35.9211707153511,-1.17914899703588));
#8155=CARTESIAN_POINT('Ctrl Pts',(-12.0887010545349,35.9327475343047,-1.47269637376915));
#8156=CARTESIAN_POINT('Ctrl Pts',(-12.0459284961632,35.9443243532583,-1.76466906680104));
#8157=CARTESIAN_POINT('Ctrl Pts',(-12.0392930536843,35.9461203018566,-1.80996371560749));
#8158=CARTESIAN_POINT('Ctrl Pts',(-12.0324022028897,35.9479162504549,-1.85522048095315));
#8159=CARTESIAN_POINT('Ctrl Pts',(-12.0252563877582,35.9497121990533,-1.90043654423916));
#8160=CARTESIAN_POINT('Ctrl Pts',(-11.9809028943906,35.9608595059425,-2.18108897173295));
#8161=CARTESIAN_POINT('Ctrl Pts',(-11.9267134419172,35.9720068128318,-2.46022991528048));
#8162=CARTESIAN_POINT('Ctrl Pts',(-11.8628155407781,35.9831541197211,-2.73716234364608));
#8163=CARTESIAN_POINT('Ctrl Pts',(-11.7989284926723,35.9942995332446,-3.01404773514772));
#8164=CARTESIAN_POINT('Ctrl Pts',(-11.7253363480305,36.0054449467682,-3.28872510056579));
#8165=CARTESIAN_POINT('Ctrl Pts',(-11.6422175183502,36.0165903602918,-3.56050860207074));
#8166=CARTESIAN_POINT('Ctrl Pts',(-11.559107916142,36.0277345365026,-3.8322619314151));
#8167=CARTESIAN_POINT('Ctrl Pts',(-11.466473818764,36.0388787127133,-4.10112178333928));
#8168=CARTESIAN_POINT('Ctrl Pts',(-11.3645435686143,36.0500228889241,-4.36641726442477));
#8169=CARTESIAN_POINT('Ctrl Pts',(-11.2594033383302,36.0615180167336,-4.64006741179234));
#8170=CARTESIAN_POINT('Ctrl Pts',(-11.1443720573033,36.0730131445432,-4.90992477220224));
#8171=CARTESIAN_POINT('Ctrl Pts',(-11.0197546303388,36.0845082723527,-5.17527372581657));
#8172=CARTESIAN_POINT('Ctrl Pts',(-10.8989353748965,36.0956530441313,-5.43253520030673));
#8173=CARTESIAN_POINT('Ctrl Pts',(-10.7691057848687,36.1067978159099,-5.68555876622977));
#8174=CARTESIAN_POINT('Ctrl Pts',(-10.6305916042168,36.1179425876886,-5.93371488987754));
#8175=CARTESIAN_POINT('Ctrl Pts',(-10.4855457583789,36.1296128935136,-6.19357286748642));
#8176=CARTESIAN_POINT('Ctrl Pts',(-10.3309767217692,36.1412831993385,-6.44809302920758));
#8177=CARTESIAN_POINT('Ctrl Pts',(-10.1673116861847,36.1529535051635,-6.69658295894055));
#8178=CARTESIAN_POINT('Ctrl Pts',(-10.0036466506002,36.1646238109885,-6.9450728886735));
#8179=CARTESIAN_POINT('Ctrl Pts',(-9.83088580791383,36.1762941168134,-7.18753231105948));
#8180=CARTESIAN_POINT('Ctrl Pts',(-9.64950806513854,36.1879644226384,-7.42330413972284));
#8181=CARTESIAN_POINT('Ctrl Pts',(-9.47625871296853,36.199111727114,-7.6485099226974));
#8182=CARTESIAN_POINT('Ctrl Pts',(-9.29509606919364,36.2102590315895,-7.8676816020831));
#8183=CARTESIAN_POINT('Ctrl Pts',(-9.10646565514324,36.221406336065,-8.0802681590215));
#8184=CARTESIAN_POINT('Ctrl Pts',(-8.91786728005395,36.2325517471659,-8.2928186080371));
#8185=CARTESIAN_POINT('Ctrl Pts',(-8.72180384403198,36.2436971582667,-8.49878596821237));
#8186=CARTESIAN_POINT('Ctrl Pts',(-8.51876020628826,36.2548425693675,-8.69765340754388));
#8187=CARTESIAN_POINT('Ctrl Pts',(-8.31573910957317,36.2659867431529,-8.89649876947028));
#8188=CARTESIAN_POINT('Ctrl Pts',(-8.10573954903184,36.2771309169383,-9.08824559786713));
#8189=CARTESIAN_POINT('Ctrl Pts',(-7.88928307487955,36.2882750907237,-9.27241407694993));
#8190=CARTESIAN_POINT('Ctrl Pts',(-7.66600988509742,36.2997702203486,-9.46238244792694));
#8191=CARTESIAN_POINT('Ctrl Pts',(-7.43586672490532,36.3112653499736,-9.64428721563409));
#8192=CARTESIAN_POINT('Ctrl Pts',(-7.19946377540692,36.3227604795986,-9.81764592947839));
#8193=CARTESIAN_POINT('Ctrl Pts',(-6.97026615536178,36.3339052489754,-9.98572084018279));
#8194=CARTESIAN_POINT('Ctrl Pts',(-6.73518490496334,36.3450500183522,-10.1457627683423));
#8195=CARTESIAN_POINT('Ctrl Pts',(-6.49480730688629,36.3561947877291,-10.2973748254794));
#8196=CARTESIAN_POINT('Ctrl Pts',(-6.24309451396523,36.3678650974781,-10.4561362685081));
#8197=CARTESIAN_POINT('Ctrl Pts',(-5.98557411618706,36.3795354072272,-10.6056535064113));
#8198=CARTESIAN_POINT('Ctrl Pts',(-5.7229525669938,36.3912057169763,-10.7455229824304));
#8199=CARTESIAN_POINT('Ctrl Pts',(-5.46033101780052,36.4028760267254,-10.8853924584494));
#8200=CARTESIAN_POINT('Ctrl Pts',(-5.19260861744099,36.4145463364744,-11.0156140226206));
#8201=CARTESIAN_POINT('Ctrl Pts',(-4.9205203219068,36.4262166462235,-11.1358398880238));
#8202=CARTESIAN_POINT('Ctrl Pts',(-4.66062554473769,36.4373639561281,-11.2506778836736));
#8203=CARTESIAN_POINT('Ctrl Pts',(-4.39666996201338,36.4485112660327,-11.3564306914372));
#8204=CARTESIAN_POINT('Ctrl Pts',(-4.12930845682457,36.4596585759373,-11.4528276822101));
#8205=CARTESIAN_POINT('Ctrl Pts',(-3.86199236269481,36.4708039924835,-11.5492083000596));
#8206=CARTESIAN_POINT('Ctrl Pts',(-3.59127175189979,36.4819494090297,-11.6362361830668));
#8207=CARTESIAN_POINT('Ctrl Pts',(-3.31781968883708,36.4930948255759,-11.7136895452443));
#8208=CARTESIAN_POINT('Ctrl Pts',(-3.04439798317911,36.5042390048086,-11.7911343089017));
#8209=CARTESIAN_POINT('Ctrl Pts',(-2.76824568734694,36.5153831840413,-11.8590066015354));
#8210=CARTESIAN_POINT('Ctrl Pts',(-2.49005036894981,36.526527363274,-11.9171346979923));
#8211=CARTESIAN_POINT('Ctrl Pts',(-2.20309427787332,36.5380224888186,-11.9770933322249));
#8212=CARTESIAN_POINT('Ctrl Pts',(-1.91396469214712,36.5495176143631,-12.0266840376984));
#8213=CARTESIAN_POINT('Ctrl Pts',(-1.62342826198514,36.5610127399077,-12.065775189692));
#8214=CARTESIAN_POINT('Ctrl Pts',(-1.34174686044864,36.5721575146694,-12.1036749135756));
#8215=CARTESIAN_POINT('Ctrl Pts',(-1.05874337738828,36.5833022894311,-12.1317055846882));
#8216=CARTESIAN_POINT('Ctrl Pts',(-0.775123413472737,36.5944470641928,-12.149799749127));
#8217=CARTESIAN_POINT('Ctrl Pts',(-0.478129494697926,36.6061173651288,-12.1687471346687));
#8218=CARTESIAN_POINT('Ctrl Pts',(-0.180459873677726,36.6177876660647,-12.1767983435379));
#8219=CARTESIAN_POINT('Ctrl Pts',(0.11707202117144,36.6294579670007,-12.1739370949524));
#8220=CARTESIAN_POINT('Ctrl Pts',(0.414603916020578,36.6411282679367,-12.1710758463669));
#8221=CARTESIAN_POINT('Ctrl Pts',(0.711997749299544,36.6527985688726,-12.1573021523303));
#8222=CARTESIAN_POINT('Ctrl Pts',(1.00844175372276,36.6644688698086,-12.1326623409435));
#8223=CARTESIAN_POINT('Ctrl Pts',(1.29160072405077,36.6756161703009,-12.1091267540628));
#8224=CARTESIAN_POINT('Ctrl Pts',(1.57397769503675,36.6867634707932,-12.0756705357027));
#8225=CARTESIAN_POINT('Ctrl Pts',(1.85486813075634,36.6979107712855,-12.0323694452716));
#8226=CARTESIAN_POINT('Ctrl Pts',(2.13571085696984,36.7090561783983,-11.9890757095716));
#8227=CARTESIAN_POINT('Ctrl Pts',(2.41506728847831,36.720201585511,-11.9359404808946));
#8228=CARTESIAN_POINT('Ctrl Pts',(2.69224029849889,36.7313469926238,-11.8730911065796));
#8229=CARTESIAN_POINT('Ctrl Pts',(2.96938253809598,36.7424911624267,-11.8102487095019));
#8230=CARTESIAN_POINT('Ctrl Pts',(3.24434158014842,36.7536353322296,-11.7376943791884));
#8231=CARTESIAN_POINT('Ctrl Pts',(3.51643151935759,36.7647795020325,-11.655606360017));
#8232=CARTESIAN_POINT('Ctrl Pts',(3.79709037410433,36.776274634646,-11.5709331467551));
#8233=CARTESIAN_POINT('Ctrl Pts',(4.07469619766536,36.7877697672594,-11.4761161021925));
#8234=CARTESIAN_POINT('Ctrl Pts',(4.34851283179752,36.7992648998728,-11.3714065269734));
#8235=CARTESIAN_POINT('Ctrl Pts',(4.61398364177174,36.8104096653299,-11.2698884587465));
#8236=CARTESIAN_POINT('Ctrl Pts',(4.87589256715123,36.821554430787,-11.159072070423));
#8237=CARTESIAN_POINT('Ctrl Pts',(5.13358776672708,36.8326991962441,-11.039235792903));
#8238=CARTESIAN_POINT('Ctrl Pts',(5.40343503015256,36.8443695124357,-10.9137484279808));
#8239=CARTESIAN_POINT('Ctrl Pts',(5.66866130576691,36.8560398286273,-10.7783701409865));
#8240=CARTESIAN_POINT('Ctrl Pts',(5.92854455678638,36.8677101448189,-10.6334758986983));
#8241=CARTESIAN_POINT('Ctrl Pts',(6.18842780780583,36.8793804610105,-10.4885816564102));
#8242=CARTESIAN_POINT('Ctrl Pts',(6.4429677454689,36.8910507772021,-10.3341716298738));
#8243=CARTESIAN_POINT('Ctrl Pts',(6.69147375292597,36.9027210933937,-10.1706749659943));
#8244=CARTESIAN_POINT('Ctrl Pts',(6.92884298123643,36.9138684051906,-10.0145053935419));
#8245=CARTESIAN_POINT('Ctrl Pts',(7.16077810612801,36.9250157169876,-9.84999907333248));
#8246=CARTESIAN_POINT('Ctrl Pts',(7.38669675289892,36.9361630287846,-9.67755967848882));
#8247=CARTESIAN_POINT('Ctrl Pts',(7.61257702739218,36.9473084472108,-9.50514957247294));
#8248=CARTESIAN_POINT('Ctrl Pts',(7.83244265202763,36.9584538656371,-9.32480924375483));
#8249=CARTESIAN_POINT('Ctrl Pts',(8.0457424448486,36.9695992840634,-9.13698411737493));
#8250=CARTESIAN_POINT('Ctrl Pts',(8.25901855777424,36.9807434651591,-8.94917984277024));
#8251=CARTESIAN_POINT('Ctrl Pts',(8.46573009427768,36.9918876462549,-8.75389260599716));
#8252=CARTESIAN_POINT('Ctrl Pts',(8.66536008199898,37.0030318273506,-8.55160715300338));
#8253=CARTESIAN_POINT('Ctrl Pts',(8.87127664691684,37.0145269514863,-8.34295149916703));
#8254=CARTESIAN_POINT('Ctrl Pts',(9.06965820838166,37.026022075622,-8.12684992765588));
#8255=CARTESIAN_POINT('Ctrl Pts',(9.25997863188271,37.0375171997577,-7.90387537775461));
#8256=CARTESIAN_POINT('Ctrl Pts',(9.44449848305687,37.0486619763178,-7.68769663032144));
#8257=CARTESIAN_POINT('Ctrl Pts',(9.62144111262719,37.0598067528779,-7.46505786145395));
#8258=CARTESIAN_POINT('Ctrl Pts',(9.79036740214472,37.070951529438,-7.23651548613157));
#8259=CARTESIAN_POINT('Ctrl Pts',(9.96725925054946,37.0826218273615,-6.99719641196586));
#8260=CARTESIAN_POINT('Ctrl Pts',(10.1353603737896,37.094292125285,-6.75140383280313));
#8261=CARTESIAN_POINT('Ctrl Pts',(10.2942162169648,37.1059624232084,-6.49981251486365));
#8262=CARTESIAN_POINT('Ctrl Pts',(10.4530720601401,37.1176327211319,-6.24822119692417));
#8263=CARTESIAN_POINT('Ctrl Pts',(10.6026824515541,37.1293030190554,-5.99083142857654));
#8264=CARTESIAN_POINT('Ctrl Pts',(10.742646351938,37.1409733169788,-5.72835051364639));
#8265=CARTESIAN_POINT('Ctrl Pts',(10.8763379661845,37.1521206268483,-5.47763231324153));
#8266=CARTESIAN_POINT('Ctrl Pts',(11.0012686005856,37.1632679367179,-5.22219436487314));
#8267=CARTESIAN_POINT('Ctrl Pts',(11.1171200677777,37.1744152465874,-4.9626698105571));
#8268=CARTESIAN_POINT('Ctrl Pts',(11.2329518581578,37.1855606631402,-4.70318933523264));
#8269=CARTESIAN_POINT('Ctrl Pts',(11.3397074513444,37.196706079693,-4.43962388319863));
#8270=CARTESIAN_POINT('Ctrl Pts',(11.4371160292913,37.2078514962458,-4.17262833026484));
#8271=CARTESIAN_POINT('Ctrl Pts',(11.5345137937413,37.2189956755263,-3.90566241697496));
#8272=CARTESIAN_POINT('Ctrl Pts',(11.6225665235307,37.2301398548069,-3.63526741367178));
#8273=CARTESIAN_POINT('Ctrl Pts',(11.7010522555776,37.2412840340875,-3.3621163516812));
#8274=CARTESIAN_POINT('Ctrl Pts',(11.782009616388,37.2527791596272,-3.08036336926517));
#8275=CARTESIAN_POINT('Ctrl Pts',(11.8527875672035,37.2642742851669,-2.79567821335521));
#8276=CARTESIAN_POINT('Ctrl Pts',(11.9131983041429,37.2757694107066,-2.50881573977965));
#8277=CARTESIAN_POINT('Ctrl Pts',(11.971767831112,37.2869141856162,-2.23069631542371));
#8278=CARTESIAN_POINT('Ctrl Pts',(12.0205926768578,37.2980589605257,-1.95053060259384));
#8279=CARTESIAN_POINT('Ctrl Pts',(12.0595535357516,37.3092037354353,-1.6690173061836));
#8280=CARTESIAN_POINT('Ctrl Pts',(12.1003515732662,37.3208740362901,-1.37422939970866));
#8281=CARTESIAN_POINT('Ctrl Pts',(12.1303329348627,37.3325443371448,-1.07796407739402));
#8282=CARTESIAN_POINT('Ctrl Pts',(12.1494213968046,37.3442146379996,-0.781031352038081));
#8283=CARTESIAN_POINT('Ctrl Pts',(12.1685098587465,37.3558849388544,-0.484098626682174));
#8284=CARTESIAN_POINT('Ctrl Pts',(12.1767054082705,37.3675552397091,-0.186498833656002));
#8285=CARTESIAN_POINT('Ctrl Pts',(12.1739943825377,37.3792255405639,0.110955053691345));
#8286=CARTESIAN_POINT('Ctrl Pts',(12.1714048572777,37.3903728116839,0.395077902726157));
#8287=CARTESIAN_POINT('Ctrl Pts',(12.1588640971083,37.4015200828038,0.679152499465869));
#8288=CARTESIAN_POINT('Ctrl Pts',(12.1363956968827,37.4126673539238,0.962470643026071));
#8289=CARTESIAN_POINT('Ctrl Pts',(12.1139311132748,37.4238127315012,1.24574066046157));
#8290=CARTESIAN_POINT('Ctrl Pts',(12.0815422775253,37.4349581090787,1.52825421544422));
#8291=CARTESIAN_POINT('Ctrl Pts',(12.0393047783483,37.4461034866561,1.80930669153689));
#8292=CARTESIAN_POINT('Ctrl Pts',(11.9970719685101,37.4572476268389,2.09032796430773));
#8293=CARTESIAN_POINT('Ctrl Pts',(11.9449927182814,37.4683917670218,2.36988821838241));
#8294=CARTESIAN_POINT('Ctrl Pts',(11.8831942023772,37.4795359072047,2.64729027471258));
#8295=CARTESIAN_POINT('Ctrl Pts',(11.8194491765883,37.49103106195,2.93342985227278));
#8296=CARTESIAN_POINT('Ctrl Pts',(11.7453627483409,37.5025262166954,3.21727278043161));
#8297=CARTESIAN_POINT('Ctrl Pts',(11.6611312464288,37.5140213714408,3.49806636637472));
#8298=CARTESIAN_POINT('Ctrl Pts',(11.5794674609318,37.525166107437,3.77030022960688));
#8299=CARTESIAN_POINT('Ctrl Pts',(11.4882680468647,37.5363108434333,4.0396676423719));
#8300=CARTESIAN_POINT('Ctrl Pts',(11.387762605013,37.5474555794296,4.30549800857771));
#8301=CARTESIAN_POINT('Ctrl Pts',(11.282516944386,37.5591259435495,4.58386594558306));
#8302=CARTESIAN_POINT('Ctrl Pts',(11.1670664275532,37.5707963076694,4.85835486815289));
#8303=CARTESIAN_POINT('Ctrl Pts',(11.0417317581506,37.5824666717893,5.12821704211602));
#8304=CARTESIAN_POINT('Ctrl Pts',(10.916397088748,37.5941370359092,5.39807921607914));
#8305=CARTESIAN_POINT('Ctrl Pts',(10.7811784160682,37.6058074000291,5.66331434083362));
#8306=CARTESIAN_POINT('Ctrl Pts',(10.6364527948914,37.617477764149,5.92320202188377));
#8307=CARTESIAN_POINT('Ctrl Pts',(10.4982123241924,37.6286251796242,6.171444144219));
#8308=CARTESIAN_POINT('Ctrl Pts',(10.3512569086563,37.6397725950994,6.41488166047602));
#8309=CARTESIAN_POINT('Ctrl Pts',(10.1959461834747,37.6509200105746,6.65290400304169));
#8310=CARTESIAN_POINT('Ctrl Pts',(10.0406618319041,37.6620655330859,6.89088592657842));
#8311=CARTESIAN_POINT('Ctrl Pts',(9.87702514909113,37.6732110555971,7.12345428902473));
#8312=CARTESIAN_POINT('Ctrl Pts',(9.70543970866531,37.6843565781084,7.35002655175222));
#8313=CARTESIAN_POINT('Ctrl Pts',(9.53387331491802,37.6955008634215,7.57657366404129));
#8314=CARTESIAN_POINT('Ctrl Pts',(9.35436008645345,37.7066451487347,7.79712579310566));
#8315=CARTESIAN_POINT('Ctrl Pts',(9.16734533347097,37.7177894340478,8.01113161712426));
#8316=CARTESIAN_POINT('Ctrl Pts',(8.97444438432203,37.7292844801883,8.23187316782137));
#8317=CARTESIAN_POINT('Ctrl Pts',(8.77356223729382,37.7407795263289,8.44564942636432));
#8318=CARTESIAN_POINT('Ctrl Pts',(8.56523145482439,37.7522745724694,8.65189345607578));
#8319=CARTESIAN_POINT('Ctrl Pts',(8.36324692134798,37.7634194522824,8.85185480422498));
#8320=CARTESIAN_POINT('Ctrl Pts',(8.15426104066122,37.7745643320955,9.04473583466634));
#8321=CARTESIAN_POINT('Ctrl Pts',(7.93879633762425,37.7857092119086,9.23005758160391));
#8322=CARTESIAN_POINT('Ctrl Pts',(7.71317695122258,37.7973793412128,9.42411339790049));
#8323=CARTESIAN_POINT('Ctrl Pts',(7.48045361358973,37.8090494705171,9.6098800618625));
#8324=CARTESIAN_POINT('Ctrl Pts',(7.24126569578255,37.8207195998213,9.78685451884735));
#8325=CARTESIAN_POINT('Ctrl Pts',(7.00207777797537,37.8323897291256,9.96382897583221));
#8326=CARTESIAN_POINT('Ctrl Pts',(6.75642555486916,37.8440598584298,10.1320110333703));
#8327=CARTESIAN_POINT('Ctrl Pts',(6.50498479025111,37.8557299877341,10.2909486019804));
#8328=CARTESIAN_POINT('Ctrl Pts',(6.26481566441368,37.8668769660599,10.4427612842787));
#8329=CARTESIAN_POINT('Ctrl Pts',(6.01929383228136,37.8780239443856,10.5861854242557));
#8330=CARTESIAN_POINT('Ctrl Pts',(5.76902720315409,37.8891709227114,10.7208570263421));
#8331=CARTESIAN_POINT('Ctrl Pts',(5.51880378713731,37.9003159763075,10.8555053749135));
#8332=CARTESIAN_POINT('Ctrl Pts',(5.2638374446795,37.9114610299036,10.9814040766123));
#8333=CARTESIAN_POINT('Ctrl Pts',(5.00476124753254,37.9226060834997,11.0982347742872));
#8334=CARTESIAN_POINT('Ctrl Pts',(4.73415303693159,37.9342472263137,11.220265846185));
#8335=CARTESIAN_POINT('Ctrl Pts',(4.45906105304134,37.9458883691277,11.3324031528928));
#8336=CARTESIAN_POINT('Ctrl Pts',(4.18023221178463,37.9575295119417,11.4343390235535));
#8337=CARTESIAN_POINT('Ctrl Pts',(3.91331152914864,37.9686734874808,11.5319214402763));
#8338=CARTESIAN_POINT('Ctrl Pts',(3.64296676375931,37.97981746302,11.6201554471051));
#8339=CARTESIAN_POINT('Ctrl Pts',(3.36987168481286,37.9909614385591,11.6988210977815));
#8340=CARTESIAN_POINT('Ctrl Pts',(3.0967812092452,38.0021052262518,11.7774854224442));
#8341=CARTESIAN_POINT('Ctrl Pts',(2.82094076958306,38.0132490139445,11.8465816411191));
#8342=CARTESIAN_POINT('Ctrl Pts',(2.54303836545634,38.0243928016372,11.90593995121));
#8343=CARTESIAN_POINT('Ctrl Pts',(2.26510329492608,38.0355378992411,11.9653052386514));
#8344=CARTESIAN_POINT('Ctrl Pts',(1.98510603667008,38.0466829968449,12.0149302753719));
#8345=CARTESIAN_POINT('Ctrl Pts',(1.70374521241877,38.0578280944488,12.0546962840695));
#8346=CARTESIAN_POINT('Ctrl Pts',(1.66611545400818,38.0593186620551,12.060014669471));
#8347=CARTESIAN_POINT('Ctrl Pts',(1.62846131738319,38.0608092296613,12.0651567826123));
#8348=CARTESIAN_POINT('Ctrl Pts',(1.59078448392772,38.0622997972676,12.0701224093087));
#8349=CARTESIAN_POINT('Ctrl Pts',(1.59078448392775,35.0623145891265,12.0701224093086));
#8350=CARTESIAN_POINT('Ctrl Pts',(1.30904352310633,35.0734587995694,12.1072545222867));
#8351=CARTESIAN_POINT('Ctrl Pts',(1.0259830707147,35.0846030100123,12.1345202070283));
#8352=CARTESIAN_POINT('Ctrl Pts',(0.742308280011921,35.0957472204552,12.1518487756977));
#8353=CARTESIAN_POINT('Ctrl Pts',(0.447013787609849,35.1073479127754,12.1698871458912));
#8354=CARTESIAN_POINT('Ctrl Pts',(0.15105387917742,35.1189486050956,12.1771572388848));
#8355=CARTESIAN_POINT('Ctrl Pts',(-0.144772198628088,35.1305492974159,12.1736391954298));
#8356=CARTESIAN_POINT('Ctrl Pts',(-0.428971912206157,35.1416940668668,12.1702594158319));
#8357=CARTESIAN_POINT('Ctrl Pts',(-0.713047829445617,35.1528388363178,12.1569231801871));
#8358=CARTESIAN_POINT('Ctrl Pts',(-0.996292022982744,35.1639836057687,12.1336660764561));
#8359=CARTESIAN_POINT('Ctrl Pts',(-1.27954579202879,35.1751287519858,12.1104081864827));
#8360=CARTESIAN_POINT('Ctrl Pts',(-1.56196751558968,35.186273898203,12.0772287831481));
#8361=CARTESIAN_POINT('Ctrl Pts',(-1.84285396305103,35.1974190444201,12.0342153678945));
#8362=CARTESIAN_POINT('Ctrl Pts',(-2.12379262655591,35.2085662624903,11.9911939565613));
#8363=CARTESIAN_POINT('Ctrl Pts',(-2.40319518021695,35.2197134805605,11.9383349222077));
#8364=CARTESIAN_POINT('Ctrl Pts',(-2.68036673719162,35.2308606986307,11.8757772126357));
#8365=CARTESIAN_POINT('Ctrl Pts',(-2.71430555813908,35.2322256418531,11.8681172098301));
#8366=CARTESIAN_POINT('Ctrl Pts',(-2.74821094278368,35.2335905850756,11.8603118549257));
#8367=CARTESIAN_POINT('Ctrl Pts',(-2.78208162737386,35.234955528298,11.8523614553653));
#8368=CARTESIAN_POINT('Ctrl Pts',(-3.05869891833734,35.2461028346214,11.7874316195767));
#8369=CARTESIAN_POINT('Ctrl Pts',(-3.33308347439181,35.2572501409449,11.7128040752968));
#8370=CARTESIAN_POINT('Ctrl Pts',(-3.60454956580541,35.2683974472683,11.628657389297));
#8371=CARTESIAN_POINT('Ctrl Pts',(-3.87596954873944,35.2795428602232,11.5445249956007));
#8372=CARTESIAN_POINT('Ctrl Pts',(-4.14447180200817,35.2906882731782,11.4508767671221));
#8373=CARTESIAN_POINT('Ctrl Pts',(-4.40938551257707,35.3018336861331,11.3479412076145));
#8374=CARTESIAN_POINT('Ctrl Pts',(-4.67426981361024,35.3129778617741,11.2450170755525));
#8375=CARTESIAN_POINT('Ctrl Pts',(-4.93556611887974,35.3241220374151,11.1328077678666));
#8376=CARTESIAN_POINT('Ctrl Pts',(-5.19262220129422,35.3352662130561,11.0115904811533));
#8377=CARTESIAN_POINT('Ctrl Pts',(-5.45777349882183,35.3467613412917,10.8865558173052));
#8378=CARTESIAN_POINT('Ctrl Pts',(-5.71841290697268,35.3582564695273,10.7519367395924));
#8379=CARTESIAN_POINT('Ctrl Pts',(-5.97384924005414,35.3697515977629,10.6080900970488));
#8380=CARTESIAN_POINT('Ctrl Pts',(-6.22150019559629,35.3808963689756,10.4686277188988));
#8381=CARTESIAN_POINT('Ctrl Pts',(-6.46426030265943,35.3920411401884,10.320492072634));
#8382=CARTESIAN_POINT('Ctrl Pts',(-6.70152576426192,35.4031859114012,10.164054441065));
#8383=CARTESIAN_POINT('Ctrl Pts',(-6.94997956062108,35.4148562181482,10.00023993897));
#8384=CARTESIAN_POINT('Ctrl Pts',(-7.19240777343378,35.4265265248952,9.82732182100846));
#8385=CARTESIAN_POINT('Ctrl Pts',(-7.42815137572714,35.4381968316421,9.64577717912264));
#8386=CARTESIAN_POINT('Ctrl Pts',(-7.66389497802051,35.4498671383891,9.4642325372368));
#8387=CARTESIAN_POINT('Ctrl Pts',(-7.89295370933529,35.4615374451361,9.27406158308408));
#8388=CARTESIAN_POINT('Ctrl Pts',(-8.11470759005776,35.4732077518831,9.0757903775847));
#8389=CARTESIAN_POINT('Ctrl Pts',(-8.32652365126632,35.4843550580777,8.88640462404963));
#8390=CARTESIAN_POINT('Ctrl Pts',(-8.53173846022696,35.4955023642722,8.68957211823678));
#8391=CARTESIAN_POINT('Ctrl Pts',(-8.72983535399109,35.5066496704667,8.48577780419729));
#8392=CARTESIAN_POINT('Ctrl Pts',(-8.92789860102508,35.5177950832929,8.28201810459399));
#8393=CARTESIAN_POINT('Ctrl Pts',(-9.11884616072902,35.528940496119,8.07129914875044));
#8394=CARTESIAN_POINT('Ctrl Pts',(-9.30219836495137,35.5400859089451,7.85414259032112));
#8395=CARTESIAN_POINT('Ctrl Pts',(-9.48553021423546,35.5512300844576,7.63701013963763));
#8396=CARTESIAN_POINT('Ctrl Pts',(-9.66126821973614,35.56237425997,7.41344171722012));
#8397=CARTESIAN_POINT('Ctrl Pts',(-9.82897233455958,35.5735184354825,7.18399283800189));
#8398=CARTESIAN_POINT('Ctrl Pts',(-10.0019577940555,35.5850135638146,6.94731814552835));
#8399=CARTESIAN_POINT('Ctrl Pts',(-10.1663949731909,35.5965086921468,6.70438685320291));
#8400=CARTESIAN_POINT('Ctrl Pts',(-10.3218477339838,35.6080038204789,6.45584305931104));
#8401=CARTESIAN_POINT('Ctrl Pts',(-10.4725624875548,35.6191485915657,6.21487457179775));
#8402=CARTESIAN_POINT('Ctrl Pts',(-10.6148322327911,35.6302933626525,5.96863087732274));
#8403=CARTESIAN_POINT('Ctrl Pts',(-10.7483044718205,35.6414381337393,5.71772692868804));
#8404=CARTESIAN_POINT('Ctrl Pts',(-10.8880706444308,35.6531084406941,5.45499151008326));
#8405=CARTESIAN_POINT('Ctrl Pts',(-11.0181894980664,35.6647787476489,5.18714603041487));
#8406=CARTESIAN_POINT('Ctrl Pts',(-11.1383106735327,35.6764490546037,4.91492477967551));
#8407=CARTESIAN_POINT('Ctrl Pts',(-11.2584318489989,35.6881193615585,4.64270352893615));
#8408=CARTESIAN_POINT('Ctrl Pts',(-11.3685552188829,35.6997896685134,4.36610681761556));
#8409=CARTESIAN_POINT('Ctrl Pts',(-11.4683881438355,35.7114599754682,4.08589324778976));
#8410=CARTESIAN_POINT('Ctrl Pts',(-11.5636605180159,35.7225971614369,3.81848034680994));
#8411=CARTESIAN_POINT('Ctrl Pts',(-11.6495908466594,35.7337343474056,3.54769134091233));
#8412=CARTESIAN_POINT('Ctrl Pts',(-11.7259574475739,35.7448715333744,3.27419794570916));
#8413=CARTESIAN_POINT('Ctrl Pts',(-11.8023132777083,35.7560071485493,3.00074312413884));
#8414=CARTESIAN_POINT('Ctrl Pts',(-11.8691079996121,35.7671427637243,2.72458493211118));
#8415=CARTESIAN_POINT('Ctrl Pts',(-11.9261699500892,35.7782783788992,2.44640973093008));
#8416=CARTESIAN_POINT('Ctrl Pts',(-11.9832242232964,35.7894124958583,2.16827195619616));
#8417=CARTESIAN_POINT('Ctrl Pts',(-12.0305482866717,35.8005466128173,1.88811797652426));
#8418=CARTESIAN_POINT('Ctrl Pts',(-12.0680214761787,35.8116807297764,1.60664492047536));
#8419=CARTESIAN_POINT('Ctrl Pts',(-12.1054959778234,35.8228152366007,1.32516200854266));
#8420=CARTESIAN_POINT('Ctrl Pts',(-12.1331188783859,35.833949743425,1.04236019299949));
#8421=CARTESIAN_POINT('Ctrl Pts',(-12.1508211493447,35.8450842502493,0.758943770405247));
#8422=CARTESIAN_POINT('Ctrl Pts',(-12.1666082922634,35.8550141655112,0.506188879272841));
#8423=CARTESIAN_POINT('Ctrl Pts',(-12.1745059239959,35.864944080773,0.252945394476219));
#8424=CARTESIAN_POINT('Ctrl Pts',(-12.1744999966649,35.8748739960349,-0.000284966977105543));
#8425=CARTESIAN_POINT('',(-12.1744999990795,35.6251260039956,-0.000149711562892353));
#8426=CARTESIAN_POINT('Ctrl Pts',(1.59078448392778,34.8125669141531,12.0701224093086));
#8427=CARTESIAN_POINT('Ctrl Pts',(1.3090559178938,34.8237119930029,12.1072528887129));
#8428=CARTESIAN_POINT('Ctrl Pts',(1.02599923070556,34.8348570718527,12.1345189599205));
#8429=CARTESIAN_POINT('Ctrl Pts',(0.742319374086524,34.8460021507025,12.1518480979996));
#8430=CARTESIAN_POINT('Ctrl Pts',(0.45866727424099,34.8571461390574,12.1691755405019));
#8431=CARTESIAN_POINT('Ctrl Pts',(0.174392392915168,34.8682901274123,12.1765679752301));
#8432=CARTESIAN_POINT('Ctrl Pts',(-0.109796879691469,34.8794341157672,12.1740048831603));
#8433=CARTESIAN_POINT('Ctrl Pts',(-0.394010203114441,34.8905790472331,12.1714415741771));
#8434=CARTESIAN_POINT('Ctrl Pts',(-0.678137636520358,34.901723978699,12.1589210539924));
#8435=CARTESIAN_POINT('Ctrl Pts',(-0.96147096144561,34.9128689101649,12.1364749346875));
#8436=CARTESIAN_POINT('Ctrl Pts',(-1.24480084680939,34.9240137063354,12.1140290878701));
#8437=CARTESIAN_POINT('Ctrl Pts',(-1.52733637715058,34.9351585025059,12.0816579059211));
#8438=CARTESIAN_POINT('Ctrl Pts',(-1.80837370794537,34.9463032986765,12.0394449532531));
#8439=CARTESIAN_POINT('Ctrl Pts',(-2.08947599074481,34.957450670579,11.9972222445293));
#8440=CARTESIAN_POINT('Ctrl Pts',(-2.36907911783929,34.9685980424816,11.9451532576149));
#8441=CARTESIAN_POINT('Ctrl Pts',(-2.64648707988667,34.9797454143842,11.8833731064035));
#8442=CARTESIAN_POINT('Ctrl Pts',(-2.89654218866479,34.9897936382099,11.8276845734663));
#8443=CARTESIAN_POINT('Ctrl Pts',(-3.14481365690257,34.9998418620356,11.7641062220393));
#8444=CARTESIAN_POINT('Ctrl Pts',(-3.39080016893301,35.0098900858613,11.6927723173063));
#8445=CARTESIAN_POINT('Ctrl Pts',(-3.66369287414124,35.0210373921087,11.6136358554125));
#8446=CARTESIAN_POINT('Ctrl Pts',(-3.93385472728386,35.0321846983561,11.5249300100742));
#8447=CARTESIAN_POINT('Ctrl Pts',(-4.2006101415968,35.0433320046035,11.4268685425323));
#8448=CARTESIAN_POINT('Ctrl Pts',(-4.46732024753654,35.0544774174824,11.3288237307182));
#8449=CARTESIAN_POINT('Ctrl Pts',(-4.73062481951636,35.0656228303613,11.2214265612428));
#8450=CARTESIAN_POINT('Ctrl Pts',(-4.98986574788541,35.0767682432401,11.1049398948432));
#8451=CARTESIAN_POINT('Ctrl Pts',(-5.24907789648335,35.087912418805,10.9884661602735));
#8452=CARTESIAN_POINT('Ctrl Pts',(-5.50422705905017,35.0990565943698,10.8629050530442));
#8453=CARTESIAN_POINT('Ctrl Pts',(-5.75467620310551,35.1102007699347,10.7285671013147));
#8454=CARTESIAN_POINT('Ctrl Pts',(-6.01301249949139,35.1216958982273,10.5899985745793));
#8455=CARTESIAN_POINT('Ctrl Pts',(-6.26634768811219,35.13319102652,10.4420915758961));
#8456=CARTESIAN_POINT('Ctrl Pts',(-6.51400994570775,35.1446861548126,10.2852381925369));
#8457=CARTESIAN_POINT('Ctrl Pts',(-6.75412376698239,35.1558309259505,10.1331655044178));
#8458=CARTESIAN_POINT('Ctrl Pts',(-6.98890510846411,35.1669756970883,9.97268385469279));
#8459=CARTESIAN_POINT('Ctrl Pts',(-7.21777016470715,35.1781204682262,9.80419522956695));
#8460=CARTESIAN_POINT('Ctrl Pts',(-7.45742743582955,35.1897907750962,9.6277614621073));
#8461=CARTESIAN_POINT('Ctrl Pts',(-7.69059677083969,35.2014610819663,9.44254759390848));
#8462=CARTESIAN_POINT('Ctrl Pts',(-7.9166446754192,35.2131313888363,9.24906413282754));
#8463=CARTESIAN_POINT('Ctrl Pts',(-8.14269257999871,35.2248016957063,9.05558067174661));
#8464=CARTESIAN_POINT('Ctrl Pts',(-8.36161880497301,35.2364720025764,8.85382784261666));
#8465=CARTESIAN_POINT('Ctrl Pts',(-8.57283138154773,35.2481423094464,8.64436303920366));
#8466=CARTESIAN_POINT('Ctrl Pts',(-8.7745785421954,35.2592896156963,8.44428532588983));
#8467=CARTESIAN_POINT('Ctrl Pts',(-8.96934848056512,35.2704369219463,8.23711190810849));
#8468=CARTESIAN_POINT('Ctrl Pts',(-9.15665028193266,35.2815842281962,8.02335377908656));
#8469=CARTESIAN_POINT('Ctrl Pts',(-9.34392027011314,35.2927296410776,7.80963195685556));
#8470=CARTESIAN_POINT('Ctrl Pts',(-9.52372447804811,35.303875053959,7.58932785684307));
#8471=CARTESIAN_POINT('Ctrl Pts',(-9.69561083324766,35.3150204668404,7.36298722124455));
#8472=CARTESIAN_POINT('Ctrl Pts',(-9.8674781063922,35.3261646424078,7.13667171297192));
#8473=CARTESIAN_POINT('Ctrl Pts',(-10.0314291207498,35.3373088179753,6.90432121967417));
#8474=CARTESIAN_POINT('Ctrl Pts',(-10.1870531218382,35.3484529935428,6.66651325228162));
#8475=CARTESIAN_POINT('Ctrl Pts',(-10.3475780388049,35.3599481218335,6.42121622899009));
#8476=CARTESIAN_POINT('Ctrl Pts',(-10.4992428040734,35.3714432501243,6.17011267067247));
#8477=CARTESIAN_POINT('Ctrl Pts',(-10.6416451441391,35.382938378415,5.91386835127568));
#8478=CARTESIAN_POINT('Ctrl Pts',(-10.7797072387721,35.3940831495554,5.6654340386276));
#8479=CARTESIAN_POINT('Ctrl Pts',(-10.9090630261503,35.4052279206958,5.41216793644504));
#8480=CARTESIAN_POINT('Ctrl Pts',(-11.0293922551297,35.4163726918363,5.15470239029231));
#8481=CARTESIAN_POINT('Ctrl Pts',(-11.1553956525465,35.4280429987021,4.8850959629249));
#8482=CARTESIAN_POINT('Ctrl Pts',(-11.2715005718733,35.439713305568,4.61088479720244));
#8483=CARTESIAN_POINT('Ctrl Pts',(-11.3773950641872,35.4513836124339,4.33282030592177));
#8484=CARTESIAN_POINT('Ctrl Pts',(-11.4832895565011,35.4630539192998,4.05475581464107));
#8485=CARTESIAN_POINT('Ctrl Pts',(-11.578973510603,35.4747242261657,3.77283831446075));
#8486=CARTESIAN_POINT('Ctrl Pts',(-11.6641938765588,35.4863945330316,3.48784051528297));
#8487=CARTESIAN_POINT('Ctrl Pts',(-11.7486157263752,35.4979554889427,3.20551314986525));
#8488=CARTESIAN_POINT('Ctrl Pts',(-11.8227942500949,35.5095164448538,2.92007971671269));
#8489=CARTESIAN_POINT('Ctrl Pts',(-11.8865239621894,35.521077400765,2.63229906095355));
#8490=CARTESIAN_POINT('Ctrl Pts',(-11.9482806334632,35.5322804351166,2.35342795401509));
#8491=CARTESIAN_POINT('Ctrl Pts',(-12.0002256656454,35.5434834694682,2.07235304358251));
#8492=CARTESIAN_POINT('Ctrl Pts',(-12.042223537602,35.5546865038198,1.78977722647935));
#8493=CARTESIAN_POINT('Ctrl Pts',(-12.0862340710423,35.5664264205107,1.49365954554348));
#8494=CARTESIAN_POINT('Ctrl Pts',(-12.119320691996,35.5781663372016,1.19589388457444));
#8495=CARTESIAN_POINT('Ctrl Pts',(-12.1413881016093,35.5899062538925,0.897298844366037));
#8496=CARTESIAN_POINT('Ctrl Pts',(-12.1634555112226,35.6016461705834,0.598703804157665));
#8497=CARTESIAN_POINT('Ctrl Pts',(-12.1745036811867,35.6133860872742,0.299279713519359));
#8498=CARTESIAN_POINT('Ctrl Pts',(-12.1744999990795,35.6251260039651,-0.00014971078451594));
#8499=CARTESIAN_POINT('Ctrl Pts',(-12.1744999990795,35.6251260039956,-0.000149711562934393));
#8500=CARTESIAN_POINT('Ctrl Pts',(-12.174496426179,35.6365176701443,-0.290696921273105));
#8501=CARTESIAN_POINT('Ctrl Pts',(-12.1640875501384,35.647909336293,-0.58120652559487));
#8502=CARTESIAN_POINT('Ctrl Pts',(-12.1433074390434,35.6593010024416,-0.870938970808622));
#8503=CARTESIAN_POINT('Ctrl Pts',(-12.1225204619165,35.670696432552,-1.16076714756995));
#8504=CARTESIAN_POINT('Ctrl Pts',(-12.0913554174435,35.6820918626624,-1.44981741179922));
#8505=CARTESIAN_POINT('Ctrl Pts',(-12.0498983619847,35.6934872927729,-1.73735422865857));
#8506=CARTESIAN_POINT('Ctrl Pts',(-12.0121118806754,35.7038737807208,-1.99943276838512));
#8507=CARTESIAN_POINT('Ctrl Pts',(-11.9657758328564,35.7142602686687,-2.26025391982292));
#8508=CARTESIAN_POINT('Ctrl Pts',(-11.9109926366114,35.7246467566166,-2.51926669104116));
#8509=CARTESIAN_POINT('Ctrl Pts',(-11.8521965285982,35.7357940628915,-2.79725234936639));
#8510=CARTESIAN_POINT('Ctrl Pts',(-11.783655703664,35.7469413691664,-3.0732202996823));
#8511=CARTESIAN_POINT('Ctrl Pts',(-11.7055335188614,35.7580886754414,-3.34648103069664));
#8512=CARTESIAN_POINT('Ctrl Pts',(-11.6274246031012,35.7692340883479,-3.61969534841323));
#8513=CARTESIAN_POINT('Ctrl Pts',(-11.5397376498562,35.7803795012544,-3.89020310848564));
#8514=CARTESIAN_POINT('Ctrl Pts',(-11.4426862708534,35.7915249141608,-4.15732860823185));
#8515=CARTESIAN_POINT('Ctrl Pts',(-11.3456456660616,35.8026690897533,-4.42442445289702));
#8516=CARTESIAN_POINT('Ctrl Pts',(-11.2392428024865,35.8138132653458,-4.68813853636811));
#8517=CARTESIAN_POINT('Ctrl Pts',(-11.1237403838462,35.8249574409383,-4.94781266043789));
#8518=CARTESIAN_POINT('Ctrl Pts',(-11.004600559911,35.8364525692102,-5.21566444905335));
#8519=CARTESIAN_POINT('Ctrl Pts',(-10.8757788785789,35.8479476974822,-5.47921742693672));
#8520=CARTESIAN_POINT('Ctrl Pts',(-10.7376168148967,35.8594428257542,-5.73777268514943));
#8521=CARTESIAN_POINT('Ctrl Pts',(-10.6036657578032,35.8705875969194,-5.98844750305287));
#8522=CARTESIAN_POINT('Ctrl Pts',(-10.4609353850308,35.8817323680846,-6.23442449239448));
#8523=CARTESIAN_POINT('Ctrl Pts',(-10.30978353461,35.8928771392499,-6.47509179235978));
#8524=CARTESIAN_POINT('Ctrl Pts',(-10.1515040647607,35.9045474460752,-6.72710784471055));
#8525=CARTESIAN_POINT('Ctrl Pts',(-9.98398994001832,35.9162177529005,-6.97330112872041));
#8526=CARTESIAN_POINT('Ctrl Pts',(-9.80770356017696,35.9278880597258,-7.21300222692966));
#8527=CARTESIAN_POINT('Ctrl Pts',(-9.63141718033562,35.9395583665511,-7.45270332513889));
#8528=CARTESIAN_POINT('Ctrl Pts',(-9.4463587512404,35.9512286733765,-7.68591197247079));
#8529=CARTESIAN_POINT('Ctrl Pts',(-9.25304049328369,35.9628989802018,-7.91199670624631));
#8530=CARTESIAN_POINT('Ctrl Pts',(-9.06838572400005,35.9740462863956,-8.12794953343979));
#8531=CARTESIAN_POINT('Ctrl Pts',(-8.87614002640509,35.9851935925894,-8.33746742022859));
#8532=CARTESIAN_POINT('Ctrl Pts',(-8.67677679908099,35.9963408987832,-8.54002310470703));
#8533=CARTESIAN_POINT('Ctrl Pts',(-8.47744743357855,36.0074863116083,-8.74254438512533));
#8534=CARTESIAN_POINT('Ctrl Pts',(-8.27100313898243,36.0186317244334,-8.93810563411376));
#8535=CARTESIAN_POINT('Ctrl Pts',(-8.05795483269958,36.0297771372585,-9.1262157636215));
#8536=CARTESIAN_POINT('Ctrl Pts',(-7.84493017808824,36.0409213127697,-9.31430500998273));
#8537=CARTESIAN_POINT('Ctrl Pts',(-7.62530317567703,36.0520654882808,-9.49494461212312));
#8538=CARTESIAN_POINT('Ctrl Pts',(-7.39961947215846,36.063209663792,-9.66768234466014));
#8539=CARTESIAN_POINT('Ctrl Pts',(-7.16682852840535,36.0747047921249,-9.84585994079197));
#8540=CARTESIAN_POINT('Ctrl Pts',(-6.9275934559246,36.0861999204578,-10.0156297224767));
#8541=CARTESIAN_POINT('Ctrl Pts',(-6.68254854954543,36.0976950487907,-10.1765414131211));
#8542=CARTESIAN_POINT('Ctrl Pts',(-6.44497230785367,36.1088398198755,-10.3325487150986));
#8543=CARTESIAN_POINT('Ctrl Pts',(-6.2019353743058,36.1199845909603,-10.4802297442823));
#8544=CARTESIAN_POINT('Ctrl Pts',(-5.95404475521485,36.1311293620451,-10.6192184883304));
#8545=CARTESIAN_POINT('Ctrl Pts',(-5.69446476074719,36.1427996690021,-10.7647612988788));
#8546=CARTESIAN_POINT('Ctrl Pts',(-5.429562588848,36.154469975959,-10.9007721676023));
#8547=CARTESIAN_POINT('Ctrl Pts',(-5.16006460113188,36.166140282916,-11.0268845809751));
#8548=CARTESIAN_POINT('Ctrl Pts',(-4.89056661341578,36.1778105898729,-11.1529969943479));
#8549=CARTESIAN_POINT('Ctrl Pts',(-4.61647311747857,36.1894808968299,-11.2692108181213));
#8550=CARTESIAN_POINT('Ctrl Pts',(-4.33853605764074,36.2011512037868,-11.3752167067951));
#8551=CARTESIAN_POINT('Ctrl Pts',(-4.07305464777408,36.2122985101097,-11.4764719794663));
#8552=CARTESIAN_POINT('Ctrl Pts',(-3.80398730860846,36.2234458164327,-11.5684443772484));
#8553=CARTESIAN_POINT('Ctrl Pts',(-3.53200203188287,36.2345931227556,-11.6508974717305));
#8554=CARTESIAN_POINT('Ctrl Pts',(-3.26006295181857,36.2457385357101,-11.7333365615659));
#8555=CARTESIAN_POINT('Ctrl Pts',(-2.98520717886023,36.2568839486646,-11.8062594987885));
#8556=CARTESIAN_POINT('Ctrl Pts',(-2.70811833795219,36.2680293616191,-11.8694795723169));
#8557=CARTESIAN_POINT('Ctrl Pts',(-2.43106025821149,36.2791735372596,-11.9326926274346));
#8558=CARTESIAN_POINT('Ctrl Pts',(-2.1517698655459,36.2903177129001,-11.9862049104721));
#8559=CARTESIAN_POINT('Ctrl Pts',(-1.87094268199846,36.3014618885405,-12.0298804537151));
#8560=CARTESIAN_POINT('Ctrl Pts',(-1.5812716833385,36.3129570167765,-12.0749314280132));
#8561=CARTESIAN_POINT('Ctrl Pts',(-1.28996582371931,36.3244521450124,-12.1095160101662));
#8562=CARTESIAN_POINT('Ctrl Pts',(-0.997797531322615,36.3359472732484,-12.1335423655455));
#8563=CARTESIAN_POINT('Ctrl Pts',(-0.714534160316956,36.3470920444607,-12.1568364278884));
#8564=CARTESIAN_POINT('Ctrl Pts',(-0.430460427915619,36.358236815673,-12.1702063130348));
#8565=CARTESIAN_POINT('Ctrl Pts',(-0.146284477231075,36.3693815868853,-12.1736211170597));
#8566=CARTESIAN_POINT('Ctrl Pts',(0.151291888549954,36.3810518936331,-12.1771969473476));
#8567=CARTESIAN_POINT('Ctrl Pts',(0.448980027019182,36.3927222003809,-12.169856231212));
#8568=CARTESIAN_POINT('Ctrl Pts',(0.745966753667841,36.4043925071286,-12.1516247412608));
#8569=CARTESIAN_POINT('Ctrl Pts',(1.04295348031647,36.4160628138764,-12.1333932513097));
#8570=CARTESIAN_POINT('Ctrl Pts',(1.33923846081193,36.4277331206241,-12.1042710168617));
#8571=CARTESIAN_POINT('Ctrl Pts',(1.63401340472503,36.4394034273719,-12.0643462501363));
#8572=CARTESIAN_POINT('Ctrl Pts',(1.91557811671966,36.4505507335666,-12.0262106973134));
#8573=CARTESIAN_POINT('Ctrl Pts',(2.19584925314808,36.4616980397613,-11.9782081635445));
#8574=CARTESIAN_POINT('Ctrl Pts',(2.47412713324821,36.4728453459559,-11.9204507120547));
#8575=CARTESIAN_POINT('Ctrl Pts',(2.75235774788912,36.4839907587822,-11.8627030706599));
#8576=CARTESIAN_POINT('Ctrl Pts',(3.02859552104343,36.4951361716085,-11.7952038736759));
#8577=CARTESIAN_POINT('Ctrl Pts',(3.30215083685498,36.5062815844348,-11.7181163204953));
#8578=CARTESIAN_POINT('Ctrl Pts',(3.57567578378372,36.5174257599474,-11.6410373252286));
#8579=CARTESIAN_POINT('Ctrl Pts',(3.84651861133585,36.52856993546,-11.5543721716479));
#8580=CARTESIAN_POINT('Ctrl Pts',(4.11400354010584,36.5397141109726,-11.4583343083538));
#8581=CARTESIAN_POINT('Ctrl Pts',(4.38991211491443,36.5512092393046,-11.3592720168407));
#8582=CARTESIAN_POINT('Ctrl Pts',(4.66224758709874,36.5627043676366,-11.250237209273));
#8583=CARTESIAN_POINT('Ctrl Pts',(4.93028776824498,36.5741994959687,-11.1315188888262));
#8584=CARTESIAN_POINT('Ctrl Pts',(5.19015841733053,36.5853442670556,-11.0164189554471));
#8585=CARTESIAN_POINT('Ctrl Pts',(5.44599147331901,36.5964890381425,-10.8922171642219));
#8586=CARTESIAN_POINT('Ctrl Pts',(5.69715035220492,36.6076338092294,-10.7592252562334));
#8587=CARTESIAN_POINT('Ctrl Pts',(5.96015272238509,36.619304116184,-10.6199620648587));
#8588=CARTESIAN_POINT('Ctrl Pts',(6.21802920235262,36.6309744231386,-10.4710599556509));
#8589=CARTESIAN_POINT('Ctrl Pts',(6.47007809708769,36.6426447300932,-10.3129307021615));
#8590=CARTESIAN_POINT('Ctrl Pts',(6.72212699182275,36.6543150370478,-10.1548014486722));
#8591=CARTESIAN_POINT('Ctrl Pts',(6.96834802179005,36.6659853440024,-9.98744523663738));
#8592=CARTESIAN_POINT('Ctrl Pts',(7.20807366931145,36.677655650957,-9.81132632358027));
#8593=CARTESIAN_POINT('Ctrl Pts',(7.43705609365123,36.6888029570834,-9.64310011958052));
#8594=CARTESIAN_POINT('Ctrl Pts',(7.66018090385868,36.6999502632097,-9.46682910328908));
#8595=CARTESIAN_POINT('Ctrl Pts',(7.8768873622909,36.711097569336,-9.2829465005343));
#8596=CARTESIAN_POINT('Ctrl Pts',(8.0935570131396,36.7222429820928,-9.09909513023244));
#8597=CARTESIAN_POINT('Ctrl Pts',(8.3038102853956,36.7333883948497,-8.90763492711705));
#8598=CARTESIAN_POINT('Ctrl Pts',(8.50711974988999,36.7445338076065,-8.70903920137186));
#8599=CARTESIAN_POINT('Ctrl Pts',(8.71040664386375,36.7556779830487,-8.51046552284879));
#8600=CARTESIAN_POINT('Ctrl Pts',(8.9067510786137,36.7668221584909,-8.30475808984803));
#8601=CARTESIAN_POINT('Ctrl Pts',(9.09566182065551,36.7779663339332,-8.09242771325575));
#8602=CARTESIAN_POINT('Ctrl Pts',(9.29052174942825,36.7894614623172,-7.87341061760588));
#8603=CARTESIAN_POINT('Ctrl Pts',(9.47747198957374,36.8009565907013,-7.64734689392032));
#8604=CARTESIAN_POINT('Ctrl Pts',(9.65601671358983,36.8124517190854,-7.41483590357021));
#8605=CARTESIAN_POINT('Ctrl Pts',(9.82911961410876,36.8235964901005,-7.18941156211219));
#8606=CARTESIAN_POINT('Ctrl Pts',(9.99432162080455,36.8347412611157,-6.95792736516624));
#8607=CARTESIAN_POINT('Ctrl Pts',(10.1512129534238,36.8458860321308,-6.72096167406424));
#8608=CARTESIAN_POINT('Ctrl Pts',(10.3155025584388,36.8575563391994,-6.47282177274978));
#8609=CARTESIAN_POINT('Ctrl Pts',(10.4706786683875,36.8692266462679,-6.21867123920136));
#8610=CARTESIAN_POINT('Ctrl Pts',(10.616322201149,36.8808969533365,-5.95920742812246));
#8611=CARTESIAN_POINT('Ctrl Pts',(10.7619657339106,36.892567260405,-5.69974361704354));
#8612=CARTESIAN_POINT('Ctrl Pts',(10.8980765329177,36.9042375674736,-5.43496682529208));
#8613=CARTESIAN_POINT('Ctrl Pts',(11.0242906417777,36.9159078745421,-5.16560413655685));
#8614=CARTESIAN_POINT('Ctrl Pts',(11.1448485153909,36.9270551814265,-4.90831282991925));
#8615=CARTESIAN_POINT('Ctrl Pts',(11.2564132397565,36.9382024883108,-4.64676077901756));
#8616=CARTESIAN_POINT('Ctrl Pts',(11.3586997682256,36.9493497951952,-4.38159672098112));
#8617=CARTESIAN_POINT('Ctrl Pts',(11.4609689233679,36.9604952087139,-4.11647770095597));
#8618=CARTESIAN_POINT('Ctrl Pts',(11.5539629329279,36.9716406222325,-3.84774814742302));
#8619=CARTESIAN_POINT('Ctrl Pts',(11.6374451793146,36.9827860357512,-3.57607605462302));
#8620=CARTESIAN_POINT('Ctrl Pts',(11.7209181578842,36.993930211957,-3.30443412161603));
#8621=CARTESIAN_POINT('Ctrl Pts',(11.7948814035168,37.0050743881628,-3.0298505565593));
#8622=CARTESIAN_POINT('Ctrl Pts',(11.8591480264475,37.0162185643687,-2.75300896053869));
#8623=CARTESIAN_POINT('Ctrl Pts',(11.9254385293134,37.0277136921819,-2.46744908859368));
#8624=CARTESIAN_POINT('Ctrl Pts',(11.9814117057185,37.0392088199951,-2.17948694843925));
#8625=CARTESIAN_POINT('Ctrl Pts',(12.0269190072912,37.0507039478083,-1.88988609234979));
#8626=CARTESIAN_POINT('Ctrl Pts',(12.0710393075008,37.061848719582,-1.60911188095882));
#8627=CARTESIAN_POINT('Ctrl Pts',(12.1053222141113,37.0729934913558,-1.32679764185019));
#8628=CARTESIAN_POINT('Ctrl Pts',(12.129684684297,37.0841382631295,-1.04364731089197));
#8629=CARTESIAN_POINT('Ctrl Pts',(12.1551959718931,37.0958085689624,-0.747144966467611));
#8630=CARTESIAN_POINT('Ctrl Pts',(12.1698286831205,37.1074788747954,-0.44972609738708));
#8631=CARTESIAN_POINT('Ctrl Pts',(12.1735485509352,37.1191491806283,-0.152203574280096));
#8632=CARTESIAN_POINT('Ctrl Pts',(12.1772684187499,37.1308194864613,0.145318948826918));
#8633=CARTESIAN_POINT('Ctrl Pts',(12.170075447735,37.1424897922942,0.442944790376295));
#8634=CARTESIAN_POINT('Ctrl Pts',(12.1519980013252,37.1541600981272,0.73986135578836));
#8635=CARTESIAN_POINT('Ctrl Pts',(12.134730690394,37.1653074026142,1.02347169207873));
#8636=CARTESIAN_POINT('Ctrl Pts',(12.1075278724749,37.1764547071013,1.30651963043172));
#8637=CARTESIAN_POINT('Ctrl Pts',(12.0704497066061,37.1876020115883,1.58829913123846));
#8638=CARTESIAN_POINT('Ctrl Pts',(12.0333778384804,37.1987474227007,1.87003077167098));
#8639=CARTESIAN_POINT('Ctrl Pts',(11.9864340059855,37.2098928338131,2.15049414032514));
#8640=CARTESIAN_POINT('Ctrl Pts',(11.9297301073365,37.2210382449255,2.4289894639765));
#8641=CARTESIAN_POINT('Ctrl Pts',(11.8730325037096,37.2321824187225,2.70745387027918));
#8642=CARTESIAN_POINT('Ctrl Pts',(11.806577050753,37.2433265925194,2.98395040653923));
#8643=CARTESIAN_POINT('Ctrl Pts',(11.730526779452,37.2544707663164,3.25778939260328));
#8644=CARTESIAN_POINT('Ctrl Pts',(11.6520815091351,37.2659658959327,3.5402522019744));
#8645=CARTESIAN_POINT('Ctrl Pts',(11.563427371625,37.277461025549,3.81988707545358));
#8646=CARTESIAN_POINT('Ctrl Pts',(11.4647993244373,37.2889561551654,4.09595247779841));
#8647=CARTESIAN_POINT('Ctrl Pts',(11.3691773629799,37.3001009245536,4.36360367860211));
#8648=CARTESIAN_POINT('Ctrl Pts',(11.2641805724472,37.3112456939418,4.6278995113326));
#8649=CARTESIAN_POINT('Ctrl Pts',(11.1500728991938,37.3223904633301,4.88818213579082));
#8650=CARTESIAN_POINT('Ctrl Pts',(11.0305843891053,37.3340607730604,5.16073859156343));
#8651=CARTESIAN_POINT('Ctrl Pts',(10.9011051867154,37.3457310827908,5.4288939487069));
#8652=CARTESIAN_POINT('Ctrl Pts',(10.7619941971752,37.3574013925212,5.6919180554509));
#8653=CARTESIAN_POINT('Ctrl Pts',(10.622883207635,37.3690717022515,5.95494216219492));
#8654=CARTESIAN_POINT('Ctrl Pts',(10.4741405955607,37.3807420119819,6.21283472606724));
#8655=CARTESIAN_POINT('Ctrl Pts',(10.3161801276997,37.3924123217123,6.46489580912594));
#8656=CARTESIAN_POINT('Ctrl Pts',(10.1652985893882,37.4035596315964,6.70566088456128));
#8657=CARTESIAN_POINT('Ctrl Pts',(10.0059621610874,37.4147069414806,6.94117756831538));
#8658=CARTESIAN_POINT('Ctrl Pts',(9.83856153689548,37.4258542513647,7.17085470043292));
#8659=CARTESIAN_POINT('Ctrl Pts',(9.67118934551754,37.4369996678904,7.40049282213932));
#8660=CARTESIAN_POINT('Ctrl Pts',(9.49575584989997,37.448145084416,7.62429315693641));
#8661=CARTESIAN_POINT('Ctrl Pts',(9.31269417572409,37.4592905009417,7.84169480657305));
#8662=CARTESIAN_POINT('Ctrl Pts',(9.12965282422266,37.4704346801539,8.05907232126735));
#8663=CARTESIAN_POINT('Ctrl Pts',(8.93898515694895,37.4815788593662,8.27005236527153));
#8664=CARTESIAN_POINT('Ctrl Pts',(8.74116436747306,37.4927230385784,8.47410737191944));
#8665=CARTESIAN_POINT('Ctrl Pts',(8.53711391475835,37.5042181641383,8.68458836633626));
#8666=CARTESIAN_POINT('Ctrl Pts',(8.32545271468949,37.5157132896982,8.88770087711788));
#8667=CARTESIAN_POINT('Ctrl Pts',(8.10674193044595,37.5272084152581,9.08290622670682));
#8668=CARTESIAN_POINT('Ctrl Pts',(7.89469705879945,37.5383531899996,9.27216206720623));
#8669=CARTESIAN_POINT('Ctrl Pts',(7.67602616543322,37.549497964741,9.45398541568647));
#8670=CARTESIAN_POINT('Ctrl Pts',(7.45127581728952,37.5606427394824,9.62792495528899));
#8671=CARTESIAN_POINT('Ctrl Pts',(7.21592747991899,37.5723130404516,9.81006652608769));
#8672=CARTESIAN_POINT('Ctrl Pts',(6.9739127963806,37.5839833414207,9.98356268944996));
#8673=CARTESIAN_POINT('Ctrl Pts',(6.72589631532788,37.5956536423899,10.1479440777657));
#8674=CARTESIAN_POINT('Ctrl Pts',(6.47787983427515,37.6073239433591,10.3123254660813));
#8675=CARTESIAN_POINT('Ctrl Pts',(6.22386184020968,37.6189942443282,10.4675919013181));
#8676=CARTESIAN_POINT('Ctrl Pts',(5.96454059505376,37.6306645452974,10.6133267988862));
#8677=CARTESIAN_POINT('Ctrl Pts',(5.71684316802239,37.6418117365775,10.7525292739267));
#8678=CARTESIAN_POINT('Ctrl Pts',(5.46423348683355,37.6529589278576,10.8830774824776));
#8679=CARTESIAN_POINT('Ctrl Pts',(5.20733748166243,37.6641061191377,11.0046393217621));
#8680=CARTESIAN_POINT('Ctrl Pts',(4.95048636431727,37.6752513626523,11.1261799203634));
#8681=CARTESIAN_POINT('Ctrl Pts',(4.68935065937322,37.6863966061668,11.2387371707387));
#8682=CARTESIAN_POINT('Ctrl Pts',(4.42457906275146,37.6975418496814,11.3420258493561));
#8683=CARTESIAN_POINT('Ctrl Pts',(4.15982285196366,37.7086864455477,11.4453085258853));
#8684=CARTESIAN_POINT('Ctrl Pts',(3.89143141911817,37.719831041414,11.5393236073228));
#8685=CARTESIAN_POINT('Ctrl Pts',(3.62007279718327,37.7309756372803,11.6238342724375));
#8686=CARTESIAN_POINT('Ctrl Pts',(3.34873426985421,37.7421194078688,11.7083386793819));
#8687=CARTESIAN_POINT('Ctrl Pts',(3.07442924725578,37.7532631784572,11.7833399974053));
#8688=CARTESIAN_POINT('Ctrl Pts',(2.79784129946167,37.7644069490457,11.8486511600699));
#8689=CARTESIAN_POINT('Ctrl Pts',(2.52123406790476,37.7755514965798,11.9139668762409));
#8690=CARTESIAN_POINT('Ctrl Pts',(2.24234385257215,37.786696044114,11.9695910250927));
#8691=CARTESIAN_POINT('Ctrl Pts',(1.96186619748412,37.7978405916482,12.0153872710441));
#8692=CARTESIAN_POINT('Ctrl Pts',(1.83845955010879,37.8027440526647,12.035537044378));
#8693=CARTESIAN_POINT('Ctrl Pts',(1.71474572240879,37.8076475136811,12.0537849101436));
#8694=CARTESIAN_POINT('Ctrl Pts',(1.59078448392769,37.8125509746976,12.0701224093087));
#8695=CARTESIAN_POINT('Origin',(0.,20.,0.));
#8696=CARTESIAN_POINT('',(-9.83900047314216,22.8294636018362,-3.67173622267202));
#8697=CARTESIAN_POINT('',(-9.83826089695889,22.011121265682,-3.67146067980712));
#8698=CARTESIAN_POINT('',(-9.83826089695937,20.,-3.67146067980583));
#8699=CARTESIAN_POINT('',(-10.5009999965284,22.6589303284762,0.000270018945713324));
#8700=CARTESIAN_POINT('Ctrl Pts',(-10.5010864010386,22.6589303319738,0.000269944245985663));
#8701=CARTESIAN_POINT('Ctrl Pts',(-10.4997937395166,22.7157747552614,-1.24986959862917));
#8702=CARTESIAN_POINT('Ctrl Pts',(-10.2752983162086,22.7726191785488,-2.50045949815336));
#8703=CARTESIAN_POINT('Ctrl Pts',(-9.8390004731412,22.8294636018363,-3.6717362226746));
#8704=CARTESIAN_POINT('',(-7.93387242656103,20.0000000365693,-6.87929279207206));
#8705=CARTESIAN_POINT('Ctrl Pts',(-7.93387242656103,20.0000000365693,-6.87929279207206));
#8706=CARTESIAN_POINT('Ctrl Pts',(-7.76761933943708,20.0115427600485,-7.07103209197269));
#8707=CARTESIAN_POINT('Ctrl Pts',(-7.59438520903055,20.0230854835278,-7.25677295860134));
#8708=CARTESIAN_POINT('Ctrl Pts',(-7.41462834869705,20.034628207007,-7.4360128732203));
#8709=CARTESIAN_POINT('Ctrl Pts',(-7.23490292970705,20.0461689115439,-7.61522143691495));
#8710=CARTESIAN_POINT('Ctrl Pts',(-7.04865725581925,20.0577096160809,-7.78793112142728));
#8711=CARTESIAN_POINT('Ctrl Pts',(-6.85638681915036,20.0692503206178,-7.95367592916516));
#8712=CARTESIAN_POINT('Ctrl Pts',(-6.66413668086264,20.080789806779,-8.11940323888648));
#8713=CARTESIAN_POINT('Ctrl Pts',(-6.46586326115029,20.0923292929403,-8.27816695779237));
#8714=CARTESIAN_POINT('Ctrl Pts',(-6.26209628867734,20.1038687791016,-8.42954038316049));
#8715=CARTESIAN_POINT('Ctrl Pts',(-6.05831348529575,20.1154091617798,-8.58092556891764));
#8716=CARTESIAN_POINT('Ctrl Pts',(-5.84903649881054,20.126949544458,-8.72491914519595));
#8717=CARTESIAN_POINT('Ctrl Pts',(-5.63482633728949,20.1384899271363,-8.86113610935916));
#8718=CARTESIAN_POINT('Ctrl Pts',(-5.42061577914819,20.1500303311821,-8.99735332573452));
#8719=CARTESIAN_POINT('Ctrl Pts',(-5.20147226469043,20.1615707352279,-9.12579375361984));
#8720=CARTESIAN_POINT('Ctrl Pts',(-4.97798450545638,20.1731111392737,-9.24611655039218));
#8721=CARTESIAN_POINT('Ctrl Pts',(-4.75444854472634,20.1846540323361,-9.36646529820017));
#8722=CARTESIAN_POINT('Ctrl Pts',(-4.52656671290687,20.1961969253985,-9.47869278418477));
#8723=CARTESIAN_POINT('Ctrl Pts',(-4.29495217795627,20.2077398184608,-9.58250420240288));
#8724=CARTESIAN_POINT('Ctrl Pts',(-4.17906943469033,20.2135150264528,-9.63444374034253));
#8725=CARTESIAN_POINT('Ctrl Pts',(-4.06225265218799,20.2192902344447,-9.6842772535272));
#8726=CARTESIAN_POINT('Ctrl Pts',(-3.94458058590528,20.2250654424367,-9.73197230787774));
#8727=CARTESIAN_POINT('Ctrl Pts',(-3.70889539637858,20.236632597099,-9.8275006544021));
#8728=CARTESIAN_POINT('Ctrl Pts',(-3.46970190359019,20.2481997517614,-9.91447815568018));
#8729=CARTESIAN_POINT('Ctrl Pts',(-3.227639342775,20.2597669064238,-9.99266457322425));
#8730=CARTESIAN_POINT('Ctrl Pts',(-2.98561909575511,20.2713320390874,-10.0708373233757));
#8731=CARTESIAN_POINT('Ctrl Pts',(-2.74073104518588,20.282897171751,-10.1402219724847));
#8732=CARTESIAN_POINT('Ctrl Pts',(-2.49363094408252,20.2944623044145,-10.2006277117986));
#8733=CARTESIAN_POINT('Ctrl Pts',(-2.24655838679567,20.306026147933,-10.2610267177903));
#8734=CARTESIAN_POINT('Ctrl Pts',(-1.99727454010465,20.3175899914514,-10.3124487466889));
#8735=CARTESIAN_POINT('Ctrl Pts',(-1.74644781609206,20.3291538349698,-10.3547535473167));
#8736=CARTESIAN_POINT('Ctrl Pts',(-1.49560122773008,20.3407185942927,-10.3970616982946));
#8737=CARTESIAN_POINT('Ctrl Pts',(-1.24321179031955,20.3522833536156,-10.4302511288727));
#8738=CARTESIAN_POINT('Ctrl Pts',(-0.989956899476713,20.3638481129385,-10.4542329387277));
#8739=CARTESIAN_POINT('Ctrl Pts',(-0.736706570407378,20.3754126639502,-10.4782143166084));
#8740=CARTESIAN_POINT('Ctrl Pts',(-0.482591094877707,20.386977214962,-10.4929883812208));
#8741=CARTESIAN_POINT('Ctrl Pts',(-0.228292540303652,20.3985417659737,-10.4985181581041));
#8742=CARTESIAN_POINT('Ctrl Pts',(0.0260656621990141,20.4101090295511,-10.5040492320444));
#8743=CARTESIAN_POINT('Ctrl Pts',(0.280606752688652,20.4216762931284,-10.5003316777243));
#8744=CARTESIAN_POINT('Ctrl Pts',(0.534647621022751,20.4332435567058,-10.4873806511128));
#8745=CARTESIAN_POINT('Ctrl Pts',(0.754810692836675,20.4432682598111,-10.4761567176542));
#8746=CARTESIAN_POINT('Ctrl Pts',(0.974597946320386,20.4532929629165,-10.4579986016713));
#8747=CARTESIAN_POINT('Ctrl Pts',(1.19356681527101,20.4633176660218,-10.4329477741185));
#8748=CARTESIAN_POINT('Ctrl Pts',(1.44621574302689,20.4748842896372,-10.4040438264891));
#8749=CARTESIAN_POINT('Ctrl Pts',(1.69785355141683,20.4864509132526,-10.3659536780285));
#8750=CARTESIAN_POINT('Ctrl Pts',(1.94780404330222,20.4980175368679,-10.3187722335991));
#8751=CARTESIAN_POINT('Ctrl Pts',(2.19771061531791,20.5095821280624,-10.271599079623));
#8752=CARTESIAN_POINT('Ctrl Pts',(2.44593019076294,20.5211467192569,-10.2153378699943));
#8753=CARTESIAN_POINT('Ctrl Pts',(2.69179571929448,20.5327113104513,-10.1501348171139));
#8754=CARTESIAN_POINT('Ctrl Pts',(2.93763365212993,20.5442746036479,-10.0849390825577));
#8755=CARTESIAN_POINT('Ctrl Pts',(3.18111779808646,20.5558378968444,-10.0108035796106));
#8756=CARTESIAN_POINT('Ctrl Pts',(3.42159418211181,20.567401190041,-9.92792497216506));
#8757=CARTESIAN_POINT('Ctrl Pts',(3.66208940860482,20.5789653892765,-9.84503987078675));
#8758=CARTESIAN_POINT('Ctrl Pts',(3.89957613936932,20.5905295885121,-9.7534103830688));
#8759=CARTESIAN_POINT('Ctrl Pts',(4.13341708260761,20.6020937877476,-9.65328256196863));
#8760=CARTESIAN_POINT('Ctrl Pts',(4.36725372089671,20.6136577740893,-9.55315658419485));
#8761=CARTESIAN_POINT('Ctrl Pts',(4.59744445206855,20.6252217604311,-9.44453269662927));
#8762=CARTESIAN_POINT('Ctrl Pts',(4.82337272867542,20.6367857467728,-9.32770478307875));
#8763=CARTESIAN_POINT('Ctrl Pts',(5.049353932526,20.6483524421598,-9.21084950075641));
#8764=CARTESIAN_POINT('Ctrl Pts',(5.27107043963594,20.6599191375467,-9.08578647774354));
#8765=CARTESIAN_POINT('Ctrl Pts',(5.48792973200312,20.6714858329337,-8.95285587154156));
#8766=CARTESIAN_POINT('Ctrl Pts',(5.67594100123841,20.6815138518248,-8.83760855278735));
#8767=CARTESIAN_POINT('Ctrl Pts',(5.86030167021098,20.6915418707158,-8.71644839631923));
#8768=CARTESIAN_POINT('Ctrl Pts',(6.04064259344008,20.7015698896069,-8.58962386011853));
#8769=CARTESIAN_POINT('Ctrl Pts',(6.24866971656362,20.7131374244913,-8.44332903731897));
#8770=CARTESIAN_POINT('Ctrl Pts',(6.45141193053673,20.7247049593757,-8.2894509307573));
#8771=CARTESIAN_POINT('Ctrl Pts',(6.64832085415769,20.7362724942601,-8.1283965712908));
#8772=CARTESIAN_POINT('Ctrl Pts',(6.84519539190618,20.7478380091254,-7.96737033647484));
#8773=CARTESIAN_POINT('Ctrl Pts',(7.03623845868885,20.7594035239908,-7.79917052559365));
#8774=CARTESIAN_POINT('Ctrl Pts',(7.22093426151812,20.7709690388561,-7.624244840693));
#8775=CARTESIAN_POINT('Ctrl Pts',(7.4056094914013,20.7825332654588,-7.4493386404619));
#8776=CARTESIAN_POINT('Ctrl Pts',(7.58393866813121,20.7940974920614,-7.26770825235433));
#8777=CARTESIAN_POINT('Ctrl Pts',(7.75544162581868,20.805661718664,-7.07983941827206));
#8778=CARTESIAN_POINT('Ctrl Pts',(7.92695814427787,20.8172268596523,-6.89195572936509));
#8779=CARTESIAN_POINT('Ctrl Pts',(8.09164717607218,20.8287920006405,-6.69783281100001));
#8780=CARTESIAN_POINT('Ctrl Pts',(8.24906684102578,20.8403571416288,-6.49799178610508));
#8781=CARTESIAN_POINT('Ctrl Pts',(8.40648365211932,20.8519220729527,-6.29815438412675));
#8782=CARTESIAN_POINT('Ctrl Pts',(8.55663119010718,20.8634870042766,-6.09259930154301));
#8783=CARTESIAN_POINT('Ctrl Pts',(8.69910868029778,20.8750519356005,-5.88187973086563));
#8784=CARTESIAN_POINT('Ctrl Pts',(8.84161952783095,20.8866195745477,-5.67111082576427));
#8785=CARTESIAN_POINT('Ctrl Pts',(8.97645658274871,20.8981872134949,-5.45517524491679));
#8786=CARTESIAN_POINT('Ctrl Pts',(9.10326231471628,20.9097548524421,-5.23465531142849));
#8787=CARTESIAN_POINT('Ctrl Pts',(9.21312918916514,20.9197772726921,-5.04359268775918));
#8788=CARTESIAN_POINT('Ctrl Pts',(9.31696772742072,20.929799692942,-4.84908921829048));
#8789=CARTESIAN_POINT('Ctrl Pts',(9.41457305225478,20.939822113192,-4.65153901883646));
#8790=CARTESIAN_POINT('Ctrl Pts',(9.52721930290881,20.9513889827819,-4.42354644443252));
#8791=CARTESIAN_POINT('Ctrl Pts',(9.63159720442441,20.9629558523718,-4.19142462929393));
#8792=CARTESIAN_POINT('Ctrl Pts',(9.7274200224257,20.9745227219618,-3.9557933094781));
#8793=CARTESIAN_POINT('Ctrl Pts',(9.82322603763168,20.9860875632692,-3.72020330826378));
#8794=CARTESIAN_POINT('Ctrl Pts',(9.91047985981083,20.9976524045767,-3.48110528720773));
#8795=CARTESIAN_POINT('Ctrl Pts',(9.98894283068399,21.0092172458841,-3.23913910249729));
#8796=CARTESIAN_POINT('Ctrl Pts',(10.0673970183146,21.0207807926089,-2.99720000378267));
#8797=CARTESIAN_POINT('Ctrl Pts',(10.1370622341291,21.0323443393336,-2.75239364572893));
#8798=CARTESIAN_POINT('Ctrl Pts',(10.1977493055541,21.0439078860583,-2.50537623942409));
#8799=CARTESIAN_POINT('Ctrl Pts',(10.2584411501937,21.0554723422896,-2.25833940448208));
#8800=CARTESIAN_POINT('Ctrl Pts',(10.3101533700907,21.0670367985209,-2.00909144186784));
#8801=CARTESIAN_POINT('Ctrl Pts',(10.3527473408365,21.0786012547522,-1.75830131001571));
#8802=CARTESIAN_POINT('Ctrl Pts',(10.3953405331328,21.0901654996309,-1.50751576161625));
#8803=CARTESIAN_POINT('Ctrl Pts',(10.428815765027,21.1017297445096,-1.25518837362866));
#8804=CARTESIAN_POINT('Ctrl Pts',(10.453085851784,21.1132939893884,-1.00199659442159));
#8805=CARTESIAN_POINT('Ctrl Pts',(10.4773616255209,21.1248609440072,-0.748745487179122));
#8806=CARTESIAN_POINT('Ctrl Pts',(10.492427915911,21.1364278986261,-0.494629859558551));
#8807=CARTESIAN_POINT('Ctrl Pts',(10.4982494496924,21.147994853245,-0.240332045374405));
#8808=CARTESIAN_POINT('Ctrl Pts',(10.5032956851473,21.1580213477557,-0.0199010225155619));
#8809=CARTESIAN_POINT('Ctrl Pts',(10.5013963984425,21.1680478422664,0.200666716014741));
#8810=CARTESIAN_POINT('Ctrl Pts',(10.4925603111451,21.1780743367771,0.420926498313265));
#8811=CARTESIAN_POINT('Ctrl Pts',(10.4823664180197,21.1896415621819,0.675032711280474));
#8812=CARTESIAN_POINT('Ctrl Pts',(10.4629357848001,21.2012087875866,0.928807784217113));
#8813=CARTESIAN_POINT('Ctrl Pts',(10.4343132327989,21.2127760129914,1.18157029407343));
#8814=CARTESIAN_POINT('Ctrl Pts',(10.405695689421,21.2243412142624,1.4342885733465));
#8815=CARTESIAN_POINT('Ctrl Pts',(10.3678894693691,21.2359064155334,1.6859943683356));
#8816=CARTESIAN_POINT('Ctrl Pts',(10.3209912360567,21.2474716168044,1.9360115973934));
#8817=CARTESIAN_POINT('Ctrl Pts',(10.2740982398118,21.2590355266038,2.18600090733733));
#8818=CARTESIAN_POINT('Ctrl Pts',(10.2181153085458,21.2705994364031,2.43430175588062));
#8819=CARTESIAN_POINT('Ctrl Pts',(10.1531903835915,21.2821633462024,2.68024738308711));
#8820=CARTESIAN_POINT('Ctrl Pts',(10.0882603399369,21.2937281677038,2.92621240071936));
#8821=CARTESIAN_POINT('Ctrl Pts',(10.0143869613077,21.3052929892052,3.16982155745538));
#8822=CARTESIAN_POINT('Ctrl Pts',(9.93176867348247,21.3168578107066,3.4104210907793));
#8823=CARTESIAN_POINT('Ctrl Pts',(9.84915189072215,21.3284224215306,3.65101624107944));
#8824=CARTESIAN_POINT('Ctrl Pts',(9.75779060903818,21.3399870323546,3.88860161638269));
#8825=CARTESIAN_POINT('Ctrl Pts',(9.65793248410276,21.3515516431785,4.12254061623566));
#8826=CARTESIAN_POINT('Ctrl Pts',(9.55805097403558,21.3631189622443,4.35653440075777));
#8827=CARTESIAN_POINT('Ctrl Pts',(9.44966875177061,21.3746862813101,4.58687984810717));
#8828=CARTESIAN_POINT('Ctrl Pts',(9.33308139224463,21.3862536003759,4.81296091047258));
#8829=CARTESIAN_POINT('Ctrl Pts',(9.23204596712439,21.3962779203713,5.00888434797557));
#8830=CARTESIAN_POINT('Ctrl Pts',(9.12484921800875,21.4063022403668,5.20160543394834));
#8831=CARTESIAN_POINT('Ctrl Pts',(9.01171144400528,21.4163265603622,5.3907381544631));
#8832=CARTESIAN_POINT('Ctrl Pts',(8.88116158188506,21.4278936395697,5.60897870942459));
#8833=CARTESIAN_POINT('Ctrl Pts',(8.74265991882837,21.4394607187771,5.82250848322717));
#8834=CARTESIAN_POINT('Ctrl Pts',(8.59657188523117,21.4510277979846,6.0307506018781));
#8835=CARTESIAN_POINT('Ctrl Pts',(8.45050943566692,21.4625928514783,6.23895625160618));
#8836=CARTESIAN_POINT('Ctrl Pts',(8.29686342668251,21.474157904972,6.44187586825196));
#8837=CARTESIAN_POINT('Ctrl Pts',(8.1360422536485,21.4857229584658,6.63896207602109));
#8838=CARTESIAN_POINT('Ctrl Pts',(7.97523905559414,21.4972867193337,6.83602625546828));
#8839=CARTESIAN_POINT('Ctrl Pts',(7.80726246971827,21.5088504802016,7.02725811347687));
#8840=CARTESIAN_POINT('Ctrl Pts',(7.63256145618762,21.5204142410695,7.21214299757839));
#8841=CARTESIAN_POINT('Ctrl Pts',(7.45784667973596,21.5319789129288,7.39704244688481));
#8842=CARTESIAN_POINT('Ctrl Pts',(7.27640660479359,21.5435435847882,7.57559371963131));
#8843=CARTESIAN_POINT('Ctrl Pts',(7.08872830055373,21.5551082566475,7.74731773460523));
#8844=CARTESIAN_POINT('Ctrl Pts',(6.90105341809982,21.5666727176576,7.91903861867477));
#8845=CARTESIAN_POINT('Ctrl Pts',(6.70714073932691,21.5782371786677,8.08393230839132));
#8846=CARTESIAN_POINT('Ctrl Pts',(6.50751234785372,21.5898016396778,8.24155835036866));
#8847=CARTESIAN_POINT('Ctrl Pts',(6.30783719252306,21.6013688097154,8.39922131696232));
#8848=CARTESIAN_POINT('Ctrl Pts',(6.10244386533014,21.612935979753,8.54961306089783));
#8849=CARTESIAN_POINT('Ctrl Pts',(5.89188669093872,21.6245031497906,8.69233410662172));
#8850=CARTESIAN_POINT('Ctrl Pts',(5.70939778698386,21.6345283611761,8.8160297597417));
#8851=CARTESIAN_POINT('Ctrl Pts',(5.52303059208186,21.6445535725617,8.93396407346112));
#8852=CARTESIAN_POINT('Ctrl Pts',(5.3331633740482,21.6545787839473,9.04590346099885));
#8853=CARTESIAN_POINT('Ctrl Pts',(5.11409401130845,21.6661459027596,9.17505946037215));
#8854=CARTESIAN_POINT('Ctrl Pts',(4.89029674129765,21.677713021572,9.29627375453589));
#8855=CARTESIAN_POINT('Ctrl Pts',(4.66236849914987,21.6892801403843,9.40921468445348));
#8856=CARTESIAN_POINT('Ctrl Pts',(4.4344801664234,21.7008452338355,9.52213583881753));
#8857=CARTESIAN_POINT('Ctrl Pts',(4.20246255342235,21.7124103272867,9.62678639796797));
#8858=CARTESIAN_POINT('Ctrl Pts',(3.96693620500328,21.7239754207378,9.72288116483145));
#8859=CARTESIAN_POINT('Ctrl Pts',(3.73143617643087,21.7355392218007,9.81896519319563));
#8860=CARTESIAN_POINT('Ctrl Pts',(3.49242845155076,21.7471030228636,9.90649523377258));
#8861=CARTESIAN_POINT('Ctrl Pts',(3.25055353409967,21.7586668239265,9.98523423470637));
#8862=CARTESIAN_POINT('Ctrl Pts',(3.00865956023713,21.7702315360576,10.0639794391887));
#8863=CARTESIAN_POINT('Ctrl Pts',(2.76389820463271,21.7817962481888,10.1339321311693));
#8864=CARTESIAN_POINT('Ctrl Pts',(2.51692641074983,21.7933609603199,10.1949047294651));
#8865=CARTESIAN_POINT('Ctrl Pts',(2.26995912005407,21.8049254615846,10.2558762160104));
#8866=CARTESIAN_POINT('Ctrl Pts',(2.02078174091657,21.8164899628492,10.3078678717852));
#8867=CARTESIAN_POINT('Ctrl Pts',(1.77006347660718,21.8280544641139,10.3507427892293));
#8868=CARTESIAN_POINT('Ctrl Pts',(1.51928648744899,21.8396216740907,10.3936277491129));
#8869=CARTESIAN_POINT('Ctrl Pts',(1.26696816464985,21.8511888840674,10.4273916553262));
#8870=CARTESIAN_POINT('Ctrl Pts',(1.01378641150786,21.8627560940442,10.451949010201));
#8871=CARTESIAN_POINT('Ctrl Pts',(0.794361003023756,21.8727810652069,10.4732321696619));
#8872=CARTESIAN_POINT('Ctrl Pts',(0.574287290355624,21.8828060363696,10.4876009062648));
#8873=CARTESIAN_POINT('Ctrl Pts',(0.354009164658848,21.8928310075323,10.4950311343672));
#8874=CARTESIAN_POINT('Ctrl Pts',(0.0998454799983954,21.9043981279682,10.5036043603578));
#8875=CARTESIAN_POINT('Ctrl Pts',(-0.154669164764553,21.9159652484041,10.5029417501122));
#8876=CARTESIAN_POINT('Ctrl Pts',(-0.408851908986821,21.92753236884,10.4930377449296));
#8877=CARTESIAN_POINT('Ctrl Pts',(-0.662990148560078,21.9390974639982,10.4831354738312));
#8878=CARTESIAN_POINT('Ctrl Pts',(-0.916796327124914,21.9506625591565,10.4639950486802));
#8879=CARTESIAN_POINT('Ctrl Pts',(-1.16958908724468,21.9622276543147,10.4356630056263));
#8880=CARTESIAN_POINT('Ctrl Pts',(-1.42235359973181,21.9737914571631,10.4073341284589));
#8881=CARTESIAN_POINT('Ctrl Pts',(-1.67410464488521,21.9853552600116,10.3698157149898));
#8882=CARTESIAN_POINT('Ctrl Pts',(-1.9241663796562,21.99691906286,10.323206127139));
#8883=CARTESIAN_POINT('Ctrl Pts',(-2.17424781820299,22.0084837768858,10.2765928666557));
#8884=CARTESIAN_POINT('Ctrl Pts',(-2.42263940761389,22.0200484909115,10.220887047828));
#8885=CARTESIAN_POINT('Ctrl Pts',(-2.66867454355026,22.0316132049373,10.1562383381155));
#8886=CARTESIAN_POINT('Ctrl Pts',(-2.91470519460546,22.0431777081542,10.0915908068597));
#8887=CARTESIAN_POINT('Ctrl Pts',(-3.15837921079943,22.0547422113712,10.0180007828975));
#8888=CARTESIAN_POINT('Ctrl Pts',(-3.39904347241097,22.0663067145882,9.93566829522103));
#8889=CARTESIAN_POINT('Ctrl Pts',(-3.6397641056346,22.0778739265982,9.85331652252478));
#8890=CARTESIAN_POINT('Ctrl Pts',(-3.87747331294342,22.0894411386083,9.76221828223451));
#8891=CARTESIAN_POINT('Ctrl Pts',(-4.11153493727735,22.1010083506183,9.66262290786243));
#8892=CARTESIAN_POINT('Ctrl Pts',(-4.31438921697679,22.1110333107847,9.57630654572003));
#8893=CARTESIAN_POINT('Ctrl Pts',(-4.51450390802682,22.1210582709511,9.48360864941968));
#8894=CARTESIAN_POINT('Ctrl Pts',(-4.71147772092378,22.1310832311175,9.38472049052282));
#8895=CARTESIAN_POINT('Ctrl Pts',(-4.93875220021531,22.1426503403095,9.27062027338817));
#8896=CARTESIAN_POINT('Ctrl Pts',(-5.16191511449861,22.1542174495014,9.14824246401068));
#8897=CARTESIAN_POINT('Ctrl Pts',(-5.38036420898964,22.1657845586934,9.01790895821328));
#8898=CARTESIAN_POINT('Ctrl Pts',(-5.59877505233851,22.1773496424472,8.88759827423379));
#8899=CARTESIAN_POINT('Ctrl Pts',(-5.81247348602248,22.1889147262009,8.74933481654849));
#8900=CARTESIAN_POINT('Ctrl Pts',(-6.02088350472526,22.2004798099547,8.60348550428995));
#8901=CARTESIAN_POINT('Ctrl Pts',(-6.22927023290093,22.2120436012711,8.45765249118719));
#8902=CARTESIAN_POINT('Ctrl Pts',(-6.43236949941675,22.2236073925875,8.30423547485258));
#8903=CARTESIAN_POINT('Ctrl Pts',(-6.62963494174465,22.2351711839039,8.14364424193484));
#8904=CARTESIAN_POINT('Ctrl Pts',(-6.82691592579408,22.2467358862832,7.98304035670358));
#8905=CARTESIAN_POINT('Ctrl Pts',(-7.01836195042591,22.2583005886625,7.81526129764087));
#8906=CARTESIAN_POINT('Ctrl Pts',(-7.20345931715591,22.2698652910418,7.64075747986283));
#8907=CARTESIAN_POINT('Ctrl Pts',(-7.38855330907376,22.2814297825661,7.46625684374865));
#8908=CARTESIAN_POINT('Ctrl Pts',(-7.56729867441535,22.2929942740905,7.28503188540077));
#8909=CARTESIAN_POINT('Ctrl Pts',(-7.73921765517788,22.3045587656148,7.09757078765566));
#8910=CARTESIAN_POINT('Ctrl Pts',(-7.91117690526097,22.3161259659396,6.91006578009324));
#8911=CARTESIAN_POINT('Ctrl Pts',(-8.07630638719474,22.3276931662644,6.71632191726792));
#8912=CARTESIAN_POINT('Ctrl Pts',(-8.23416683158492,22.3392603665892,6.51686255721469));
#8913=CARTESIAN_POINT('Ctrl Pts',(-8.37098088745965,22.3492853959603,6.34399566749777));
#8914=CARTESIAN_POINT('Ctrl Pts',(-8.50233549758968,22.3593104253315,6.16683632915167));
#8915=CARTESIAN_POINT('Ctrl Pts',(-8.6279698299386,22.3693354547026,5.98574453294403));
#8916=CARTESIAN_POINT('Ctrl Pts',(-8.7729297269788,22.3809025733261,5.776796487913));
#8917=CARTESIAN_POINT('Ctrl Pts',(-8.91031820995912,22.3924696919496,5.56254773761589));
#8918=CARTESIAN_POINT('Ctrl Pts',(-9.03976050121706,22.4040368105731,5.343569133139));
#8919=CARTESIAN_POINT('Ctrl Pts',(-9.16918012806939,22.4156019038781,5.12462887022624));
#8920=CARTESIAN_POINT('Ctrl Pts',(-9.29065619986459,22.4271669971831,4.9009606445605));
#8921=CARTESIAN_POINT('Ctrl Pts',(-9.40385853326217,22.4387320904881,4.67316227905604));
#8922=CARTESIAN_POINT('Ctrl Pts',(-9.51704821682695,22.4502958914479,4.44538936895653));
#8923=CARTESIAN_POINT('Ctrl Pts',(-9.62196588488816,22.4618596924076,4.2134874883438));
#8924=CARTESIAN_POINT('Ctrl Pts',(-9.71832789633379,22.4734234933674,3.97807791519226));
#8925=CARTESIAN_POINT('Ctrl Pts',(-9.81469750034251,22.484988205463,3.74264979363137));
#8926=CARTESIAN_POINT('Ctrl Pts',(-9.90250999273814,22.4965529175587,3.50371368221689));
#8927=CARTESIAN_POINT('Ctrl Pts',(-9.98152985600637,22.5081176296544,3.26191090216357));
#8928=CARTESIAN_POINT('Ctrl Pts',(-10.060548278714,22.5196821309211,3.02011253026216));
#8929=CARTESIAN_POINT('Ctrl Pts',(-10.1307743086362,22.5312466321879,2.77544785797645));
#8930=CARTESIAN_POINT('Ctrl Pts',(-10.1920220597857,22.5428111334547,2.52857416993089));
#8931=CARTESIAN_POINT('Ctrl Pts',(-10.253284157106,22.5543783434954,2.28164265621764));
#8932=CARTESIAN_POINT('Ctrl Pts',(-10.3055637050415,22.5659455535361,2.03250136123242));
#8933=CARTESIAN_POINT('Ctrl Pts',(-10.3487254459157,22.5775127635768,1.78182003722534));
#8934=CARTESIAN_POINT('Ctrl Pts',(-10.3861324977168,22.5875377351471,1.56456167176555));
#8935=CARTESIAN_POINT('Ctrl Pts',(-10.4166917642207,22.5975627067174,1.34614685374224));
#8936=CARTESIAN_POINT('Ctrl Pts',(-10.4403464900633,22.6075876782877,1.12701648941934));
#8937=CARTESIAN_POINT('Ctrl Pts',(-10.4692474892472,22.6198360424031,0.859286204883308));
#8938=CARTESIAN_POINT('Ctrl Pts',(-10.4878466242685,22.6320844065186,0.590435506072792));
#8939=CARTESIAN_POINT('Ctrl Pts',(-10.496085593371,22.644332770634,0.32122922754471));
#8940=CARTESIAN_POINT('Ctrl Pts',(-10.4993586516315,22.6491986232481,0.214282858074387));
#8941=CARTESIAN_POINT('Ctrl Pts',(-10.5009972449014,22.6540644758621,0.107280420198263));
#8942=CARTESIAN_POINT('Ctrl Pts',(-10.5009999965284,22.6589303284762,0.000270018945713879));
#8943=CARTESIAN_POINT('',(7.93381306740072,20.,-6.87936125025729));
#8944=CARTESIAN_POINT('Origin',(0.,20.,0.));
#8945=CARTESIAN_POINT('Ctrl Pts',(7.93381306740072,20.,-6.87936125025729));
#8946=CARTESIAN_POINT('Ctrl Pts',(8.33170850771912,20.0276160927694,-6.42047736132949));
#8947=CARTESIAN_POINT('Ctrl Pts',(8.6890477220574,20.054661105705,-5.9279313429));
#8948=CARTESIAN_POINT('Ctrl Pts',(9.25327381718263,20.1041280035438,-4.98862816615476));
#8949=CARTESIAN_POINT('Ctrl Pts',(9.47522497451872,20.126344404341,-4.55297499331653));
#8950=CARTESIAN_POINT('Ctrl Pts',(9.79836691632613,20.1643589694833,-3.79178851112153));
#8951=CARTESIAN_POINT('Ctrl Pts',(9.91553003773292,20.1800057244298,-3.47389058038225));
#8952=CARTESIAN_POINT('Ctrl Pts',(10.0952999382063,20.2076664306373,-2.90237669961849));
#8953=CARTESIAN_POINT('Ctrl Pts',(10.1641960235044,20.219674611679,-2.65103624009131));
#8954=CARTESIAN_POINT('Ctrl Pts',(10.3094356532406,20.2487563952025,-2.03166213315775));
#8955=CARTESIAN_POINT('Ctrl Pts',(10.3755099682223,20.2656411687531,-1.66159912157421));
#8956=CARTESIAN_POINT('Ctrl Pts',(10.4777552458961,20.303032596406,-0.834802718256054));
#8957=CARTESIAN_POINT('Ctrl Pts',(10.5041720493136,20.3235132528092,-0.377643834044697));
#8958=CARTESIAN_POINT('Ctrl Pts',(10.496453767424,20.3695127093978,0.638301907748669));
#8959=CARTESIAN_POINT('Ctrl Pts',(10.4476558813244,20.395092943157,1.1955885646722));
#8960=CARTESIAN_POINT('Ctrl Pts',(10.3016966979839,20.4355285424765,2.06104547614693));
#8961=CARTESIAN_POINT('Ctrl Pts',(10.2342996985265,20.4502475425874,2.37317831113298));
#8962=CARTESIAN_POINT('Ctrl Pts',(10.0570313419514,20.4820093583924,3.04429371137263));
#8963=CARTESIAN_POINT('Ctrl Pts',(9.94192385891823,20.4989006904602,3.40143468374545));
#8964=CARTESIAN_POINT('Ctrl Pts',(9.63986791337795,20.5368593837045,4.1910983082916));
#8965=CARTESIAN_POINT('Ctrl Pts',(9.44243741772192,20.5579055054931,4.61873680006114));
#8966=CARTESIAN_POINT('Ctrl Pts',(8.91191104245967,20.6079994043206,5.5905496196773));
#8967=CARTESIAN_POINT('Ctrl Pts',(8.55663196483671,20.6371917674026,6.12049147995457));
#8968=CARTESIAN_POINT('Ctrl Pts',(7.97378386342717,20.6798218120091,6.83908192755249));
#8969=CARTESIAN_POINT('Ctrl Pts',(7.78284407418771,20.6931119818567,7.05560850752202));
#8970=CARTESIAN_POINT('Ctrl Pts',(7.32890788282693,20.7230916506436,7.52949384767635));
#8971=CARTESIAN_POINT('Ctrl Pts',(7.0608247281153,20.7396254506821,7.78144756106601));
#8972=CARTESIAN_POINT('Ctrl Pts',(6.42926161537202,20.7767429292833,8.31544629874953));
#8973=CARTESIAN_POINT('Ctrl Pts',(6.0593663925618,20.7973022681417,8.58872086019017));
#8974=CARTESIAN_POINT('Ctrl Pts',(5.12991785590839,20.8472877075065,9.18537263375261));
#8975=CARTESIAN_POINT('Ctrl Pts',(4.55612010371929,20.876887788323,9.48308275207275));
#8976=CARTESIAN_POINT('Ctrl Pts',(3.69901264028119,20.9195379465733,9.8319322831093));
#8977=CARTESIAN_POINT('Ctrl Pts',(3.43523340515425,20.9324494287245,9.9271728580165));
#8978=CARTESIAN_POINT('Ctrl Pts',(2.83021902392823,20.9614404354452,10.1186140352906));
#8979=CARTESIAN_POINT('Ctrl Pts',(2.48729389099104,20.9773789866624,10.2083231847577));
#8980=CARTESIAN_POINT('Ctrl Pts',(1.68420993801496,21.0142008888276,10.3755311924679));
#8981=CARTESIAN_POINT('Ctrl Pts',(1.22212278455807,21.0350511105719,10.4400489434024));
#8982=CARTESIAN_POINT('Ctrl Pts',(0.125954152230296,21.0847779393699,10.5193059252721));
#8983=CARTESIAN_POINT('Ctrl Pts',(-0.508197190164823,21.1138006461458,10.5077762010507));
#8984=CARTESIAN_POINT('Ctrl Pts',(-1.42441616088062,21.1562675912602,10.4079480717021));
#8985=CARTESIAN_POINT('Ctrl Pts',(-1.71000102798903,21.1695651291613,10.3648561741657));
#8986=CARTESIAN_POINT('Ctrl Pts',(-2.34296255588236,21.1990213357113,10.2424730595806));
#8987=CARTESIAN_POINT('Ctrl Pts',(-2.68880852581115,21.2150413230804,10.157166930549));
#8988=CARTESIAN_POINT('Ctrl Pts',(-3.47516177481196,21.2519075549319,9.92021883200492));
#8989=CARTESIAN_POINT('Ctrl Pts',(-3.91124289030554,21.2727226706814,9.75651913122846));
#8990=CARTESIAN_POINT('Ctrl Pts',(-4.92738186256186,21.3231991359801,9.29596026407012));
#8991=CARTESIAN_POINT('Ctrl Pts',(-5.49350364275742,21.353033187985,8.97303445559977));
#8992=CARTESIAN_POINT('Ctrl Pts',(-6.25637932893135,21.3959611522619,8.4384707840874));
#8993=CARTESIAN_POINT('Ctrl Pts',(-6.48009235505487,21.4089110064311,8.26791854861376));
#8994=CARTESIAN_POINT('Ctrl Pts',(-6.98250597371194,21.4387064996792,7.85196125438404));
#8995=CARTESIAN_POINT('Ctrl Pts',(-7.25557334748587,21.455387295951,7.60035159506074));
#8996=CARTESIAN_POINT('Ctrl Pts',(-7.83567546319084,21.4926580291033,7.00601774921797));
#8997=CARTESIAN_POINT('Ctrl Pts',(-8.13466751077909,21.5132236303013,6.65652115756698));
#8998=CARTESIAN_POINT('Ctrl Pts',(-8.75160441519402,21.5598569737943,5.8314816379862));
#8999=CARTESIAN_POINT('Ctrl Pts',(-9.05555988987851,21.5859980332283,5.34729517612323));
#9000=CARTESIAN_POINT('Ctrl Pts',(-9.4650561751063,21.6269275040984,4.55900940410054));
#9001=CARTESIAN_POINT('Ctrl Pts',(-9.5985956070701,21.6415732678217,4.27069313825337));
#9002=CARTESIAN_POINT('Ctrl Pts',(-9.86078218491834,21.6732509339197,3.62993266846404));
#9003=CARTESIAN_POINT('Ctrl Pts',(-9.9840306246657,21.6901303635167,3.27575537037389));
#9004=CARTESIAN_POINT('Ctrl Pts',(-10.2178516872492,21.7279344349071,2.46676406607352));
#9005=CARTESIAN_POINT('Ctrl Pts',(-10.3174994780433,21.7488388005139,2.00963136933526));
#9006=CARTESIAN_POINT('Ctrl Pts',(-10.4824452607786,21.7994776004841,0.902482616465333));
#9007=CARTESIAN_POINT('Ctrl Pts',(-10.5182494478197,21.8293840331909,0.250044238442422));
#9008=CARTESIAN_POINT('Ctrl Pts',(-10.4825538342925,21.8724086802026,-0.682940267238052));
#9009=CARTESIAN_POINT('Ctrl Pts',(-10.4604640690836,21.8853803065603,-0.963865308085334));
#9010=CARTESIAN_POINT('Ctrl Pts',(-10.3823265404302,21.9155202319846,-1.619037524658));
#9011=CARTESIAN_POINT('Ctrl Pts',(-10.3172996736249,21.9325133938148,-1.99181280326991));
#9012=CARTESIAN_POINT('Ctrl Pts',(-10.1296190864295,21.9699826338174,-2.80544831621959));
#9013=CARTESIAN_POINT('Ctrl Pts',(-9.99799076945949,21.9904370961928,-3.24343916582445));
#9014=CARTESIAN_POINT('Ctrl Pts',(-9.83826089695888,22.011121265682,-3.67146067980712));
#9015=CARTESIAN_POINT('Origin',(0.,20.,0.));
#9016=CARTESIAN_POINT('',(-9.83826089696967,25.8299813406324,-3.67146067977821));
#9017=CARTESIAN_POINT('',(-9.83826089299223,25.0121157186286,-3.67146069043641));
#9018=CARTESIAN_POINT('',(-9.83826089695937,20.,-3.67146067980583));
#9019=CARTESIAN_POINT('',(-10.5012121264633,25.6589303284762,-0.000261163433911081));
#9020=CARTESIAN_POINT('Ctrl Pts',(-9.83826089696967,25.8299813406324,-3.67146067977821));
#9021=CARTESIAN_POINT('Ctrl Pts',(-9.89045159809829,25.8232071459156,-3.53160742275631));
#9022=CARTESIAN_POINT('Ctrl Pts',(-9.939673531474,25.8164106538706,-3.3906056865579));
#9023=CARTESIAN_POINT('Ctrl Pts',(-10.1287223228633,25.7885121074398,-2.80947855419518));
#9024=CARTESIAN_POINT('Ctrl Pts',(-10.2424427334057,25.767240589704,-2.3614703355705));
#9025=CARTESIAN_POINT('Ctrl Pts',(-10.3824353262031,25.7317358521643,-1.6035935839193));
#9026=CARTESIAN_POINT('Ctrl Pts',(-10.4251238890136,25.717526202749,-1.29741018819776));
#9027=CARTESIAN_POINT('Ctrl Pts',(-10.4853901420833,25.6884582855822,-0.66087079578811));
#9028=CARTESIAN_POINT('Ctrl Pts',(-10.500991607173,25.6736315998779,-0.330663241303831));
#9029=CARTESIAN_POINT('Ctrl Pts',(-10.5009999966147,25.6588081038301,-0.000266641749689656));
#9030=CARTESIAN_POINT('Ctrl Pts',(-9.8390004731412,22.8294636018363,-3.6717362226746));
#9031=CARTESIAN_POINT('Ctrl Pts',(-9.79710281651912,22.8349223685151,-3.78421385875093));
#9032=CARTESIAN_POINT('Ctrl Pts',(-9.11528360003952,22.9197985430557,-5.52171118454613));
#9033=CARTESIAN_POINT('Ctrl Pts',(-6.8861881181333,23.0840921254579,-8.50962861104461));
#9034=CARTESIAN_POINT('Ctrl Pts',(-1.97429514280339,23.322344349043,-10.7673360139992));
#9035=CARTESIAN_POINT('Ctrl Pts',(3.41907203483483,23.5605965726281,-10.3991976830994));
#9036=CARTESIAN_POINT('Ctrl Pts',(7.9786251950841,23.7988487962132,-7.49499206591381));
#9037=CARTESIAN_POINT('Ctrl Pts',(10.5924195565847,24.0371010197983,-2.76297195119323));
#9038=CARTESIAN_POINT('Ctrl Pts',(10.6230253270481,24.2753532433834,2.64285810476577));
#9039=CARTESIAN_POINT('Ctrl Pts',(8.06297863443841,24.5136054669685,7.40417055498215));
#9040=CARTESIAN_POINT('Ctrl Pts',(3.53660174667682,24.7518576905536,10.3598172835396));
#9041=CARTESIAN_POINT('Ctrl Pts',(-1.852251294932,24.9901099141387,10.7890004729458));
#9042=CARTESIAN_POINT('Ctrl Pts',(-6.78939314957438,25.2283621377238,8.58705460123571));
#9043=CARTESIAN_POINT('Ctrl Pts',(-9.85990547775721,25.4513022758363,4.5670737028351));
#9044=CARTESIAN_POINT('Ctrl Pts',(-10.4997645278665,25.5948250060871,1.40951361517464));
#9045=CARTESIAN_POINT('Ctrl Pts',(-10.5012121264633,25.6589303284762,-0.000261163433911081));
#9046=CARTESIAN_POINT('Ctrl Pts',(-9.83826089695889,22.011121265682,-3.67146067980712));
#9047=CARTESIAN_POINT('Ctrl Pts',(-9.83815902016989,22.0111344581847,-3.6717336748129));
#9048=CARTESIAN_POINT('Ctrl Pts',(-9.83805713194903,22.0111476507706,-3.67200666576359));
#9049=CARTESIAN_POINT('Ctrl Pts',(-9.64434668302772,22.0362268124193,-4.19095263523416));
#9050=CARTESIAN_POINT('Ctrl Pts',(-9.41002738239786,22.0615788385252,-4.69349193767824));
#9051=CARTESIAN_POINT('Ctrl Pts',(-8.97712264262286,22.102049618576,-5.45781687901402));
#9052=CARTESIAN_POINT('Ctrl Pts',(-8.80402489973173,22.1170322616488,-5.73285651885139));
#9053=CARTESIAN_POINT('Ctrl Pts',(-8.41440599084763,22.1482450050358,-6.29256191692831));
#9054=CARTESIAN_POINT('Ctrl Pts',(-8.19553555048529,22.1643533526806,-6.57508668780649));
#9055=CARTESIAN_POINT('Ctrl Pts',(-7.65258308910481,22.2017570499126,-7.20661073322297));
#9056=CARTESIAN_POINT('Ctrl Pts',(-7.31832987445934,22.2230196512501,-7.54581411621333));
#9057=CARTESIAN_POINT('Ctrl Pts',(-6.46898209784905,22.2743175656941,-8.29803651587865));
#9058=CARTESIAN_POINT('Ctrl Pts',(-5.9357161480937,22.3045223522079,-8.68748361885374));
#9059=CARTESIAN_POINT('Ctrl Pts',(-5.12394153632778,22.3480516497147,-9.17048920874733));
#9060=CARTESIAN_POINT('Ctrl Pts',(-4.8725168794026,22.3612130171386,-9.3065155146438));
#9061=CARTESIAN_POINT('Ctrl Pts',(-4.29763489393,22.3904554879768,-9.5878491972953));
#9062=CARTESIAN_POINT('Ctrl Pts',(-3.97174141558032,22.4063986100488,-9.72737330635653));
#9063=CARTESIAN_POINT('Ctrl Pts',(-3.20245155002429,22.4432131272224,-10.0116084584261));
#9064=CARTESIAN_POINT('Ctrl Pts',(-2.75523686219245,22.4640520645159,-10.143799346496));
#9065=CARTESIAN_POINT('Ctrl Pts',(-1.66473884588458,22.5146184762881,-10.3886728584124));
#9066=CARTESIAN_POINT('Ctrl Pts',(-1.01684588705719,22.5445200078446,-10.4719560635979));
#9067=CARTESIAN_POINT('Ctrl Pts',(-0.0853416228904833,22.5874704913377,
-10.5043929161344));
#9068=CARTESIAN_POINT('Ctrl Pts',(0.195041786972363,22.6003765838329,-10.502928877526));
#9069=CARTESIAN_POINT('Ctrl Pts',(0.81655748248041,22.6287938592871,-10.4747846598895));
#9070=CARTESIAN_POINT('Ctrl Pts',(1.15711873060623,22.6441823048351,-10.4426509660506));
#9071=CARTESIAN_POINT('Ctrl Pts',(1.95922851258783,22.6805636350815,-10.3272410399013));
#9072=CARTESIAN_POINT('Ctrl Pts',(2.41795474048663,22.701516826454,-10.2295637506253));
#9073=CARTESIAN_POINT('Ctrl Pts',(3.49635554825474,22.7522269050209,-9.92332238117599));
#9074=CARTESIAN_POINT('Ctrl Pts',(4.10609480486743,22.7821548408593,-9.68693834709733));
#9075=CARTESIAN_POINT('Ctrl Pts',(4.94269625392056,22.8252426909853,-9.26933483375999));
#9076=CARTESIAN_POINT('Ctrl Pts',(5.19027498506561,22.8382533542126,-9.13300950794298));
#9077=CARTESIAN_POINT('Ctrl Pts',(5.75040850746558,22.8681520763889,-8.79444022394108));
#9078=CARTESIAN_POINT('Ctrl Pts',(6.05830627436546,22.88487469136,-8.5852376614528));
#9079=CARTESIAN_POINT('Ctrl Pts',(6.72007094510577,22.9221775871373,-8.08223637358721));
#9080=CARTESIAN_POINT('Ctrl Pts',(7.06705417455174,22.9427340794435,-7.78065796364311));
#9081=CARTESIAN_POINT('Ctrl Pts',(7.79751885398652,22.9892960837487,-7.05647798906836));
#9082=CARTESIAN_POINT('Ctrl Pts',(8.16857886507436,23.0153735169989,-6.62340351151992));
#9083=CARTESIAN_POINT('Ctrl Pts',(8.68951133169902,23.0562752807112,-5.9046370081607));
#9084=CARTESIAN_POINT('Ctrl Pts',(8.86451243462568,23.0709572450441,-5.63850751838844));
#9085=CARTESIAN_POINT('Ctrl Pts',(9.33304683409507,23.1129214453884,-4.85012744194704));
#9086=CARTESIAN_POINT('Ctrl Pts',(9.59435339042549,23.1396021008703,-4.31020770155439));
#9087=CARTESIAN_POINT('Ctrl Pts',(9.99983374349218,23.1905863083567,-3.24993259678776));
#9088=CARTESIAN_POINT('Ctrl Pts',(10.1527641376387,23.2148085179695,-2.73497656755786));
#9089=CARTESIAN_POINT('Ctrl Pts',(10.4007629878409,23.2687159474576,-1.58331140976642));
#9090=CARTESIAN_POINT('Ctrl Pts',(10.4780616286908,23.2984558210026,-0.944963989157477));
#9091=CARTESIAN_POINT('Ctrl Pts',(10.5075671360965,23.3450782235732,0.0752577520063168));
#9092=CARTESIAN_POINT('Ctrl Pts',(10.4980074689732,23.3621089064779,0.454394046262921));
#9093=CARTESIAN_POINT('Ctrl Pts',(10.4317614492728,23.3996192632603,1.2876886456361));
#9094=CARTESIAN_POINT('Ctrl Pts',(10.3658589018376,23.4200775574763,1.74033120298424));
#9095=CARTESIAN_POINT('Ctrl Pts',(10.1550289049611,23.4659069337931,2.73033316573101));
#9096=CARTESIAN_POINT('Ctrl Pts',(9.99647915889097,23.4913361835439,3.26338941403484));
#9097=CARTESIAN_POINT('Ctrl Pts',(9.68006758582109,23.5318202650046,4.08312365456022));
#9098=CARTESIAN_POINT('Ctrl Pts',(9.54972305405631,23.5467390083196,4.37931491553579));
#9099=CARTESIAN_POINT('Ctrl Pts',(9.24577669894103,23.5780250103329,4.99162647250862));
#9100=CARTESIAN_POINT('Ctrl Pts',(9.06914863390172,23.5942652616466,5.305776938101));
#9101=CARTESIAN_POINT('Ctrl Pts',(8.62340797158104,23.6317323780177,6.01104391268322));
#9102=CARTESIAN_POINT('Ctrl Pts',(8.34323953991837,23.6529290018979,6.39422899165451));
#9103=CARTESIAN_POINT('Ctrl Pts',(7.61514676227132,23.7040929453002,7.2603481875249));
#9104=CARTESIAN_POINT('Ctrl Pts',(7.1458480924517,23.7342297904803,7.72268928596635));
#9105=CARTESIAN_POINT('Ctrl Pts',(6.41536461271097,23.777665886549,8.31838137924427));
#9106=CARTESIAN_POINT('Ctrl Pts',(6.18704025795914,23.7908046197879,8.4895763911214));
#9107=CARTESIAN_POINT('Ctrl Pts',(5.65868170174971,23.8201057109058,8.85308455988577));
#9108=CARTESIAN_POINT('Ctrl Pts',(5.35526513543522,23.8361272906311,9.03985196730476));
#9109=CARTESIAN_POINT('Ctrl Pts',(4.63496995130448,23.8729884528147,9.43421355827906));
#9110=CARTESIAN_POINT('Ctrl Pts',(4.21261409007777,23.8937966225121,9.63022376952958));
#9111=CARTESIAN_POINT('Ctrl Pts',(3.21948087009429,23.9419578780391,10.0132479869728));
#9112=CARTESIAN_POINT('Ctrl Pts',(2.64287647158049,23.9694124821907,10.1806367538641));
#9113=CARTESIAN_POINT('Ctrl Pts',(1.75287456069259,24.0112332109821,10.3582552497805));
#9114=CARTESIAN_POINT('Ctrl Pts',(1.44807074470326,24.0254447667837,10.4052445727814));
#9115=CARTESIAN_POINT('Ctrl Pts',(0.555767135274358,24.0665008850491,10.5028318669704));
#9116=CARTESIAN_POINT('Ctrl Pts',(-0.0344499151844701,24.092764140141,10.5174700191434));
#9117=CARTESIAN_POINT('Ctrl Pts',(-1.15924631420159,24.1433699730843,10.4506437241561));
#9118=CARTESIAN_POINT('Ctrl Pts',(-1.69245673400647,24.1676350826749,10.377638272027));
#9119=CARTESIAN_POINT('Ctrl Pts',(-2.8435682224278,24.2215227181855,10.1289233613513));
#9120=CARTESIAN_POINT('Ctrl Pts',(-3.45572680846813,24.2511967049917,9.93674531730604));
#9121=CARTESIAN_POINT('Ctrl Pts',(-4.3790713293582,24.2969111099058,9.55115615584327));
#9122=CARTESIAN_POINT('Ctrl Pts',(-4.7042142993661,24.313121006967,9.39527652413933));
#9123=CARTESIAN_POINT('Ctrl Pts',(-5.4277437100935,24.3500962416154,9.00140953445909));
#9124=CARTESIAN_POINT('Ctrl Pts',(-5.81966103042136,24.3708325236976,8.75313178819298));
#9125=CARTESIAN_POINT('Ctrl Pts',(-6.67746466046599,24.418901899173,8.12656570111863));
#9126=CARTESIAN_POINT('Ctrl Pts',(-7.12992670676351,24.446338259833,7.73263979066241));
#9127=CARTESIAN_POINT('Ctrl Pts',(-7.75954682546717,24.4880610182181,7.08198012569272));
#9128=CARTESIAN_POINT('Ctrl Pts',(-7.96300872057675,24.5021958701584,6.85240862926559));
#9129=CARTESIAN_POINT('Ctrl Pts',(-8.52488338439856,24.54299408193,6.15955360840909));
#9130=CARTESIAN_POINT('Ctrl Pts',(-8.85495584636693,24.5690851036403,5.67481298086184));
#9131=CARTESIAN_POINT('Ctrl Pts',(-9.40791733758965,24.6195732197068,4.69599439798748));
#9132=CARTESIAN_POINT('Ctrl Pts',(-9.63641966303246,24.6438970363864,4.20721614263459));
#9133=CARTESIAN_POINT('Ctrl Pts',(-10.0522541068766,24.6978520280123,3.10376689292687));
#9134=CARTESIAN_POINT('Ctrl Pts',(-10.2228003983249,24.7275331235944,2.48505934808134));
#9135=CARTESIAN_POINT('Ctrl Pts',(-10.3984690151572,24.772976314344,1.50608121476103));
#9136=CARTESIAN_POINT('Ctrl Pts',(-10.4433459744648,24.7889144646162,1.15454178886592));
#9137=CARTESIAN_POINT('Ctrl Pts',(-10.505929849523,24.8257262803297,0.336875177503686));
#9138=CARTESIAN_POINT('Ctrl Pts',(-10.5105315440466,24.8465674105374,-0.12949535687918));
#9139=CARTESIAN_POINT('Ctrl Pts',(-10.4472377535106,24.8971385399517,-1.245462253474));
#9140=CARTESIAN_POINT('Ctrl Pts',(-10.349801139714,24.9270426025443,-1.89143581293053));
#9141=CARTESIAN_POINT('Ctrl Pts',(-10.1257429083098,24.9699953718586,-2.79622626179373));
#9142=CARTESIAN_POINT('Ctrl Pts',(-10.0475087846972,24.9829011928103,-3.06547232081995));
#9143=CARTESIAN_POINT('Ctrl Pts',(-9.92043121505545,25.0011979718126,-3.44536206030048));
#9144=CARTESIAN_POINT('Ctrl Pts',(-9.88031276594183,25.0066686769615,-3.55877603111409));
#9145=CARTESIAN_POINT('Ctrl Pts',(-9.83826089299223,25.0121157186286,-3.67146069043641));
#9146=CARTESIAN_POINT('Origin',(0.,20.,0.));
#9147=CARTESIAN_POINT('',(-9.83826091084007,28.8291247138027,-3.67146064261029));
#9148=CARTESIAN_POINT('',(-9.83826088292329,28.0112119827727,-3.67146071741772));
#9149=CARTESIAN_POINT('',(-9.83826089695937,20.,-3.67146067980583));
#9150=CARTESIAN_POINT('Ctrl Pts',(-9.83826091084007,28.8291247138027,-3.67146064261029));
#9151=CARTESIAN_POINT('Ctrl Pts',(-9.87865592041323,28.8238131018187,-3.56321580973253));
#9152=CARTESIAN_POINT('Ctrl Pts',(-9.91726649557972,28.8185104352702,-3.45429895222306));
#9153=CARTESIAN_POINT('Ctrl Pts',(-10.1463566686194,28.7856088690282,-2.77252060102908));
#9154=CARTESIAN_POINT('Ctrl Pts',(-10.2889335781495,28.7587218828267,-2.18478333336485));
#9155=CARTESIAN_POINT('Ctrl Pts',(-10.460636635831,28.7077180821375,-1.06244929267068));
#9156=CARTESIAN_POINT('Ctrl Pts',(-10.5010088482604,28.6836978808386,-0.531517047903976));
#9157=CARTESIAN_POINT('Ctrl Pts',(-10.5009915652785,28.6361742225104,0.506848100517199));
#9158=CARTESIAN_POINT('Ctrl Pts',(-10.4643124591535,28.6127661383962,1.012854700152));
#9159=CARTESIAN_POINT('Ctrl Pts',(-10.349077464141,28.5760384018781,1.80364652905196));
#9160=CARTESIAN_POINT('Ctrl Pts',(-10.2948284982149,28.5626854573338,2.09118625213222));
#9161=CARTESIAN_POINT('Ctrl Pts',(-10.1524018818668,28.5342484550003,2.70430645000063));
#9162=CARTESIAN_POINT('Ctrl Pts',(-10.0604050604299,28.5191670709985,3.02866161267971));
#9163=CARTESIAN_POINT('Ctrl Pts',(-9.78078089020341,28.4798136980383,3.8599232156621));
#9164=CARTESIAN_POINT('Ctrl Pts',(-9.56935865845635,28.4555078685281,4.35775621233012));
#9165=CARTESIAN_POINT('Ctrl Pts',(-9.10866277396772,28.4098552854066,5.24546805337249));
#9166=CARTESIAN_POINT('Ctrl Pts',(-8.87012987032504,28.3886625424817,5.63945549867554));
#9167=CARTESIAN_POINT('Ctrl Pts',(-8.39481116936552,28.3504421612671,6.31939104680849));
#9168=CARTESIAN_POINT('Ctrl Pts',(-8.16724069797434,28.333462568094,6.61088141490322));
#9169=CARTESIAN_POINT('Ctrl Pts',(-7.73920684218572,28.3039186601339,7.10321544846201));
#9170=CARTESIAN_POINT('Ctrl Pts',(-7.54509277020654,28.2912278366045,7.30907454270442));
#9171=CARTESIAN_POINT('Ctrl Pts',(-6.87626451667295,28.249253774505,7.96329609522314));
#9172=CARTESIAN_POINT('Ctrl Pts',(-6.36809015951772,28.2199823966844,8.37523151930707));
#9173=CARTESIAN_POINT('Ctrl Pts',(-5.43481699171802,28.1687475870897,8.99742455172715));
#9174=CARTESIAN_POINT('Ctrl Pts',(-5.02767534204249,28.1471316927054,9.23110799371259));
#9175=CARTESIAN_POINT('Ctrl Pts',(-4.29994499453645,28.1098356133824,9.58632782094374));
#9176=CARTESIAN_POINT('Ctrl Pts',(-3.98649222318385,28.0941873969082,9.72085906386877));
#9177=CARTESIAN_POINT('Ctrl Pts',(-3.40413257847277,28.0660391936369,9.93788732317606));
#9178=CARTESIAN_POINT('Ctrl Pts',(-3.13739759613245,28.0534477669827,10.0252911521772));
#9179=CARTESIAN_POINT('Ctrl Pts',(-2.24047447567557,28.0116178341672,10.2798875697885));
#9180=CARTESIAN_POINT('Ctrl Pts',(-1.59827124573953,27.9823970318907,10.3991019236625));
#9181=CARTESIAN_POINT('Ctrl Pts',(-0.484954907263053,27.931344590157,10.5001475895433));
#9182=CARTESIAN_POINT('Ctrl Pts',(-0.0184444661739987,27.9098617345736,
10.5113239048773));
#9183=CARTESIAN_POINT('Ctrl Pts',(0.80045003192573,27.8721083103663,10.4764142106946));
#9184=CARTESIAN_POINT('Ctrl Pts',(1.15267038956768,27.8558777032382,10.4435310354543));
#9185=CARTESIAN_POINT('Ctrl Pts',(1.78542266794532,27.8269296983462,10.3520502820949));
#9186=CARTESIAN_POINT('Ctrl Pts',(2.06649138533566,27.8141079633993,10.2996260059725));
#9187=CARTESIAN_POINT('Ctrl Pts',(2.98725169581614,27.77173041069,10.0886752059421));
#9188=CARTESIAN_POINT('Ctrl Pts',(3.61414735214316,27.7421777932464,9.88144496242516));
#9189=CARTESIAN_POINT('Ctrl Pts',(4.65307470562964,27.6903362940943,9.42582279508626));
#9190=CARTESIAN_POINT('Ctrl Pts',(5.07518644878895,27.6683996593876,9.20541754112403));
#9191=CARTESIAN_POINT('Ctrl Pts',(5.78555358165188,27.630055308456,8.77074345285593));
#9192=CARTESIAN_POINT('Ctrl Pts',(6.08051194093631,27.6136918223141,8.56889497459747));
#9193=CARTESIAN_POINT('Ctrl Pts',(6.62300614190321,27.5828647896981,8.15550868870517));
#9194=CARTESIAN_POINT('Ctrl Pts',(6.87212015002063,27.5683179981145,7.94672893050593));
#9195=CARTESIAN_POINT('Ctrl Pts',(7.51850943189882,27.5289058692825,7.35183672079408));
#9196=CARTESIAN_POINT('Ctrl Pts',(7.89557003381352,27.5040110994093,6.94531806600125));
#9197=CARTESIAN_POINT('Ctrl Pts',(8.52232467977584,27.4578818150736,6.15223976145366));
#9198=CARTESIAN_POINT('Ctrl Pts',(8.78209427500418,27.4368254140924,5.7753685342449));
#9199=CARTESIAN_POINT('Ctrl Pts',(9.21023571901058,27.3983421045552,5.05820620088779));
#9200=CARTESIAN_POINT('Ctrl Pts',(9.38634076996834,27.3809665043756,4.72340085038933));
#9201=CARTESIAN_POINT('Ctrl Pts',(9.66153206116036,27.3510852179623,4.12373496024748));
#9202=CARTESIAN_POINT('Ctrl Pts',(9.76869846150711,27.3384413218305,3.86302025304477));
#9203=CARTESIAN_POINT('Ctrl Pts',(10.0886555350229,27.2965501609103,2.98581479684692));
#9204=CARTESIAN_POINT('Ctrl Pts',(10.2545304733166,27.267317565445,2.35385693556927));
#9205=CARTESIAN_POINT('Ctrl Pts',(10.4368743717964,27.2161934001995,1.24945043154621));
#9206=CARTESIAN_POINT('Ctrl Pts',(10.4821394408103,27.1946494940426,0.783719067757864));
#9207=CARTESIAN_POINT('Ctrl Pts',(10.5075148188313,27.1558757564564,-0.0577294557712837));
#9208=CARTESIAN_POINT('Ctrl Pts',(10.4987761814546,27.1387016418583,-0.432338556765475));
#9209=CARTESIAN_POINT('Ctrl Pts',(10.4457119065858,27.1074326089507,-1.12191544444419));
#9210=CARTESIAN_POINT('Ctrl Pts',(10.4070636928996,27.0932258532195,-1.43687872092839));
#9211=CARTESIAN_POINT('Ctrl Pts',(10.2589372280531,27.0533422556544,-2.31349282487628));
#9212=CARTESIAN_POINT('Ctrl Pts',(10.1177536861628,27.0276377850881,-2.8686378727547));
#9213=CARTESIAN_POINT('Ctrl Pts',(9.78290341033973,26.9805648681496,-3.84407294962027));
#9214=CARTESIAN_POINT('Ctrl Pts',(9.60536923028663,26.9594022522756,-4.26836825030155));
#9215=CARTESIAN_POINT('Ctrl Pts',(9.23513606089142,26.9211264220879,-5.01210178079168));
#9216=CARTESIAN_POINT('Ctrl Pts',(9.05212486952971,26.904062007347,-5.33553687625689));
#9217=CARTESIAN_POINT('Ctrl Pts',(8.70035963719141,26.874446936582,-5.88681505644243));
#9218=CARTESIAN_POINT('Ctrl Pts',(8.5388048770834,26.8617672673773,-6.11879595360297));
#9219=CARTESIAN_POINT('Ctrl Pts',(7.97388556503127,26.8198155424908,-6.86395833918171));
#9220=CARTESIAN_POINT('Ctrl Pts',(7.53208180673409,26.7905560253361,-7.34605306975006));
#9221=CARTESIAN_POINT('Ctrl Pts',(6.70111001494593,26.7393519240148,-8.09849614544494));
#9222=CARTESIAN_POINT('Ctrl Pts',(6.33315604796249,26.717754826784,-8.38937658895251));
#9223=CARTESIAN_POINT('Ctrl Pts',(5.66531986722898,26.6804348274477,-8.84827516267339));
#9224=CARTESIAN_POINT('Ctrl Pts',(5.37433179608604,26.6647445071336,-9.02797837314898));
#9225=CARTESIAN_POINT('Ctrl Pts',(4.51347728910668,26.6202075278006,-9.50321302013761));
#9226=CARTESIAN_POINT('Ctrl Pts',(3.92462964793251,26.5917225675874,-9.76113912543414));
#9227=CARTESIAN_POINT('Ctrl Pts',(2.80818579361606,26.5385947654838,-10.1326921208555));
#9228=CARTESIAN_POINT('Ctrl Pts',(2.28828057551133,26.5141910295174,-10.2626071530311));
#9229=CARTESIAN_POINT('Ctrl Pts',(1.16810232698847,26.4619090371942,-10.4531304803375));
#9230=CARTESIAN_POINT('Ctrl Pts',(0.567868246511755,26.4341067707607,-10.5028553427611));
#9231=CARTESIAN_POINT('Ctrl Pts',(-0.351408512689415,26.3925461627676,-10.4999375061956));
#9232=CARTESIAN_POINT('Ctrl Pts',(-0.669279215390337,26.3782987851555,-10.484476361876));
#9233=CARTESIAN_POINT('Ctrl Pts',(-1.55313663816918,26.3384715239668,-10.4011210371498));
#9234=CARTESIAN_POINT('Ctrl Pts',(-2.1150097324725,26.3128636795486,-10.3015662406973));
#9235=CARTESIAN_POINT('Ctrl Pts',(-3.11016169909518,26.2659035284779,-10.0403558899959));
#9236=CARTESIAN_POINT('Ctrl Pts',(-3.54617229251944,26.2447536668076,-9.89477154102883));
#9237=CARTESIAN_POINT('Ctrl Pts',(-4.31573647487857,26.2064539224273,-9.58039139671548));
#9238=CARTESIAN_POINT('Ctrl Pts',(-4.65251401597445,26.1893531532413,-9.42144416325672));
#9239=CARTESIAN_POINT('Ctrl Pts',(-5.22883403661191,26.1597073858888,-9.11098706163269));
#9240=CARTESIAN_POINT('Ctrl Pts',(-5.47201374754287,26.1470323010079,-8.96704296246385));
#9241=CARTESIAN_POINT('Ctrl Pts',(-6.25667282360332,26.1050892662708,-8.45876478369332));
#9242=CARTESIAN_POINT('Ctrl Pts',(-6.76999237242064,26.0758341315137,-8.05380883545692));
#9243=CARTESIAN_POINT('Ctrl Pts',(-7.58155294914752,26.0246418254573,-7.28082583311357));
#9244=CARTESIAN_POINT('Ctrl Pts',(-7.89870727803254,26.003052135242,-6.93547280967408));
#9245=CARTESIAN_POINT('Ctrl Pts',(-8.4074952058364,25.9655987617559,-6.30110611875553));
#9246=CARTESIAN_POINT('Ctrl Pts',(-8.60987269290143,25.9497695737279,-6.02162932995481));
#9247=CARTESIAN_POINT('Ctrl Pts',(-8.95277371293878,25.9213253381718,-5.49536895439635));
#9248=CARTESIAN_POINT('Ctrl Pts',(-9.09774629233561,25.9086154292961,-5.25188088533478));
#9249=CARTESIAN_POINT('Ctrl Pts',(-9.46534003125153,25.8739996172454,-4.57348815313626));
#9250=CARTESIAN_POINT('Ctrl Pts',(-9.66766124650532,25.8521246578494,-4.12860948690843));
#9251=CARTESIAN_POINT('Ctrl Pts',(-9.83826089696969,25.8299813406324,-3.67146067977821));
#9252=CARTESIAN_POINT('Ctrl Pts',(-9.83826089299223,25.0121157186286,-3.67146069043641));
#9253=CARTESIAN_POINT('Ctrl Pts',(-9.76075300064936,25.0221554312385,-3.87915537395064));
#9254=CARTESIAN_POINT('Ctrl Pts',(-9.67667706671879,25.0321241213543,-4.08437205702527));
#9255=CARTESIAN_POINT('Ctrl Pts',(-9.39493386590707,25.0631086038194,-4.71440637966613));
#9256=CARTESIAN_POINT('Ctrl Pts',(-9.17532054386728,25.0840583919932,-5.12873264663993));
#9257=CARTESIAN_POINT('Ctrl Pts',(-8.5853534378316,25.134762535786,-6.0818138649344));
#9258=CARTESIAN_POINT('Ctrl Pts',(-8.19096716067736,25.1646879750445,-6.60339082686781));
#9259=CARTESIAN_POINT('Ctrl Pts',(-7.56016458876944,25.207771580521,-7.29347011223664));
#9260=CARTESIAN_POINT('Ctrl Pts',(-7.36124113141074,25.2207806331471,-7.49419284956908));
#9261=CARTESIAN_POINT('Ctrl Pts',(-6.88210665288705,25.2506818667835,-7.94015441478219));
#9262=CARTESIAN_POINT('Ctrl Pts',(-6.59647108555561,25.2674084493627,-8.17899853859639));
#9263=CARTESIAN_POINT('Ctrl Pts',(-5.93133099321032,25.304713920329,-8.67762534715816));
#9264=CARTESIAN_POINT('Ctrl Pts',(-5.54623931221407,25.3252690517141,-8.92866693588708));
#9265=CARTESIAN_POINT('Ctrl Pts',(-4.6494360944431,25.3718403495577,-9.43282527750661));
#9266=CARTESIAN_POINT('Ctrl Pts',(-4.1310365331164,25.3979287662914,-9.67108880676581));
#9267=CARTESIAN_POINT('Ctrl Pts',(-3.29696622650543,25.4388329004323,-9.97508104006006));
#9268=CARTESIAN_POINT('Ctrl Pts',(-2.99324090409898,25.4535062711629,-10.0703892329591));
#9269=CARTESIAN_POINT('Ctrl Pts',(-2.10506466790359,25.4955449089419,-10.3053569839323));
#9270=CARTESIAN_POINT('Ctrl Pts',(-1.51237793076189,25.5223041541911,-10.4088616502049));
#9271=CARTESIAN_POINT('Ctrl Pts',(-0.380666846091074,25.5733287540954,-10.5077496005324));
#9272=CARTESIAN_POINT('Ctrl Pts',(0.155523981271924,25.5975096870528,-10.5134913766237));
#9273=CARTESIAN_POINT('Ctrl Pts',(1.32917141982183,25.651333161507,-10.4362288265948));
#9274=CARTESIAN_POINT('Ctrl Pts',(1.96334113481097,25.6810303074909,-10.3357073884281));
#9275=CARTESIAN_POINT('Ctrl Pts',(2.95246986269504,25.7276465117983,-10.0845500377189));
#9276=CARTESIAN_POINT('Ctrl Pts',(3.3152140893724,25.7447118335475,-9.97118785461763));
#9277=CARTESIAN_POINT('Ctrl Pts',(4.09889665007971,25.7822459427528,-9.67877093641956));
#9278=CARTESIAN_POINT('Ctrl Pts',(4.51589019677931,25.802693588194,-9.49137981413581));
#9279=CARTESIAN_POINT('Ctrl Pts',(5.41111758709042,25.8485735132144,-9.01668622542121));
#9280=CARTESIAN_POINT('Ctrl Pts',(5.88135822648925,25.874065878704,-8.71724865256425));
#9281=CARTESIAN_POINT('Ctrl Pts',(6.58287739329119,25.9145592424325,-8.18783165650493));
#9282=CARTESIAN_POINT('Ctrl Pts',(6.83104727622634,25.9294242228729,-7.98195824528117));
#9283=CARTESIAN_POINT('Ctrl Pts',(7.33765945003296,25.960778306039,-7.52073180747464));
#9284=CARTESIAN_POINT('Ctrl Pts',(7.5931174670888,25.977135738209,-7.26272844811498));
#9285=CARTESIAN_POINT('Ctrl Pts',(8.14956108161896,26.014662332474,-6.63922026589004));
#9286=CARTESIAN_POINT('Ctrl Pts',(8.44021647823084,26.0358033303613,-6.2655673058368));
#9287=CARTESIAN_POINT('Ctrl Pts',(9.07168109751893,26.0868563765776,-5.32973469143728));
#9288=CARTESIAN_POINT('Ctrl Pts',(9.38687688222927,26.1169380608015,-4.75268042787667));
#9289=CARTESIAN_POINT('Ctrl Pts',(9.75869492583654,26.1602934449843,-3.88843960106565));
#9290=CARTESIAN_POINT('Ctrl Pts',(9.86054699868495,26.173409025586,-3.6223893556622));
#9291=CARTESIAN_POINT('Ctrl Pts',(10.0658754506011,26.2027922734766,-3.01290350970603));
#9292=CARTESIAN_POINT('Ctrl Pts',(10.1628282762837,26.218915593411,-2.66765084903357));
#9293=CARTESIAN_POINT('Ctrl Pts',(10.3444142603852,26.2558379303364,-1.86536188076883));
#9294=CARTESIAN_POINT('Ctrl Pts',(10.4167525674532,26.2766068380195,-1.40632236420041));
#9295=CARTESIAN_POINT('Ctrl Pts',(10.5123409898598,26.3247205777358,-0.34731705689704));
#9296=CARTESIAN_POINT('Ctrl Pts',(10.5150351460995,26.3521679604852,0.252876673934817));
#9297=CARTESIAN_POINT('Ctrl Pts',(10.4416651182508,26.3939367716773,1.15632261822086));
#9298=CARTESIAN_POINT('Ctrl Pts',(10.4033527110059,26.4081052652601,1.46140592339454));
#9299=CARTESIAN_POINT('Ctrl Pts',(10.2530593062309,26.4490169093351,2.34319045607481));
#9300=CARTESIAN_POINT('Ctrl Pts',(10.1060337161021,26.4751837781094,2.91270616932516));
#9301=CARTESIAN_POINT('Ctrl Pts',(9.73449756649101,26.5257235690258,3.97494396375965));
#9302=CARTESIAN_POINT('Ctrl Pts',(9.51803608469693,26.5500213790414,4.46851105848206));
#9303=CARTESIAN_POINT('Ctrl Pts',(8.96315700599671,26.6039555873216,5.50846234220355));
#9304=CARTESIAN_POINT('Ctrl Pts',(8.610530850104,26.6336428646415,6.04483960405354));
#9305=CARTESIAN_POINT('Ctrl Pts',(7.98821598006915,26.6792547471245,6.82549740762069));
#9306=CARTESIAN_POINT('Ctrl Pts',(7.75104619252017,26.6953518367844,7.09367998963111));
#9307=CARTESIAN_POINT('Ctrl Pts',(7.17560663216171,26.7322582971608,7.68097440837005));
#9308=CARTESIAN_POINT('Ctrl Pts',(6.82892181902772,26.7530372293412,7.99077721654748));
#9309=CARTESIAN_POINT('Ctrl Pts',(5.9906111882726,26.8011637342064,8.645380300992));
#9310=CARTESIAN_POINT('Ctrl Pts',(5.48766322039095,26.8286136123418,8.97304540426886));
#9311=CARTESIAN_POINT('Ctrl Pts',(4.68844432601075,26.8703960538427,9.40128095225348));
#9312=CARTESIAN_POINT('Ctrl Pts',(4.41109611238629,26.8845752610326,9.53455962749087));
#9313=CARTESIAN_POINT('Ctrl Pts',(3.58790307356012,26.9255229314759,9.8865243228236));
#9314=CARTESIAN_POINT('Ctrl Pts',(3.02907594088133,26.9517138599482,10.0717981834828));
#9315=CARTESIAN_POINT('Ctrl Pts',(1.93464259117908,27.0022700979017,10.335258862224));
#9316=CARTESIAN_POINT('Ctrl Pts',(1.40271844505116,27.0265597097168,10.4207858762804));
#9317=CARTESIAN_POINT('Ctrl Pts',(0.228369115918427,27.0804780387298,10.5180310647503));
#9318=CARTESIAN_POINT('Ctrl Pts',(-0.413348270803016,27.1101576545282,10.5123860107341));
#9319=CARTESIAN_POINT('Ctrl Pts',(-1.40663598019266,27.1557670161011,10.4125147720544));
#9320=CARTESIAN_POINT('Ctrl Pts',(-1.76066499763962,27.171868980435,10.3585303443809));
#9321=CARTESIAN_POINT('Ctrl Pts',(-2.56616123710465,27.2087783859612,10.1932072701764));
#9322=CARTESIAN_POINT('Ctrl Pts',(-3.01436912110219,27.2295554501554,10.0697682236358));
#9323=CARTESIAN_POINT('Ctrl Pts',(-4.01878417821638,27.2776796084062,9.72005053985172));
#9324=CARTESIAN_POINT('Ctrl Pts',(-4.56672628561487,27.3051290545453,9.47496640068579));
#9325=CARTESIAN_POINT('Ctrl Pts',(-5.359722030793,27.3469089750363,9.0354273261699));
#9326=CARTESIAN_POINT('Ctrl Pts',(-5.6220087946756,27.3610861715226,8.87460347217745));
#9327=CARTESIAN_POINT('Ctrl Pts',(-6.36383353765463,27.4020270840498,8.37364397057684));
#9328=CARTESIAN_POINT('Ctrl Pts',(-6.82233664236446,27.4282135003865,8.0045000738226));
#9329=CARTESIAN_POINT('Ctrl Pts',(-7.63688730562669,27.4787666518605,7.22761428973073));
#9330=CARTESIAN_POINT('Ctrl Pts',(-7.99709220919185,27.5030577992767,6.82692843427301));
#9331=CARTESIAN_POINT('Ctrl Pts',(-8.71535856676066,27.5569793595116,5.89268204537063));
#9332=CARTESIAN_POINT('Ctrl Pts',(-9.05844354768592,27.5866606750433,5.35030500272587));
#9333=CARTESIAN_POINT('Ctrl Pts',(-9.51288968886619,27.6322721271269,4.46139273755004));
#9334=CARTESIAN_POINT('Ctrl Pts',(-9.65940689536713,27.6483745054719,4.13460485312264));
#9335=CARTESIAN_POINT('Ctrl Pts',(-9.95704584452271,27.6852841612461,3.36806956048787));
#9336=CARTESIAN_POINT('Ctrl Pts',(-10.0962334208425,27.7060610668963,2.92450347137084));
#9337=CARTESIAN_POINT('Ctrl Pts',(-10.3467201885116,27.7541850252979,1.89086987561539));
#9338=CARTESIAN_POINT('Ctrl Pts',(-10.4377356413369,27.7816344340699,1.29755567173516));
#9339=CARTESIAN_POINT('Ctrl Pts',(-10.4981514713004,27.8234141401926,0.392913033911138));
#9340=CARTESIAN_POINT('Ctrl Pts',(-10.5051552215293,27.8375911663282,0.0853299485340096));
#9341=CARTESIAN_POINT('Ctrl Pts',(-10.4862215596595,27.8785315062419,-0.809591124987056));
#9342=CARTESIAN_POINT('Ctrl Pts',(-10.4245064953328,27.9047175402339,-1.39497411059982));
#9343=CARTESIAN_POINT('Ctrl Pts',(-10.2131096014756,27.9552704302117,-2.50057024650288));
#9344=CARTESIAN_POINT('Ctrl Pts',(-10.0716088916502,27.9795617077902,-3.02045248795448));
#9345=CARTESIAN_POINT('Ctrl Pts',(-9.87370387496888,28.0065212948858,-3.57541525405906));
#9346=CARTESIAN_POINT('Ctrl Pts',(-9.85615642006742,28.0088658143616,-3.62350678937248));
#9347=CARTESIAN_POINT('Ctrl Pts',(-9.83826088292329,28.0112119827727,-3.67146071741772));
#9348=CARTESIAN_POINT('Origin',(0.,20.,0.));
#9349=CARTESIAN_POINT('',(-9.83826093350753,31.8296488111843,-3.67146058186924));
#9350=CARTESIAN_POINT('',(-9.83826089557905,31.0116616139852,-3.67146068350461));
#9351=CARTESIAN_POINT('',(-9.83826089695937,20.,-3.67146067980583));
#9352=CARTESIAN_POINT('',(-10.5010003051392,31.6584104925326,-4.11482518479439E-5));
#9353=CARTESIAN_POINT('Ctrl Pts',(-9.83826093350753,31.8296488111843,-3.67146058186924));
#9354=CARTESIAN_POINT('Ctrl Pts',(-10.0094795081984,31.8076523557889,-3.21265325521828));
#9355=CARTESIAN_POINT('Ctrl Pts',(-10.1484321693502,31.7855438356587,-2.74232807173823));
#9356=CARTESIAN_POINT('Ctrl Pts',(-10.4181972024547,31.7283755090288,-1.520467410793));
#9357=CARTESIAN_POINT('Ctrl Pts',(-10.5009970189966,31.6929958703928,-0.761382904710808));
#9358=CARTESIAN_POINT('Ctrl Pts',(-10.5009999999195,31.6584099621222,-4.11151364069526E-5));
#9359=CARTESIAN_POINT('Ctrl Pts',(-10.5009999999193,31.6584099647158,-4.11722280356519E-5));
#9360=CARTESIAN_POINT('Ctrl Pts',(-10.5010029719109,31.623975496371,0.757966959591466));
#9361=CARTESIAN_POINT('Ctrl Pts',(-10.4189324737747,31.5904413899423,1.51376024549679));
#9362=CARTESIAN_POINT('Ctrl Pts',(-10.1312166813896,31.5297580311426,2.82285787600405));
#9363=CARTESIAN_POINT('Ctrl Pts',(-9.9591335994681,31.5030737741803,3.38019336946323));
#9364=CARTESIAN_POINT('Ctrl Pts',(-9.62657157092227,31.4620254817805,4.2065783101474));
#9365=CARTESIAN_POINT('Ctrl Pts',(-9.49883576393913,31.4478018133524,4.48757204654972));
#9366=CARTESIAN_POINT('Ctrl Pts',(-9.19329425687296,31.4169876093467,5.08799528102228));
#9367=CARTESIAN_POINT('Ctrl Pts',(-9.01081404737691,31.4005399667176,5.40458965930672));
#9368=CARTESIAN_POINT('Ctrl Pts',(-8.5574470493751,31.3631151825095,6.1041403530954));
#9369=CARTESIAN_POINT('Ctrl Pts',(-8.27667154015362,31.3421644954908,6.47974794710526));
#9370=CARTESIAN_POINT('Ctrl Pts',(-7.54702729141367,31.2914589448984,7.33069901596518));
#9371=CARTESIAN_POINT('Ctrl Pts',(-7.07705673809412,31.2615330123196,7.78537069265081));
#9372=CARTESIAN_POINT('Ctrl Pts',(-6.34753993713335,31.2184481879107,8.37015769482052));
#9373=CARTESIAN_POINT('Ctrl Pts',(-6.12008149546854,31.2054384573527,8.53788077642229));
#9374=CARTESIAN_POINT('Ctrl Pts',(-5.57809952373071,31.1755417669533,8.90472709394489));
#9375=CARTESIAN_POINT('Ctrl Pts',(-5.25920760678224,31.1588202271627,9.09670808727943));
#9376=CARTESIAN_POINT('Ctrl Pts',(-4.52532749965072,31.1215181078612,9.48700771984015));
#9377=CARTESIAN_POINT('Ctrl Pts',(-4.10615558996647,31.1009613292202,9.67581446052378));
#9378=CARTESIAN_POINT('Ctrl Pts',(-3.1426498840517,31.0543998783173,10.0358812627618));
#9379=CARTESIAN_POINT('Ctrl Pts',(-2.59400862506019,31.0283233163457,10.1914794378608));
#9380=CARTESIAN_POINT('Ctrl Pts',(-1.72315646797506,30.9874217168502,10.3635460562461));
#9381=CARTESIAN_POINT('Ctrl Pts',(-1.40818649056257,30.9727390482237,10.4110214790555));
#9382=CARTESIAN_POINT('Ctrl Pts',(-0.496105447267984,30.9307770581461,10.5063458167437));
#9383=CARTESIAN_POINT('Ctrl Pts',(0.103554571297619,30.9040991535197,10.5175428444798));
#9384=CARTESIAN_POINT('Ctrl Pts',(1.23615810814353,30.853116318168,10.4417760482636));
#9385=CARTESIAN_POINT('Ctrl Pts',(1.76786438535313,30.8288926177573,10.3650088809611));
#9386=CARTESIAN_POINT('Ctrl Pts',(2.91882883017579,30.7749248798937,10.1076621676343));
#9387=CARTESIAN_POINT('Ctrl Pts',(3.53207512909303,30.7451244531409,9.91003673895346));
#9388=CARTESIAN_POINT('Ctrl Pts',(4.43795670876226,30.7001341715368,9.52326297092287));
#9389=CARTESIAN_POINT('Ctrl Pts',(4.74577646543308,30.6847381374973,9.37366557264447));
#9390=CARTESIAN_POINT('Ctrl Pts',(5.45655018352348,30.6483526025346,8.98423469998865));
#9391=CARTESIAN_POINT('Ctrl Pts',(5.85182343138215,30.6274026682853,8.73192827296279));
#9392=CARTESIAN_POINT('Ctrl Pts',(6.75423761367047,30.5766983083303,8.06703353008391));
#9393=CARTESIAN_POINT('Ctrl Pts',(7.2423188522358,30.5467728018786,7.63187612968911));
#9394=CARTESIAN_POINT('Ctrl Pts',(7.87929346817327,30.503688992417,6.94748378035463));
#9395=CARTESIAN_POINT('Ctrl Pts',(8.06332541754961,30.4906798117367,6.73302177484321));
#9396=CARTESIAN_POINT('Ctrl Pts',(8.46918835254721,30.4607796181574,6.21950751259473));
#9397=CARTESIAN_POINT('Ctrl Pts',(8.68421041660464,30.4440541640326,5.91556575944822));
#9398=CARTESIAN_POINT('Ctrl Pts',(9.12757966406785,30.4067494562523,5.21240502546104));
#9399=CARTESIAN_POINT('Ctrl Pts',(9.3467605432577,30.3861939693831,4.80831974446729));
#9400=CARTESIAN_POINT('Ctrl Pts',(9.77695256372727,30.3396249280172,3.87383297196255));
#9401=CARTESIAN_POINT('Ctrl Pts',(9.97262920115203,30.3135392046698,3.337966894007));
#9402=CARTESIAN_POINT('Ctrl Pts',(10.2083958280231,30.2726356587073,2.48211832055813));
#9403=CARTESIAN_POINT('Ctrl Pts',(10.2789190544463,30.257960187701,2.17165424717177));
#9404=CARTESIAN_POINT('Ctrl Pts',(10.4414565501759,30.215936859755,1.26775671570833));
#9405=CARTESIAN_POINT('Ctrl Pts',(10.4968383957213,30.1891940897518,0.669039387544863));
#9406=CARTESIAN_POINT('Ctrl Pts',(10.5042868157778,30.1381779524306,-0.466779564517998));
#9407=CARTESIAN_POINT('Ctrl Pts',(10.4668101813873,30.1139883520765,-1.00189271282337));
#9408=CARTESIAN_POINT('Ctrl Pts',(10.2951847713318,30.0601486322426,-2.1658595525262));
#9409=CARTESIAN_POINT('Ctrl Pts',(10.1438419931816,30.030443939003,-2.79002392599146));
#9410=CARTESIAN_POINT('Ctrl Pts',(9.81388306759422,29.9838446633388,-3.75533219169576));
#9411=CARTESIAN_POINT('Ctrl Pts',(9.67187482201498,29.9668029547496,-4.10726941975931));
#9412=CARTESIAN_POINT('Ctrl Pts',(9.31750355162947,29.9292850872525,-4.8645496016262));
#9413=CARTESIAN_POINT('Ctrl Pts',(9.09707562871007,29.9088302317151,-5.26525637970499));
#9414=CARTESIAN_POINT('Ctrl Pts',(8.55224960660479,29.8629849568965,-6.11872774650409));
#9415=CARTESIAN_POINT('Ctrl Pts',(8.21653890499678,29.8375357624051,-6.56264167301637));
#9416=CARTESIAN_POINT('Ctrl Pts',(7.63261845744045,29.7970488080632,-7.21931479187445));
#9417=CARTESIAN_POINT('Ctrl Pts',(7.40691609965493,29.7821471167866,-7.45070243484553));
#9418=CARTESIAN_POINT('Ctrl Pts',(6.90719511346969,29.750840913549,-7.91782586000983));
#9419=CARTESIAN_POINT('Ctrl Pts',(6.63095358837488,29.7345648394487,-8.15056865789208));
#9420=CARTESIAN_POINT('Ctrl Pts',(5.96572279077559,29.6970797713222,-8.65480137096482));
#9421=CARTESIAN_POINT('Ctrl Pts',(5.56924809301941,29.6759003705688,-8.91509435014499));
#9422=CARTESIAN_POINT('Ctrl Pts',(4.58426022019142,29.624770997779,-9.47033038367636));
#9423=CARTESIAN_POINT('Ctrl Pts',(3.98296225200876,29.5946514738936,-9.73850963354644));
#9424=CARTESIAN_POINT('Ctrl Pts',(3.09046721182634,29.5512403602524,-10.0399850438766));
#9425=CARTESIAN_POINT('Ctrl Pts',(2.81674775674761,29.5381085529275,-10.1201888279556));
#9426=CARTESIAN_POINT('Ctrl Pts',(2.19395682337431,29.5087837409927,-10.2754473268974));
#9427=CARTESIAN_POINT('Ctrl Pts',(1.84364424209252,29.4927325531931,-10.3440438740099));
#9428=CARTESIAN_POINT('Ctrl Pts',(1.03037329502299,29.4558537217162,-10.4606602287176));
#9429=CARTESIAN_POINT('Ctrl Pts',(0.566365628337865,29.4350571039316,-10.4960138577852));
#9430=CARTESIAN_POINT('Ctrl Pts',(-0.497703865727678,29.3869091447435,-10.5063041963415));
#9431=CARTESIAN_POINT('Ctrl Pts',(-1.09633936813621,29.3594559615501,-10.4607908615899));
#9432=CARTESIAN_POINT('Ctrl Pts',(-1.99177299762381,29.3176500776683,-10.3149740767657));
#9433=CARTESIAN_POINT('Ctrl Pts',(-2.29342159521646,29.3034514706996,-10.2521251320501));
#9434=CARTESIAN_POINT('Ctrl Pts',(-3.16236749142982,29.2624386300888,-10.030803123064));
#9435=CARTESIAN_POINT('Ctrl Pts',(-3.71962300240937,29.2362041996979,-9.83778390824362));
#9436=CARTESIAN_POINT('Ctrl Pts',(-4.74922988451164,29.185618179249,-9.38109078280864));
#9437=CARTESIAN_POINT('Ctrl Pts',(-5.22320775861405,29.1613433504691,-9.12568513083327));
#9438=CARTESIAN_POINT('Ctrl Pts',(-6.21475465024609,29.1074181253387,-8.4887318811753));
#9439=CARTESIAN_POINT('Ctrl Pts',(-6.72112662152996,29.0777157234547,-8.09371285533201));
#9440=CARTESIAN_POINT('Ctrl Pts',(-7.45270245699273,29.0318680506219,-7.40673776204664));
#9441=CARTESIAN_POINT('Ctrl Pts',(-7.70404562399735,29.0155553325848,-7.14494386101737));
#9442=CARTESIAN_POINT('Ctrl Pts',(-8.24398863608406,28.9785163329944,-6.52085947837628));
#9443=CARTESIAN_POINT('Ctrl Pts',(-8.52318560181982,28.95781791939,-6.15144367501544));
#9444=CARTESIAN_POINT('Ctrl Pts',(-9.10012422392409,28.9102582503829,-5.27303831661512));
#9445=CARTESIAN_POINT('Ctrl Pts',(-9.38122216741048,28.883305981918,-4.75497999426468));
#9446=CARTESIAN_POINT('Ctrl Pts',(-9.69612696169593,28.847164576079,-4.03664795901804));
#9447=CARTESIAN_POINT('Ctrl Pts',(-9.76975967869846,28.8381320632105,-3.85502055516978));
#9448=CARTESIAN_POINT('Ctrl Pts',(-9.83826091084007,28.8291247138027,-3.67146064261029));
#9449=CARTESIAN_POINT('Ctrl Pts',(-9.83826088292329,28.0112119827727,-3.67146071741772));
#9450=CARTESIAN_POINT('Ctrl Pts',(-9.63233473390102,28.0382096315146,-4.22327247100276));
#9451=CARTESIAN_POINT('Ctrl Pts',(-9.38031912188069,28.065496103614,-4.75686020923467));
#9452=CARTESIAN_POINT('Ctrl Pts',(-8.90557621356885,28.1087433876724,-5.575793418109));
#9453=CARTESIAN_POINT('Ctrl Pts',(-8.71064440008901,28.1248251234884,-5.87566485887207));
#9454=CARTESIAN_POINT('Ctrl Pts',(-8.22805239493337,28.1617223235901,-6.54109929211968));
#9455=CARTESIAN_POINT('Ctrl Pts',(-7.93065471161723,28.1825071544524,-6.89866199759931));
#9456=CARTESIAN_POINT('Ctrl Pts',(-7.19919120869614,28.230542420745,-7.66805748594574));
#9457=CARTESIAN_POINT('Ctrl Pts',(-6.75167554745295,28.257892170752,-8.06488101351353));
#9458=CARTESIAN_POINT('Ctrl Pts',(-6.02512532181003,28.2996390276788,-8.60606232885609));
#9459=CARTESIAN_POINT('Ctrl Pts',(-5.76934019205613,28.3138825271891,-8.77958769818982));
#9460=CARTESIAN_POINT('Ctrl Pts',(-5.00304875173894,28.3550454604036,-9.25147415735185));
#9461=CARTESIAN_POINT('Ctrl Pts',(-4.47456880442693,28.3813798654994,-9.51832511468678));
#9462=CARTESIAN_POINT('Ctrl Pts',(-3.42852853096244,28.43203473232,-9.94004039354387));
#9463=CARTESIAN_POINT('Ctrl Pts',(-2.91596786447846,28.4562759682461,-10.1022929073331));
#9464=CARTESIAN_POINT('Ctrl Pts',(-1.76698463174089,28.5102728697067,-10.37123329394));
#9465=CARTESIAN_POINT('Ctrl Pts',(-1.12856998007311,28.5400847485167,-10.4599728064787));
#9466=CARTESIAN_POINT('Ctrl Pts',(-0.145070787777347,28.5850553676003,-10.5055452732829));
#9467=CARTESIAN_POINT('Ctrl Pts',(0.196484823710329,28.6004210999214,-10.5047096051333));
#9468=CARTESIAN_POINT('Ctrl Pts',(1.00550151449112,28.636789730861,-10.4632528868762));
#9469=CARTESIAN_POINT('Ctrl Pts',(1.47146700094931,28.6577525681422,-10.407952486264));
#9470=CARTESIAN_POINT('Ctrl Pts',(2.57371132310845,28.7084776633949,-10.2016176558495));
#9471=CARTESIAN_POINT('Ctrl Pts',(3.20264201786382,28.7384108117788,-10.0219776853927));
#9472=CARTESIAN_POINT('Ctrl Pts',(4.0742069902033,28.7815121233764,-9.68254848628005));
#9473=CARTESIAN_POINT('Ctrl Pts',(4.33336691402994,28.7945305032246,-9.56936996621349));
#9474=CARTESIAN_POINT('Ctrl Pts',(4.92101182835283,28.8243737855602,-9.28396417582688));
#9475=CARTESIAN_POINT('Ctrl Pts',(5.2455679906417,28.8410353906497,-9.10452461256677));
#9476=CARTESIAN_POINT('Ctrl Pts',(5.94995049113592,28.8782980508488,-8.6648959961835));
#9477=CARTESIAN_POINT('Ctrl Pts',(6.32352711746613,28.8988747719579,-8.39614989546143));
#9478=CARTESIAN_POINT('Ctrl Pts',(7.1209088982611,28.9456457421507,-7.73903235280749));
#9479=CARTESIAN_POINT('Ctrl Pts',(7.53289270146961,28.9719163864062,-7.33862828664188));
#9480=CARTESIAN_POINT('Ctrl Pts',(8.11829189114373,29.0129279808974,-6.66817273702931));
#9481=CARTESIAN_POINT('Ctrl Pts',(8.31558950329078,29.0275252066665,-6.42044893059705));
#9482=CARTESIAN_POINT('Ctrl Pts',(8.72201361299088,29.0592038169341,-5.85992567878681));
#9483=CARTESIAN_POINT('Ctrl Pts',(8.92613363015351,29.0761303892718,-5.5440412265667));
#9484=CARTESIAN_POINT('Ctrl Pts',(9.34482163716742,29.1139560856039,-4.81281480529713));
#9485=CARTESIAN_POINT('Ctrl Pts',(9.54949020363153,29.1348354722129,-4.39273379914329));
#9486=CARTESIAN_POINT('Ctrl Pts',(9.97137368278544,29.1854419308279,-3.3567262459062));
#9487=CARTESIAN_POINT('Ctrl Pts',(10.1604649521668,29.2153416361926,-2.73144948306346));
#9488=CARTESIAN_POINT('Ctrl Pts',(10.3464009860724,29.2583356301675,-1.81715629618003));
#9489=CARTESIAN_POINT('Ctrl Pts',(10.3913488019078,29.271284666685,-1.53946192602653));
#9490=CARTESIAN_POINT('Ctrl Pts',(10.4657500100949,29.2996015140777,-0.924019887580983));
#9491=CARTESIAN_POINT('Ctrl Pts',(10.4901081552804,29.3148513170999,-0.585977830003707));
#9492=CARTESIAN_POINT('Ctrl Pts',(10.5091543523551,29.3511563112881,0.222412656326963));
#9493=CARTESIAN_POINT('Ctrl Pts',(10.4886797662731,29.3721694805039,0.692376564799234));
#9494=CARTESIAN_POINT('Ctrl Pts',(10.3646502019633,29.4229807083489,1.80889330690969));
#9495=CARTESIAN_POINT('Ctrl Pts',(10.2320267467071,29.4529490877228,2.4502361318087));
#9496=CARTESIAN_POINT('Ctrl Pts',(9.95768563518145,29.4961204860435,3.34601210296476));
#9497=CARTESIAN_POINT('Ctrl Pts',(9.86377048821956,29.5091712328104,3.61349339708788));
#9498=CARTESIAN_POINT('Ctrl Pts',(9.62403962161938,29.5388356072155,4.21696526542007));
#9499=CARTESIAN_POINT('Ctrl Pts',(9.47124289687231,29.5552931414798,4.54977980898371));
#9500=CARTESIAN_POINT('Ctrl Pts',(9.08724967436104,29.5924236753195,5.28258781618324));
#9501=CARTESIAN_POINT('Ctrl Pts',(8.84642545296598,29.6130703647793,5.67667088795452));
#9502=CARTESIAN_POINT('Ctrl Pts',(8.23595657122771,29.6609979484473,6.54195421661666));
#9503=CARTESIAN_POINT('Ctrl Pts',(7.85039218358787,29.6883834983227,6.99996121813689));
#9504=CARTESIAN_POINT('Ctrl Pts',(7.21253448019393,29.7299672068082,7.63827535937103));
#9505=CARTESIAN_POINT('Ctrl Pts',(6.98779898455277,29.7440177658395,7.84439748659218));
#9506=CARTESIAN_POINT('Ctrl Pts',(6.29098588322203,29.7856360743679,8.4297581958081));
#9507=CARTESIAN_POINT('Ctrl Pts',(5.79477555917899,29.8125842367786,8.7782635753352));
#9508=CARTESIAN_POINT('Ctrl Pts',(4.81399661231949,29.863532448144,9.34751391886051));
#9509=CARTESIAN_POINT('Ctrl Pts',(4.33730619892938,29.8874258788524,9.57801309186884));
#9510=CARTESIAN_POINT('Ctrl Pts',(3.24498406131828,29.9411576434858,10.0078599991292));
#9511=CARTESIAN_POINT('Ctrl Pts',(2.62418553411607,29.9710647030443,10.1882688167627));
#9512=CARTESIAN_POINT('Ctrl Pts',(1.58923252694129,30.0191758100296,10.3880982672269));
#9513=CARTESIAN_POINT('Ctrl Pts',(1.18351196804469,30.037513931895,10.4421046784482));
#9514=CARTESIAN_POINT('Ctrl Pts',(0.144862686981982,30.0842356954535,10.5190357669806));
#9515=CARTESIAN_POINT('Ctrl Pts',(-0.4888616783407,30.1126184177228,10.5086673993383));
#9516=CARTESIAN_POINT('Ctrl Pts',(-1.5818551808535,30.1628211623336,10.391658493651));
#9517=CARTESIAN_POINT('Ctrl Pts',(-2.0420945023228,30.1843322759007,10.3110946018329));
#9518=CARTESIAN_POINT('Ctrl Pts',(-2.86060133256157,30.2231445594523,10.1108499331129));
#9519=CARTESIAN_POINT('Ctrl Pts',(-3.22071534644785,30.2403892234578,10.0019666444908));
#9520=CARTESIAN_POINT('Ctrl Pts',(-3.8718038180859,30.2716960682434,9.76628349993863));
#9521=CARTESIAN_POINT('Ctrl Pts',(-4.16436479706541,30.2858726134789,9.64516602787594));
#9522=CARTESIAN_POINT('Ctrl Pts',(-4.9706455322075,30.3258082299518,9.26783910065944));
#9523=CARTESIAN_POINT('Ctrl Pts',(-5.46946745949984,30.3515947339942,8.98248657036646));
#9524=CARTESIAN_POINT('Ctrl Pts',(-6.32152632643401,30.398766799773,8.39765887737398));
#9525=CARTESIAN_POINT('Ctrl Pts',(-6.68307917688397,30.4199437237763,8.11287939219596));
#9526=CARTESIAN_POINT('Ctrl Pts',(-7.30017914791703,30.4581930889483,7.55748934682719));
#9527=CARTESIAN_POINT('Ctrl Pts',(-7.56225810640208,30.4752170860831,7.29524017171136));
#9528=CARTESIAN_POINT('Ctrl Pts',(-7.99890840640804,30.5047981949374,6.80943323918421));
#9529=CARTESIAN_POINT('Ctrl Pts',(-8.17931770227583,30.5174831260515,6.5916372765147));
#9530=CARTESIAN_POINT('Ctrl Pts',(-8.74641206874221,30.5594452052333,5.84783705291626));
#9531=CARTESIAN_POINT('Ctrl Pts',(-9.09285357153411,30.5887101334723,5.29310052074037));
#9532=CARTESIAN_POINT('Ctrl Pts',(-9.59577594160372,30.6399284224677,4.29089399154537));
#9533=CARTESIAN_POINT('Ctrl Pts',(-9.77771090054328,30.6615342781933,3.8583735624167));
#9534=CARTESIAN_POINT('Ctrl Pts',(-10.0411628828821,30.6988431170465,3.09234276004025));
#9535=CARTESIAN_POINT('Ctrl Pts',(-10.1363803408675,30.7145138031143,2.76429783978361));
#9536=CARTESIAN_POINT('Ctrl Pts',(-10.3639128066613,30.7590076115742,1.80863771144074));
#9537=CARTESIAN_POINT('Ctrl Pts',(-10.4549714258374,30.7874695772116,1.17279641167473));
#9538=CARTESIAN_POINT('Ctrl Pts',(-10.5146055243684,30.840554819351,-0.00141240276887271));
#9539=CARTESIAN_POINT('Ctrl Pts',(-10.5008966525229,30.8649396524933,-0.536728397122199));
#9540=CARTESIAN_POINT('Ctrl Pts',(-10.3852276138976,30.9172365074931,-1.66743429855176));
#9541=CARTESIAN_POINT('Ctrl Pts',(-10.2726032240514,30.9450737385028,-2.25985786975737));
#9542=CARTESIAN_POINT('Ctrl Pts',(-10.0309173198126,30.9854842527832,-3.1204009893133));
#9543=CARTESIAN_POINT('Ctrl Pts',(-9.94031035515241,30.9985682311324,-3.3980029798592));
#9544=CARTESIAN_POINT('Ctrl Pts',(-9.83826089557905,31.0116616139851,-3.67146068350461));
#9545=CARTESIAN_POINT('Origin',(0.,20.,0.));
#9546=CARTESIAN_POINT('',(-9.83826090449497,34.8296849384879,-3.671460659613));
#9547=CARTESIAN_POINT('',(-9.83826088462892,34.0117278664922,-3.67146071284722));
#9548=CARTESIAN_POINT('',(-9.83826089695937,20.,-3.67146067980583));
#9549=CARTESIAN_POINT('Ctrl Pts',(-9.83826090449497,34.8296849384879,-3.67146065961299));
#9550=CARTESIAN_POINT('Ctrl Pts',(-9.87013633268989,34.8254908533905,-3.58604539628911));
#9551=CARTESIAN_POINT('Ctrl Pts',(-9.90090469256612,34.8212920122283,-3.5002008550201));
#9552=CARTESIAN_POINT('Ctrl Pts',(-10.0381989019327,34.8018370504582,-3.10083688152188));
#9553=CARTESIAN_POINT('Ctrl Pts',(-10.1309726508253,34.7865611629162,-2.78280827432138));
#9554=CARTESIAN_POINT('Ctrl Pts',(-10.2898789181953,34.7555197163493,-2.12362392381044));
#9555=CARTESIAN_POINT('Ctrl Pts',(-10.3544230567936,34.7398574003433,-1.78250223045051));
#9556=CARTESIAN_POINT('Ctrl Pts',(-10.4679052283791,34.7026484492834,-0.962071396842471));
#9557=CARTESIAN_POINT('Ctrl Pts',(-10.5009950583733,34.6811443202572,-0.481374431363444));
#9558=CARTESIAN_POINT('Ctrl Pts',(-10.5010059971665,34.6329869416597,0.584074227527096));
#9559=CARTESIAN_POINT('Ctrl Pts',(-10.4522641003492,34.6062739922244,1.1672253169037));
#9560=CARTESIAN_POINT('Ctrl Pts',(-10.2712639095788,34.556047637444,2.24239017538735));
#9561=CARTESIAN_POINT('Ctrl Pts',(-10.1512619301906,34.5326917969161,2.73479225064487));
#9562=CARTESIAN_POINT('Ctrl Pts',(-9.79660557440828,34.480295246905,3.83694637694141));
#9563=CARTESIAN_POINT('Ctrl Pts',(-9.5396883845809,34.4513608581882,4.43734175670019));
#9564=CARTESIAN_POINT('Ctrl Pts',(-8.95746364100407,34.3962142269396,5.50983150560361));
#9565=CARTESIAN_POINT('Ctrl Pts',(-8.64600107367251,34.3702280086654,5.98673832377566));
#9566=CARTESIAN_POINT('Ctrl Pts',(-7.98461654538339,34.3205292275213,6.83940487991358));
#9567=CARTESIAN_POINT('Ctrl Pts',(-7.64276005766471,34.296951349283,7.21940490641383));
#9568=CARTESIAN_POINT('Ctrl Pts',(-7.07530876290363,34.2613049116018,7.7644951896326));
#9569=CARTESIAN_POINT('Ctrl Pts',(-6.86851775670562,34.2488991110006,7.94800897823506));
#9570=CARTESIAN_POINT('Ctrl Pts',(-6.14770234010226,34.2070910557485,8.53852227459741));
#9571=CARTESIAN_POINT('Ctrl Pts',(-5.60291145794244,34.1777169263762,8.90550211149995));
#9572=CARTESIAN_POINT('Ctrl Pts',(-4.62018427710503,34.12660652522,9.44140473596752));
#9573=CARTESIAN_POINT('Ctrl Pts',(-4.19861787549921,34.1052293693084,9.63627644832546));
#9574=CARTESIAN_POINT('Ctrl Pts',(-3.43035923345287,34.0673184054502,9.93139337493067));
#9575=CARTESIAN_POINT('Ctrl Pts',(-3.08876700801998,34.0508276702708,10.042881669787));
#9576=CARTESIAN_POINT('Ctrl Pts',(-2.46738715424225,34.021679306244,10.2109748284553));
#9577=CARTESIAN_POINT('Ctrl Pts',(-2.18973698849106,34.008909624726,10.2740966311617));
#9578=CARTESIAN_POINT('Ctrl Pts',(-1.26512575620733,33.9667255212829,10.4451120393492));
#9579=CARTESIAN_POINT('Ctrl Pts',(-0.610648105926783,33.9373179263997,10.5037133309675));
#9580=CARTESIAN_POINT('Ctrl Pts',(0.517447316625793,33.8857764482132,10.4988789282049));
#9581=CARTESIAN_POINT('Ctrl Pts',(0.989214235355772,33.8639920030632,10.4649727950989));
#9582=CARTESIAN_POINT('Ctrl Pts',(1.81725123890417,33.8254891572408,10.3489548272268));
#9583=CARTESIAN_POINT('Ctrl Pts',(2.17456437111616,33.8088198402017,10.2798129469653));
#9584=CARTESIAN_POINT('Ctrl Pts',(2.84004022142136,33.777827180874,10.1147816930769));
#9585=CARTESIAN_POINT('Ctrl Pts',(3.1487755355104,33.7634098659188,10.0229663018507));
#9586=CARTESIAN_POINT('Ctrl Pts',(3.97884962762206,33.7239776381315,9.73396229696878));
#9587=CARTESIAN_POINT('Ctrl Pts',(4.48947632726099,33.6989348997777,9.50925078789113));
#9588=CARTESIAN_POINT('Ctrl Pts',(5.38185766584579,33.6526821209184,9.02857129310746));
#9589=CARTESIAN_POINT('Ctrl Pts',(5.76930053070901,33.6316563254727,8.78604873819855));
#9590=CARTESIAN_POINT('Ctrl Pts',(6.44800700312271,33.5931095733654,8.29690377244693));
#9591=CARTESIAN_POINT('Ctrl Pts',(6.74401474077003,33.5756406005176,8.05814423722092));
#9592=CARTESIAN_POINT('Ctrl Pts',(7.23567168159055,33.5456780391768,7.61546636469039));
#9593=CARTESIAN_POINT('Ctrl Pts',(7.43724914870386,33.5330434761281,7.41873311618829));
#9594=CARTESIAN_POINT('Ctrl Pts',(8.07851750994854,33.4911654907862,6.74043805931232));
#9595=CARTESIAN_POINT('Ctrl Pts',(8.48126699105468,33.4619372844473,6.22607724549495));
#9596=CARTESIAN_POINT('Ctrl Pts',(9.08630087861113,33.4108296182019,5.28472989311774));
#9597=CARTESIAN_POINT('Ctrl Pts',(9.31237542967223,33.3892979492435,4.87533458854948));
#9598=CARTESIAN_POINT('Ctrl Pts',(9.66942584208554,33.3505099838225,4.11264165144949));
#9599=CARTESIAN_POINT('Ctrl Pts',(9.81011440460812,33.3333097001856,3.76474308258486));
#9600=CARTESIAN_POINT('Ctrl Pts',(10.0348042768741,33.302026797313,3.11032660483451));
#9601=CARTESIAN_POINT('Ctrl Pts',(10.1240943721748,33.2878314013858,2.8060907455077));
#9602=CARTESIAN_POINT('Ctrl Pts',(10.3357079403615,33.247928484519,1.94215663404644));
#9603=CARTESIAN_POINT('Ctrl Pts',(10.4262118827604,33.2221934079735,1.37583340133174));
#9604=CARTESIAN_POINT('Ctrl Pts',(10.5053297003632,33.1750835843259,0.346762646039677));
#9605=CARTESIAN_POINT('Ctrl Pts',(10.5104404522202,33.1539157153092,-0.113258737358978));
#9606=CARTESIAN_POINT('Ctrl Pts',(10.4651880088415,33.1156496581278,-0.942605781500887));
#9607=CARTESIAN_POINT('Ctrl Pts',(10.4253514217436,33.098600139274,-1.31176579931775));
#9608=CARTESIAN_POINT('Ctrl Pts',(10.3208952683169,33.0689976127102,-1.95703721848463));
#9609=CARTESIAN_POINT('Ctrl Pts',(10.2644883953892,33.0563160316584,-2.2340893270028));
#9610=CARTESIAN_POINT('Ctrl Pts',(10.041088696114,33.0143605989711,-3.14219107947203));
#9611=CARTESIAN_POINT('Ctrl Pts',(9.82648095911503,32.9850991701866,-3.75993030389822));
#9612=CARTESIAN_POINT('Ctrl Pts',(9.36165983621652,32.9338900091296,-4.78015711496229));
#9613=CARTESIAN_POINT('Ctrl Pts',(9.13905893701823,32.9122897687789,-5.19308853275904));
#9614=CARTESIAN_POINT('Ctrl Pts',(8.70777308487517,32.8749737998869,-5.87898010982293));
#9615=CARTESIAN_POINT('Ctrl Pts',(8.51190435680739,32.8592905508418,-6.15915713765298));
#9616=CARTESIAN_POINT('Ctrl Pts',(7.90966258317944,32.8147389731778,-6.9368857146172));
#9617=CARTESIAN_POINT('Ctrl Pts',(7.47088088258671,32.7862332018928,-7.40736825144903));
#9618=CARTESIAN_POINT('Ctrl Pts',(6.59226331426678,32.7330610427167,-8.19145537949761));
#9619=CARTESIAN_POINT('Ctrl Pts',(6.16595443142408,32.7086342560755,-8.51697476988249));
#9620=CARTESIAN_POINT('Ctrl Pts',(5.21318211352657,32.6563709747048,-9.13531791234831));
#9621=CARTESIAN_POINT('Ctrl Pts',(4.68256757704756,32.6286119105837,-9.41832823497058));
#9622=CARTESIAN_POINT('Ctrl Pts',(3.83812832133132,32.5870875851872,-9.77962272300775));
#9623=CARTESIAN_POINT('Ctrl Pts',(3.5400433955146,32.5728350665806,-9.891427907448));
#9624=CARTESIAN_POINT('Ctrl Pts',(2.69553446102158,32.5330091446118,-10.1651108589706));
#9625=CARTESIAN_POINT('Ctrl Pts',(2.14035208403521,32.5074076986813,-10.296322581333));
#9626=CARTESIAN_POINT('Ctrl Pts',(1.12328449695624,32.4604531191923,-10.4508423149459));
#9627=CARTESIAN_POINT('Ctrl Pts',(0.665255284381629,32.4393021605012,-10.4899617799723));
#9628=CARTESIAN_POINT('Ctrl Pts',(-0.165842753504508,32.4010044834549,-10.5062803531098));
#9629=CARTESIAN_POINT('Ctrl Pts',(-0.537968685621155,32.3839068517497,-10.4938094379395));
#9630=CARTESIAN_POINT('Ctrl Pts',(-1.19007607645678,32.354263738098,-10.4371698539277));
#9631=CARTESIAN_POINT('Ctrl Pts',(-1.47039813209097,32.3415882620907,-10.4013810758494));
#9632=CARTESIAN_POINT('Ctrl Pts',(-2.39225583406765,32.2996444969063,-10.2456711986442));
#9633=CARTESIAN_POINT('Ctrl Pts',(-3.02403528342239,32.2703889992753,-10.0772939761365));
#9634=CARTESIAN_POINT('Ctrl Pts',(-4.07549501224391,32.2191957053056,-9.68920649976376));
#9635=CARTESIAN_POINT('Ctrl Pts',(-4.50355433057597,32.1976053902157,-9.4978087160507));
#9636=CARTESIAN_POINT('Ctrl Pts',(-5.22369264015762,32.1600678617824,-9.11615071658563));
#9637=CARTESIAN_POINT('Ctrl Pts',(-5.52177054628588,32.1441563014154,-8.93874893922606));
#9638=CARTESIAN_POINT('Ctrl Pts',(-6.04824302722397,32.1155373506617,-8.58901609167487));
#9639=CARTESIAN_POINT('Ctrl Pts',(-6.27941783779057,32.1027340047969,-8.42148182420838));
#9640=CARTESIAN_POINT('Ctrl Pts',(-7.01978009718587,32.0604301251586,-7.83748106677449));
#9641=CARTESIAN_POINT('Ctrl Pts',(-7.49667198872497,32.0309341063268,-7.38263550097256));
#9642=CARTESIAN_POINT('Ctrl Pts',(-8.23899565964519,31.9792083802575,-6.52801900409605));
#9643=CARTESIAN_POINT('Ctrl Pts',(-8.52547493261577,31.9573297821157,-6.14917464006969));
#9644=CARTESIAN_POINT('Ctrl Pts',(-8.98229265647638,31.9189310046498,-5.45148389254653));
#9645=CARTESIAN_POINT('Ctrl Pts',(-9.16366221499971,31.9024568708651,-5.14077510401679));
#9646=CARTESIAN_POINT('Ctrl Pts',(-9.47731248523631,31.871579186215,-4.53390107052915));
#9647=CARTESIAN_POINT('Ctrl Pts',(-9.61251774001361,31.8570883740581,-4.23971900875921));
#9648=CARTESIAN_POINT('Ctrl Pts',(-9.76993596611932,31.8382643952994,-3.85078765283611));
#9649=CARTESIAN_POINT('Ctrl Pts',(-9.80471763308074,31.8339581199903,-3.76134517542839));
#9650=CARTESIAN_POINT('Ctrl Pts',(-9.83826093350753,31.8296488111843,-3.67146058186924));
#9651=CARTESIAN_POINT('Ctrl Pts',(-9.83826089557905,31.0116616139852,-3.67146068350461));
#9652=CARTESIAN_POINT('Ctrl Pts',(-9.82914856923431,31.0128307644932,-3.69587860641687));
#9653=CARTESIAN_POINT('Ctrl Pts',(-9.81994500822106,31.0139999610707,-3.72026348698511));
#9654=CARTESIAN_POINT('Ctrl Pts',(-9.60744622470539,31.0407334114432,-4.27699665625298));
#9655=CARTESIAN_POINT('Ctrl Pts',(-9.36124837708719,31.0663477931998,-4.79194460643673));
#9656=CARTESIAN_POINT('Ctrl Pts',(-8.84343503861281,31.1133136620883,-5.68115199578211));
#9657=CARTESIAN_POINT('Ctrl Pts',(-8.58659952399314,31.1344624286705,-6.06235346052566));
#9658=CARTESIAN_POINT('Ctrl Pts',(-8.0779015442922,31.1727642891362,-6.71989865898381));
#9659=CARTESIAN_POINT('Ctrl Pts',(-7.83465925602574,31.1898682421531,-7.00197556762376));
#9660=CARTESIAN_POINT('Ctrl Pts',(-7.38137989219953,31.2195167317468,-7.4743572830578));
#9661=CARTESIAN_POINT('Ctrl Pts',(-7.1776665519123,31.2321914486825,-7.67019504977119));
#9662=CARTESIAN_POINT('Ctrl Pts',(-6.47812054187384,31.2741338280966,-8.29039217655118));
#9663=CARTESIAN_POINT('Ctrl Pts',(-5.95067359768883,31.303388653166,-8.67675682070298));
#9664=CARTESIAN_POINT('Ctrl Pts',(-4.98887166047795,31.3545800935956,-9.25210887203168));
#9665=CARTESIAN_POINT('Ctrl Pts',(-4.57130897831263,31.376169227222,-9.4653834087176));
#9666=CARTESIAN_POINT('Ctrl Pts',(-3.79868502152885,31.4148918552883,-9.7969219746833));
#9667=CARTESIAN_POINT('Ctrl Pts',(-3.44887523636577,31.4319707435522,-9.92547051903154));
#9668=CARTESIAN_POINT('Ctrl Pts',(-2.78894922061205,31.4631908145377,-10.1288681297488));
#9669=CARTESIAN_POINT('Ctrl Pts',(-2.48082846589552,31.4774403983092,-10.2087071239348));
#9670=CARTESIAN_POINT('Ctrl Pts',(-1.61221589782715,31.5172671051568,-10.392123979522));
#9671=CARTESIAN_POINT('Ctrl Pts',(-1.04623331237099,31.5428722241993,-10.4642657505441));
#9672=CARTESIAN_POINT('Ctrl Pts',(-0.0184858863972343,31.5898300287755,
-10.51101897649));
#9673=CARTESIAN_POINT('Ctrl Pts',(0.44110533347316,31.6109803849648,-10.5017749605602));
#9674=CARTESIAN_POINT('Ctrl Pts',(1.26933972814084,31.6492792475791,-10.4306392692086));
#9675=CARTESIAN_POINT('Ctrl Pts',(1.63813055474911,31.66637865205,-10.379113803606));
#9676=CARTESIAN_POINT('Ctrl Pts',(2.28070312194509,31.696023293501,-10.254227734207));
#9677=CARTESIAN_POINT('Ctrl Pts',(2.55570528502207,31.7086985765141,-10.1891691013496));
#9678=CARTESIAN_POINT('Ctrl Pts',(3.45607871398569,31.75064201096,-9.93741325689512));
#9679=CARTESIAN_POINT('Ctrl Pts',(4.0666539501315,31.7798973590637,-9.70355424353691));
#9680=CARTESIAN_POINT('Ctrl Pts',(5.07148209200513,31.8310902257058,-9.20708673399526));
#9681=CARTESIAN_POINT('Ctrl Pts',(5.47704407566804,31.8526802623373,-8.97175315950559));
#9682=CARTESIAN_POINT('Ctrl Pts',(6.15308232009437,31.8902184156435,-8.51649927806003));
#9683=CARTESIAN_POINT('Ctrl Pts',(6.43087446562323,31.9061308667628,-8.30873332574524));
#9684=CARTESIAN_POINT('Ctrl Pts',(6.91767933539055,31.9347507915758,-7.90557746905667));
#9685=CARTESIAN_POINT('Ctrl Pts',(7.12996222725988,31.9475542432224,-7.71466684323086));
#9686=CARTESIAN_POINT('Ctrl Pts',(7.80483323400902,31.9898585540256,-7.05606191798188));
#9687=CARTESIAN_POINT('Ctrl Pts',(8.23126914646099,32.019354905531,-6.55359562378533));
#9688=CARTESIAN_POINT('Ctrl Pts',(8.87964062679311,32.0710813188298,-5.62566181671774));
#9689=CARTESIAN_POINT('Ctrl Pts',(9.12470734527588,32.0929602648956,-5.21879242579634));
#9690=CARTESIAN_POINT('Ctrl Pts',(9.50567038337168,32.131361794661,-4.47688803501034));
#9691=CARTESIAN_POINT('Ctrl Pts',(9.65338821463603,32.1478382856922,-4.14878388954857));
#9692=CARTESIAN_POINT('Ctrl Pts',(9.90154503783663,32.1787229375254,-3.51214808074365));
#9693=CARTESIAN_POINT('Ctrl Pts',(10.0050968633687,32.1932183520988,-3.20527982364734));
#9694=CARTESIAN_POINT('Ctrl Pts',(10.2472581585438,32.2326382453562,-2.36065233089806));
#9695=CARTESIAN_POINT('Ctrl Pts',(10.3576746050566,32.2575915458213,-1.81591241339751));
#9696=CARTESIAN_POINT('Ctrl Pts',(10.4795777665442,32.3037695734767,-0.811350842455702));
#9697=CARTESIAN_POINT('Ctrl Pts',(10.5049559575086,32.3248137670466,-0.354584559319434));
#9698=CARTESIAN_POINT('Ctrl Pts',(10.4968081321095,32.3633222300471,0.481156570536684));
#9699=CARTESIAN_POINT('Ctrl Pts',(10.4726219990081,32.3807349184809,0.859475314857011));
#9700=CARTESIAN_POINT('Ctrl Pts',(10.3524566095498,32.4269837209511,1.87357430956689));
#9701=CARTESIAN_POINT('Ctrl Pts',(10.218494273624,32.4555067655601,2.50320456839082));
#9702=CARTESIAN_POINT('Ctrl Pts',(9.8684212966746,32.5087677590744,3.62956853112552));
#9703=CARTESIAN_POINT('Ctrl Pts',(9.66988908326435,32.5332666402691,4.12949488227611));
#9704=CARTESIAN_POINT('Ctrl Pts',(9.17479296395958,32.5851389791878,5.14222437862356));
#9705=CARTESIAN_POINT('Ctrl Pts',(8.87134937579214,32.612432630889,5.6496459768974));
#9706=CARTESIAN_POINT('Ctrl Pts',(8.34676654387113,32.6530835281836,6.37947658030121));
#9707=CARTESIAN_POINT('Ctrl Pts',(8.15569412326338,32.6669120266757,6.62200046351361));
#9708=CARTESIAN_POINT('Ctrl Pts',(7.56363032744996,32.7075935652371,7.30892723128319));
#9709=CARTESIAN_POINT('Ctrl Pts',(7.13503867239633,32.7344713677619,7.7278795958213));
#9710=CARTESIAN_POINT('Ctrl Pts',(6.3141700865968,32.7830185034957,8.40347411311074));
#9711=CARTESIAN_POINT('Ctrl Pts',(5.93600229268122,32.8044417796721,8.6747327087716));
#9712=CARTESIAN_POINT('Ctrl Pts',(5.23817701280554,32.8422829902838,9.10822087290215));
#9713=CARTESIAN_POINT('Ctrl Pts',(4.925840367004,32.8586591790379,9.28085650042046));
#9714=CARTESIAN_POINT('Ctrl Pts',(4.34907050639899,32.8877191716683,9.56231593541395));
#9715=CARTESIAN_POINT('Ctrl Pts',(4.08783385110028,32.9005116248716,9.6768754295446));
#9716=CARTESIAN_POINT('Ctrl Pts',(3.21039784566193,32.9427746911704,10.0197751212775));
#9717=CARTESIAN_POINT('Ctrl Pts',(2.57746250091129,32.9722400284041,10.2009416604426));
#9718=CARTESIAN_POINT('Ctrl Pts',(1.46610156997011,33.0239024017958,10.4089379546954));
#9719=CARTESIAN_POINT('Ctrl Pts',(0.995073406961301,33.0457489264139,10.4644761951211));
#9720=CARTESIAN_POINT('Ctrl Pts',(0.161400278282493,33.0841841243111,10.505962333541));
#9721=CARTESIAN_POINT('Ctrl Pts',(-0.199811410660965,33.1007256701809,10.5053027578804));
#9722=CARTESIAN_POINT('Ctrl Pts',(-0.882888888169412,33.1316454499507,10.4688051310715));
#9723=CARTESIAN_POINT('Ctrl Pts',(-1.20453184458581,33.1461132205511,10.4366891497265));
#9724=CARTESIAN_POINT('Ctrl Pts',(-2.07398367875824,33.1855374088523,10.309140500572));
#9725=CARTESIAN_POINT('Ctrl Pts',(-2.61650358109148,33.2105223051167,10.1849731014887));
#9726=CARTESIAN_POINT('Ctrl Pts',(-3.58249896810754,33.256726705187,9.88156959161748));
#9727=CARTESIAN_POINT('Ctrl Pts',(-4.00895679594617,33.2777643661218,9.7163764531419));
#9728=CARTESIAN_POINT('Ctrl Pts',(-4.76723691466898,33.316286372409,9.36420141374558));
#9729=CARTESIAN_POINT('Ctrl Pts',(-5.10228556222887,33.333718992615,9.18594114613759));
#9730=CARTESIAN_POINT('Ctrl Pts',(-5.97535648448704,33.3799056759568,8.65889387582258));
#9731=CARTESIAN_POINT('Ctrl Pts',(-6.4923125805193,33.408349982469,8.27835885360256));
#9732=CARTESIAN_POINT('Ctrl Pts',(-7.37171386237732,33.4614452932092,7.4976942647904));
#9733=CARTESIAN_POINT('Ctrl Pts',(-7.74428822663554,33.4858591201902,7.11221209581097));
#9734=CARTESIAN_POINT('Ctrl Pts',(-8.46914763228307,33.5381329977369,6.23742406866072));
#9735=CARTESIAN_POINT('Ctrl Pts',(-8.81206575181795,33.5659164259542,5.74277481701839));
#9736=CARTESIAN_POINT('Ctrl Pts',(-9.2689969616897,33.6074613392789,4.94549340146927));
#9737=CARTESIAN_POINT('Ctrl Pts',(-9.41456188314599,33.6217110837854,4.66242832467283));
#9738=CARTESIAN_POINT('Ctrl Pts',(-9.78427601634383,33.6615377487643,3.8553104295076));
#9739=CARTESIAN_POINT('Ctrl Pts',(-9.97896367270501,33.6871426677592,3.31899693066528));
#9740=CARTESIAN_POINT('Ctrl Pts',(-10.2503031528505,33.7341002981444,2.32661719717631));
#9741=CARTESIAN_POINT('Ctrl Pts',(-10.3422270835954,33.7552506886358,1.87621716340056));
#9742=CARTESIAN_POINT('Ctrl Pts',(-10.4547369383482,33.7935494866052,1.05258391474129));
#9743=CARTESIAN_POINT('Ctrl Pts',(-10.4854686962397,33.8106487929695,0.681483470410139));
#9744=CARTESIAN_POINT('Ctrl Pts',(-10.5047634388197,33.8402933514364,0.0271736341898603));
#9745=CARTESIAN_POINT('Ctrl Pts',(-10.5016934800972,33.8529686466748,-0.255402988241976));
#9746=CARTESIAN_POINT('Ctrl Pts',(-10.4538383790911,33.894912103948,-1.18908610520262));
#9747=CARTESIAN_POINT('Ctrl Pts',(-10.3597932795764,33.9241674633898,-1.83611623213397));
#9748=CARTESIAN_POINT('Ctrl Pts',(-10.1077088029461,33.973114734744,-2.87766610130898));
#9749=CARTESIAN_POINT('Ctrl Pts',(-9.98479584838443,33.9924154610121,-3.27879705254936));
#9750=CARTESIAN_POINT('Ctrl Pts',(-9.83826088462892,34.0117278664922,-3.67146071284722));
#9751=CARTESIAN_POINT('Origin',(0.,20.,0.));
#9752=CARTESIAN_POINT('',(-9.83826089695936,37.8294631792708,-3.67146067980585));
#9753=CARTESIAN_POINT('',(-9.83826083089393,37.0111767992967,-3.67146085683862));
#9754=CARTESIAN_POINT('',(-9.83826089695937,20.,-3.67146067980583));
#9755=CARTESIAN_POINT('',(-10.5009999970343,37.6589303301852,0.000249570010058437));
#9756=CARTESIAN_POINT('Ctrl Pts',(-10.5009999970343,37.6589303301852,0.000249570010072427));
#9757=CARTESIAN_POINT('Ctrl Pts',(-10.5010060172308,37.6704494325525,-0.253058443389185));
#9758=CARTESIAN_POINT('Ctrl Pts',(-10.4918421461636,37.6819685349198,-0.506402163384309));
#9759=CARTESIAN_POINT('Ctrl Pts',(-10.4735267137384,37.6934876372871,-0.759104193512294));
#9760=CARTESIAN_POINT('Ctrl Pts',(-10.4552121477138,37.7050061947502,-1.01179426972174));
#9761=CARTESIAN_POINT('Ctrl Pts',(-10.4277469013743,37.7165247522132,-1.26384243591084));
#9762=CARTESIAN_POINT('Ctrl Pts',(-10.39120133153,37.7280433096763,-1.51457449061109));
#9763=CARTESIAN_POINT('Ctrl Pts',(-10.3546588348145,37.7395608985401,-1.76528546117186));
#9764=CARTESIAN_POINT('Ctrl Pts',(-10.3090375811287,37.751078487404,-2.014680263077));
#9765=CARTESIAN_POINT('Ctrl Pts',(-10.2544595205487,37.7625960762678,-2.26209216024217));
#9766=CARTESIAN_POINT('Ctrl Pts',(-10.1998725596876,37.7741155433548,-2.50954440393833));
#9767=CARTESIAN_POINT('Ctrl Pts',(-10.1363259314528,37.7856350104418,-2.75501282140218));
#9768=CARTESIAN_POINT('Ctrl Pts',(-10.0639925248397,37.7971544775288,-2.99784180035765));
#9769=CARTESIAN_POINT('Ctrl Pts',(-9.99636791331339,37.8079240447762,-3.22486298099979));
#9770=CARTESIAN_POINT('Ctrl Pts',(-9.92106382279401,37.8186936120235,-3.44957711398867));
#9771=CARTESIAN_POINT('Ctrl Pts',(-9.83826089695936,37.8294631792708,-3.67146067980586));
#9772=CARTESIAN_POINT('Ctrl Pts',(-10.5009999972296,37.6587489740896,0.000241215157813779));
#9773=CARTESIAN_POINT('Ctrl Pts',(-10.5009931671448,37.6450509232821,0.297580407341688));
#9774=CARTESIAN_POINT('Ctrl Pts',(-10.4883574507233,37.6313755496597,0.594788982950907));
#9775=CARTESIAN_POINT('Ctrl Pts',(-10.4177560221554,37.5935121766817,1.42381184909578));
#9776=CARTESIAN_POINT('Ctrl Pts',(-10.3317628358919,37.5696958577354,1.95232579157638));
#9777=CARTESIAN_POINT('Ctrl Pts',(-10.0830089073701,37.5222180834809,2.97933311726381));
#9778=CARTESIAN_POINT('Ctrl Pts',(-9.92246895061352,37.4986285760186,3.47679235254345));
#9779=CARTESIAN_POINT('Ctrl Pts',(-9.48366771275629,37.445376966917,4.55440652484981));
#9780=CARTESIAN_POINT('Ctrl Pts',(-9.18778777907868,37.4156408468801,5.12514538123641));
#9781=CARTESIAN_POINT('Ctrl Pts',(-8.64388992816215,37.3696030268651,5.97399188297625));
#9782=CARTESIAN_POINT('Ctrl Pts',(-8.43007051008348,37.3531237094165,6.27210706359289));
#9783=CARTESIAN_POINT('Ctrl Pts',(-7.91428582619626,37.3160624723504,6.91707765044198));
#9784=CARTESIAN_POINT('Ctrl Pts',(-7.6042648243848,37.2955066648173,7.25651669786153));
#9785=CARTESIAN_POINT('Ctrl Pts',(-6.86216294971548,37.2489348923546,7.96907545431884));
#9786=CARTESIAN_POINT('Ctrl Pts',(-6.41989159324911,37.2228467037766,8.32949030318713));
#9787=CARTESIAN_POINT('Ctrl Pts',(-5.68843780410364,37.1819424163878,8.83254825725357));
#9788=CARTESIAN_POINT('Ctrl Pts',(-5.41822249890715,37.1672686695633,9.0008388875092));
#9789=CARTESIAN_POINT('Ctrl Pts',(-4.61698912534079,37.1252235735471,9.45067465024983));
#9790=CARTESIAN_POINT('Ctrl Pts',(-4.06893898855017,37.0984585533248,9.69925685163864));
#9791=CARTESIAN_POINT('Ctrl Pts',(-2.99791507425247,37.0474310088776,10.0782011499541));
#9792=CARTESIAN_POINT('Ctrl Pts',(-2.48028825814185,37.0232531232271,10.2179148112985));
#9793=CARTESIAN_POINT('Ctrl Pts',(-1.3247524020341,36.9694343513984,10.4367885293251));
#9794=CARTESIAN_POINT('Ctrl Pts',(-0.685640791880849,36.939738817857,10.4981620912132));
#9795=CARTESIAN_POINT('Ctrl Pts',(0.335063923662304,36.8931136972875,10.5025299849476));
#9796=CARTESIAN_POINT('Ctrl Pts',(0.714866487983967,36.8760381714026,10.4835286885906));
#9797=CARTESIAN_POINT('Ctrl Pts',(1.54694157984521,36.8384971023869,10.3964640262963));
#9798=CARTESIAN_POINT('Ctrl Pts',(1.99748379721537,36.8180526336035,10.3193771823113));
#9799=CARTESIAN_POINT('Ctrl Pts',(2.98332707116183,36.7721575552213,10.0837012783703));
#9800=CARTESIAN_POINT('Ctrl Pts',(3.51390673322399,36.746646284169,9.91129184004001));
#9801=CARTESIAN_POINT('Ctrl Pts',(4.32559075883288,36.7061501330183,9.5741268055798));
#9802=CARTESIAN_POINT('Ctrl Pts',(4.61705629253519,36.6913012439449,9.43702458443572));
#9803=CARTESIAN_POINT('Ctrl Pts',(5.22340538795978,36.6599241217061,9.11697935372812));
#9804=CARTESIAN_POINT('Ctrl Pts',(5.53600520905962,36.6435290477408,8.9306173899538));
#9805=CARTESIAN_POINT('Ctrl Pts',(6.23101235461873,36.605982894881,8.46573646258003));
#9806=CARTESIAN_POINT('Ctrl Pts',(6.6055336342901,36.5848593384056,8.17686556556475));
#9807=CARTESIAN_POINT('Ctrl Pts',(7.45036901534075,36.5338405387999,7.42919717806922));
#9808=CARTESIAN_POINT('Ctrl Pts',(7.8996172681901,36.5037756079646,6.94960252920526));
#9809=CARTESIAN_POINT('Ctrl Pts',(8.47548669597734,36.460445537834,6.20629675579876));
#9810=CARTESIAN_POINT('Ctrl Pts',(8.64056751757498,36.4473377495159,5.97432755210562));
#9811=CARTESIAN_POINT('Ctrl Pts',(8.99222503301976,36.4179250758232,5.43506312840404));
#9812=CARTESIAN_POINT('Ctrl Pts',(9.17285809141486,36.4017657998048,5.12432436372973));
#9813=CARTESIAN_POINT('Ctrl Pts',(9.54947404862761,36.3648216195109,4.39246296582987));
#9814=CARTESIAN_POINT('Ctrl Pts',(9.73416502573225,36.3440663805361,3.96638526046115));
#9815=CARTESIAN_POINT('Ctrl Pts',(10.0914118035039,36.295970740073,2.96533666616792));
#9816=CARTESIAN_POINT('Ctrl Pts',(10.2440998739793,36.2685274735933,2.3849947684543));
#9817=CARTESIAN_POINT('Ctrl Pts',(10.3989541809779,36.2267776026196,1.49231921162564));
#9818=CARTESIAN_POINT('Ctrl Pts',(10.4381388239824,36.212623356528,1.18765527177303));
#9819=CARTESIAN_POINT('Ctrl Pts',(10.5131583355003,36.1717595586685,0.297343632478159));
#9820=CARTESIAN_POINT('Ctrl Pts',(10.513360776764,36.1456246276376,-0.290111434756389));
#9821=CARTESIAN_POINT('Ctrl Pts',(10.4196825005028,36.0951066353059,-1.41106751099651));
#9822=CARTESIAN_POINT('Ctrl Pts',(10.333645272681,36.0707979122,-1.94336046620219));
#9823=CARTESIAN_POINT('Ctrl Pts',(10.0568119201155,36.0168739070513,-3.08889598606517));
#9824=CARTESIAN_POINT('Ctrl Pts',(9.84987484321755,35.9872087190027,-3.69603793676894));
#9825=CARTESIAN_POINT('Ctrl Pts',(9.44458832182835,35.9417823433404,-4.60392992676662));
#9826=CARTESIAN_POINT('Ctrl Pts',(9.28396371067778,35.9258453826508,-4.91980086565283));
#9827=CARTESIAN_POINT('Ctrl Pts',(8.87578105869489,35.8890342822107,-5.63103608956011));
#9828=CARTESIAN_POINT('Ctrl Pts',(8.6172471334104,35.8681926938872,-6.01922787277115));
#9829=CARTESIAN_POINT('Ctrl Pts',(7.93718123420258,35.8176213233452,-6.90630879524323));
#9830=CARTESIAN_POINT('Ctrl Pts',(7.49326434197177,35.7877175010241,-7.38558709812607));
#9831=CARTESIAN_POINT('Ctrl Pts',(6.7990631115209,35.74476429676,-8.00764005631805));
#9832=CARTESIAN_POINT('Ctrl Pts',(6.58291778086649,35.7318578329585,-8.18625399876423));
#9833=CARTESIAN_POINT('Ctrl Pts',(6.08774374670913,35.7034345248684,-8.56313850062324));
#9834=CARTESIAN_POINT('Ctrl Pts',(5.80565073700636,35.6880405800981,-8.75684803972511));
#9835=CARTESIAN_POINT('Ctrl Pts',(5.11595898167302,35.6516562161267,-9.18245043650225));
#9836=CARTESIAN_POINT('Ctrl Pts',(4.7013057683148,35.6307053974818,-9.40149733726477));
#9837=CARTESIAN_POINT('Ctrl Pts',(3.6773831583457,35.5799996353671,-9.8576683107361));
#9838=CARTESIAN_POINT('Ctrl Pts',(3.05790661175083,35.5500736248345,-10.0670719907663));
#9839=CARTESIAN_POINT('Ctrl Pts',(2.14816247853522,35.5069886249336,-10.2828110046282));
#9840=CARTESIAN_POINT('Ctrl Pts',(1.87077042196794,35.4939788034298,-10.3368769361586));
#9841=CARTESIAN_POINT('Ctrl Pts',(1.22388011677837,35.4640826408215,-10.4360656513436));
#9842=CARTESIAN_POINT('Ctrl Pts',(0.853495917054556,35.4473616985031,-10.4728648086759));
#9843=CARTESIAN_POINT('Ctrl Pts',(0.0231684158759233,35.4100599734809,-10.5110119369182));
#9844=CARTESIAN_POINT('Ctrl Pts',(-0.436478849810725,35.3895029968399,-10.5019707519977));
#9845=CARTESIAN_POINT('Ctrl Pts',(-1.46130585503684,35.3429427133106,-10.4143992646476));
#9846=CARTESIAN_POINT('Ctrl Pts',(-2.02366631855655,35.3168675595913,-10.3198776322952));
#9847=CARTESIAN_POINT('Ctrl Pts',(-2.88423401563315,35.2759662593278,-10.1021564200989));
#9848=CARTESIAN_POINT('Ctrl Pts',(-3.18918480192251,35.2612824842756,-10.0100685736161));
#9849=CARTESIAN_POINT('Ctrl Pts',(-4.05388845964617,35.2193317474278,-9.70541537184412));
#9850=CARTESIAN_POINT('Ctrl Pts',(-4.60025503841201,35.1926655424663,-9.4586870525714));
#9851=CARTESIAN_POINT('Ctrl Pts',(-5.59105010693511,35.1416887258416,-8.90500339111274));
#9852=CARTESIAN_POINT('Ctrl Pts',(-6.03869717872041,35.1174588941208,-8.6077315681033));
#9853=CARTESIAN_POINT('Ctrl Pts',(-6.96717991364704,35.063560127356,-7.88293660805527));
#9854=CARTESIAN_POINT('Ctrl Pts',(-7.4354860049986,35.0338372604638,-7.44283682841304));
#9855=CARTESIAN_POINT('Ctrl Pts',(-8.10849382247395,34.9874710629029,-6.68303683256363));
#9856=CARTESIAN_POINT('Ctrl Pts',(-8.34116654542886,34.970673078064,-6.39027369024781));
#9857=CARTESIAN_POINT('Ctrl Pts',(-8.82355171872713,34.9333201812836,-5.71194377016188));
#9858=CARTESIAN_POINT('Ctrl Pts',(-9.06458373155467,34.9127884207058,-5.32115429414048));
#9859=CARTESIAN_POINT('Ctrl Pts',(-9.49243924227483,34.8714136217851,-4.51352483129694));
#9860=CARTESIAN_POINT('Ctrl Pts',(-9.67914359682593,34.8506211757911,-4.09784071169662));
#9861=CARTESIAN_POINT('Ctrl Pts',(-9.83826090449496,34.8296849384879,-3.671460659613));
#9862=CARTESIAN_POINT('Ctrl Pts',(-9.83826088462892,34.0117278664922,-3.67146071284722));
#9863=CARTESIAN_POINT('Ctrl Pts',(-9.82107553834802,34.01399278926,-3.71751157198144));
#9864=CARTESIAN_POINT('Ctrl Pts',(-9.80356528834997,34.0162576204145,-3.76344598199641));
#9865=CARTESIAN_POINT('Ctrl Pts',(-9.65997591879196,34.0344885301241,-4.13231731106991));
#9866=CARTESIAN_POINT('Ctrl Pts',(-9.51829653611892,34.0504009223036,-4.44895786013873));
#9867=CARTESIAN_POINT('Ctrl Pts',(-9.23190495344731,34.0790207844127,-5.01242190650544));
#9868=CARTESIAN_POINT('Ctrl Pts',(-9.09228079640018,34.0918242307828,-5.26145186382657));
#9869=CARTESIAN_POINT('Ctrl Pts',(-8.59798323113089,34.1341285213107,-6.06449631212284));
#9870=CARTESIAN_POINT('Ctrl Pts',(-8.20144663832499,34.1636248574456,-6.5908785424878));
#9871=CARTESIAN_POINT('Ctrl Pts',(-7.43857670499025,34.2153512391263,-7.42722457068528));
#9872=CARTESIAN_POINT('Ctrl Pts',(-7.09546775876342,34.2372301692476,-7.75566989286965));
#9873=CARTESIAN_POINT('Ctrl Pts',(-6.4553518203272,34.2756317152955,-8.2902792038028));
#9874=CARTESIAN_POINT('Ctrl Pts',(-6.16770279300873,34.2921082380427,-8.50645369867616));
#9875=CARTESIAN_POINT('Ctrl Pts',(-5.60111594826016,34.3229929066519,-8.88837882906752));
#9876=CARTESIAN_POINT('Ctrl Pts',(-5.32448466339852,34.3374883074028,-9.0568010279565));
#9877=CARTESIAN_POINT('Ctrl Pts',(-4.55366832272441,34.376908202781,-9.47855919454229));
#9878=CARTESIAN_POINT('Ctrl Pts',(-4.04648081827942,34.4018615190202,-9.70592368130221));
#9879=CARTESIAN_POINT('Ctrl Pts',(-3.09322247052688,34.4480395598217,-10.0454872972977));
#9880=CARTESIAN_POINT('Ctrl Pts',(-2.65318347112359,34.46908375011,-10.1705676972919));
#9881=CARTESIAN_POINT('Ctrl Pts',(-1.83605970106974,34.5075922198815,-10.3461769530387));
#9882=CARTESIAN_POINT('Ctrl Pts',(-1.46166637200327,34.5250049182953,-10.4056734971707));
#9883=CARTESIAN_POINT('Ctrl Pts',(-0.447842327974835,34.5711669666702,-10.5109760815768));
#9884=CARTESIAN_POINT('Ctrl Pts',(0.193906747451343,34.5996062622448,-10.5187261956888));
#9885=CARTESIAN_POINT('Ctrl Pts',(1.36593990272974,34.6526930442481,-10.4255319750211));
#9886=CARTESIAN_POINT('Ctrl Pts',(1.89548321630696,34.677103510136,-10.3423705523182));
#9887=CARTESIAN_POINT('Ctrl Pts',(3.00113641060863,34.7293801120193,-10.0809355232661));
#9888=CARTESIAN_POINT('Ctrl Pts',(3.57298191992697,34.75716983612,-9.89272084778132));
#9889=CARTESIAN_POINT('Ctrl Pts',(4.41813422754015,34.7987200223659,-9.53164668932002));
#9890=CARTESIAN_POINT('Ctrl Pts',(4.70484309408987,34.8129690032317,-9.39343674045633));
#9891=CARTESIAN_POINT('Ctrl Pts',(5.48621139839481,34.8527958671224,-8.97201120350292));
#9892=CARTESIAN_POINT('Ctrl Pts',(5.96474156420531,34.8784017365229,-8.66125507940379));
#9893=CARTESIAN_POINT('Ctrl Pts',(6.77922211186451,34.925360194481,-8.03268365815304));
#9894=CARTESIAN_POINT('Ctrl Pts',(7.12395001650136,34.9465104220155,-7.7285952760906));
#9895=CARTESIAN_POINT('Ctrl Pts',(7.70998674334918,34.9848095270804,-7.13901738239864));
#9896=CARTESIAN_POINT('Ctrl Pts',(7.95810712087114,35.001909299506,-6.86134184945294));
#9897=CARTESIAN_POINT('Ctrl Pts',(8.36772949891579,35.0315542520744,-6.35073976792056));
#9898=CARTESIAN_POINT('Ctrl Pts',(8.53552910504756,35.0442294891182,-6.12336008969783));
#9899=CARTESIAN_POINT('Ctrl Pts',(9.05987166239957,35.086172837601,-5.34933515696538));
#9900=CARTESIAN_POINT('Ctrl Pts',(9.37464318187299,35.1154281429425,-4.77626458284983));
#9901=CARTESIAN_POINT('Ctrl Pts',(9.82053445804387,35.1666208932384,-3.74799656513446));
#9902=CARTESIAN_POINT('Ctrl Pts',(9.97791192030554,35.1882108563075,-3.30630289440341));
#9903=CARTESIAN_POINT('Ctrl Pts',(10.1995496528347,35.2257491612139,-2.52197783212394));
#9904=CARTESIAN_POINT('Ctrl Pts',(10.2772472934879,35.2416618343669,-2.18389268400027));
#9905=CARTESIAN_POINT('Ctrl Pts',(10.3881555855434,35.2702819956406,-1.56162296899322));
#9906=CARTESIAN_POINT('Ctrl Pts',(10.4267570454005,35.283085467408,-1.2787429923918));
#9907=CARTESIAN_POINT('Ctrl Pts',(10.5160749685079,35.325389855962,-0.340000797934821));
#9908=CARTESIAN_POINT('Ctrl Pts',(10.5167309121742,35.3548862665161,0.319029727509173));
#9909=CARTESIAN_POINT('Ctrl Pts',(10.4117576583452,35.4066128012676,1.44616465904065));
#9910=CARTESIAN_POINT('Ctrl Pts',(10.3357994845268,35.4284918085721,1.91502709021752));
#9911=CARTESIAN_POINT('Ctrl Pts',(10.1470053802454,35.466893275827,2.72737526988958));
#9912=CARTESIAN_POINT('Ctrl Pts',(10.0476700661485,35.4833696450731,3.07321267737527));
#9913=CARTESIAN_POINT('Ctrl Pts',(9.82557113631646,35.5142542319246,3.71939926495458));
#9914=CARTESIAN_POINT('Ctrl Pts',(9.70625756771215,35.5287496990205,4.02049086457001));
#9915=CARTESIAN_POINT('Ctrl Pts',(9.34515643256911,35.5681695839986,4.82151728307303));
#9916=CARTESIAN_POINT('Ctrl Pts',(9.077344045512,35.5931228243038,5.30855768187026));
#9917=CARTESIAN_POINT('Ctrl Pts',(8.52111097531407,35.6393008014113,6.15390187850402));
#9918=CARTESIAN_POINT('Ctrl Pts',(8.24526505777467,35.6603450070749,6.51885221762408));
#9919=CARTESIAN_POINT('Ctrl Pts',(7.69890254694489,35.6988534447153,7.15132096731503));
#9920=CARTESIAN_POINT('Ctrl Pts',(7.43593714038595,35.7162660959639,7.42437523245819));
#9921=CARTESIAN_POINT('Ctrl Pts',(6.95270705750426,35.7461795903885,7.87465608880977));
#9922=CARTESIAN_POINT('Ctrl Pts',(6.73898304516037,35.7588197397611,8.05831587719436));
#9923=CARTESIAN_POINT('Ctrl Pts',(6.00699561721915,35.8007055181527,8.63782479840948));
#9924=CARTESIAN_POINT('Ctrl Pts',(5.45929559545112,35.829936257828,8.99400258021143));
#9925=CARTESIAN_POINT('Ctrl Pts',(4.46839230002774,35.8810536570763,9.51434949451566));
#9926=CARTESIAN_POINT('Ctrl Pts',(4.04062426561489,35.9025926050085,9.70374780135818));
#9927=CARTESIAN_POINT('Ctrl Pts',(3.24974289814775,35.9413721257924,9.99252423901558));
#9928=CARTESIAN_POINT('Ctrl Pts',(2.8911756253112,35.9585568610987,10.1021032799281));
#9929=CARTESIAN_POINT('Ctrl Pts',(2.21977424548672,35.9898315369082,10.2685991161173));
#9930=CARTESIAN_POINT('Ctrl Pts',(1.90873810723697,36.0040336957253,10.3309364538006));
#9931=CARTESIAN_POINT('Ctrl Pts',(1.02984421106209,36.0439251099452,10.4660299115486));
#9932=CARTESIAN_POINT('Ctrl Pts',(0.458184335963544,36.0696419646578,10.5065888423917));
#9933=CARTESIAN_POINT('Ctrl Pts',(-0.573387406794513,36.1167298271369,10.4953972652735));
#9934=CARTESIAN_POINT('Ctrl Pts',(-1.032028171556,36.1378945809863,10.4602602415402));
#9935=CARTESIAN_POINT('Ctrl Pts',(-1.85436440864884,36.1761664768795,10.3426369619515));
#9936=CARTESIAN_POINT('Ctrl Pts',(-2.21881118676237,36.1932248717734,10.2706231398251));
#9937=CARTESIAN_POINT('Ctrl Pts',(-2.85262671330958,36.2228348974054,10.1100633213754));
#9938=CARTESIAN_POINT('Ctrl Pts',(-3.12365628849769,36.2355153632179,10.029637792301));
#9939=CARTESIAN_POINT('Ctrl Pts',(-4.0086830890575,36.2774686554225,9.72765425242399));
#9940=CARTESIAN_POINT('Ctrl Pts',(-4.60525566416108,36.3067289912895,9.45983057912808));
#9941=CARTESIAN_POINT('Ctrl Pts',(-5.58085013884738,36.3579352482258,8.90756157266984));
#9942=CARTESIAN_POINT('Ctrl Pts',(-5.97269230029302,36.3795336797535,8.6497097037301));
#9943=CARTESIAN_POINT('Ctrl Pts',(-6.61826543378769,36.4168520082205,8.16004546041644));
#9944=CARTESIAN_POINT('Ctrl Pts',(-6.8802984990199,36.4325393661667,7.94035799165896));
#9945=CARTESIAN_POINT('Ctrl Pts',(-7.33695081661843,36.4607156866972,7.51789532230048));
#9946=CARTESIAN_POINT('Ctrl Pts',(-7.53503811670473,36.4732972265957,7.31934431775822));
#9947=CARTESIAN_POINT('Ctrl Pts',(-8.16646712116347,36.5151189574526,6.63360230140625));
#9948=CARTESIAN_POINT('Ctrl Pts',(-8.56237840794939,36.5443408813799,6.11404270893559));
#9949=CARTESIAN_POINT('Ctrl Pts',(-9.15431016417877,36.5953852458462,5.16591720935694));
#9950=CARTESIAN_POINT('Ctrl Pts',(-9.37447975952864,36.6168585856071,4.75470442785361));
#9951=CARTESIAN_POINT('Ctrl Pts',(-9.71260358222404,36.6546272696711,4.00770226716491));
#9952=CARTESIAN_POINT('Ctrl Pts',(-9.84219671917791,36.6708823428343,3.67797826849634));
#9953=CARTESIAN_POINT('Ctrl Pts',(-10.158797385242,36.7159212325916,2.73500596547848));
#9954=CARTESIAN_POINT('Ctrl Pts',(-10.3067023173824,36.744370277336,2.11029105045309));
#9955=CARTESIAN_POINT('Ctrl Pts',(-10.4725128634216,36.7976415472326,0.942339456098136));
#9956=CARTESIAN_POINT('Ctrl Pts',(-10.5070723079455,36.8222295342717,0.403654384983058));
#9957=CARTESIAN_POINT('Ctrl Pts',(-10.4925952456766,36.8739423694035,-0.719977388160804));
#9958=CARTESIAN_POINT('Ctrl Pts',(-10.4362377743516,36.9009827940751,-1.30303665011896));
#9959=CARTESIAN_POINT('Ctrl Pts',(-10.2768407726382,36.9412896196935,-2.1797661302418));
#9960=CARTESIAN_POINT('Ctrl Pts',(-10.2088843604856,36.9550178146084,-2.47861258304013));
#9961=CARTESIAN_POINT('Ctrl Pts',(-10.0448419571441,36.9828740075259,-3.07752305632839));
#9962=CARTESIAN_POINT('Ctrl Pts',(-9.94816557881936,36.9969829310156,-3.37695367868638));
#9963=CARTESIAN_POINT('Ctrl Pts',(-9.83826083089393,37.0111767992967,-3.67146085683862));
#9964=CARTESIAN_POINT('Origin',(0.,20.,0.));
#9965=CARTESIAN_POINT('',(-9.92805791774766,39.9999999999999,-3.42120840958979));
#9966=CARTESIAN_POINT('Ctrl Pts',(-9.83826083089393,37.0111767992967,-3.67146085683862));
#9967=CARTESIAN_POINT('Ctrl Pts',(-9.73905989430054,37.0239883024752,-3.93728547731821));
#9968=CARTESIAN_POINT('Ctrl Pts',(-9.62908183107698,37.0368682888152,-4.19909901233635));
#9969=CARTESIAN_POINT('Ctrl Pts',(-9.31204345078195,37.0709788240597,-4.8755833547218));
#9970=CARTESIAN_POINT('Ctrl Pts',(-9.08799623536165,37.0923167188737,-5.28145627578774));
#9971=CARTESIAN_POINT('Ctrl Pts',(-8.64281680448154,37.1302894779228,-5.97521515508012));
#9972=CARTESIAN_POINT('Ctrl Pts',(-8.43217506162394,37.146880163272,-6.26896461977247));
#9973=CARTESIAN_POINT('Ctrl Pts',(-8.02950610498512,37.1761071144259,-6.773389170174));
#9974=CARTESIAN_POINT('Ctrl Pts',(-7.84325783494508,37.1888583955273,-6.98821000109359));
#9975=CARTESIAN_POINT('Ctrl Pts',(-7.19985813159442,37.2309848555009,-7.67214501608539));
#9976=CARTESIAN_POINT('Ctrl Pts',(-6.70757534334714,37.2603519889738,-8.10605795831986));
#9977=CARTESIAN_POINT('Ctrl Pts',(-5.79684588091793,37.3118068234315,-8.76868790868151));
#9978=CARTESIAN_POINT('Ctrl Pts',(-5.3973391202167,37.3335457799443,-9.02009036176285));
#9979=CARTESIAN_POINT('Ctrl Pts',(-4.6603466040634,37.3721009978974,-9.41732115860841));
#9980=CARTESIAN_POINT('Ctrl Pts',(-4.32953661791407,37.3888667626374,-9.57391756462574));
#9981=CARTESIAN_POINT('Ctrl Pts',(-3.69418348777181,37.4199177555993,-9.83499562536363));
#9982=CARTESIAN_POINT('Ctrl Pts',(-3.391700343897,37.4343002646923,-9.94336477591121));
#9983=CARTESIAN_POINT('Ctrl Pts',(-2.55140399884652,37.4737382637981,-10.2015995051287));
#9984=CARTESIAN_POINT('Ctrl Pts',(-2.00587894423726,37.4988211085439,-10.322728629309));
#9985=CARTESIAN_POINT('Ctrl Pts',(-1.00127896734655,37.5451076147441,-10.4631151954579));
#9986=CARTESIAN_POINT('Ctrl Pts',(-0.545597948904389,37.5661253639356,-10.4967448073524));
#9987=CARTESIAN_POINT('Ctrl Pts',(0.291343322489434,37.6046892413099,-10.5038532182323));
#9988=CARTESIAN_POINT('Ctrl Pts',(0.671777392509451,37.6221832103093,-10.4863981134722));
#9989=CARTESIAN_POINT('Ctrl Pts',(1.68827749329314,37.6684519883671,-10.3842032878484));
#9990=CARTESIAN_POINT('Ctrl Pts',(2.31891574870903,37.6969177537914,-10.261803365034));
#9991=CARTESIAN_POINT('Ctrl Pts',(3.44880206949852,37.7500520728763,-9.93296182153168));
#9992=CARTESIAN_POINT('Ctrl Pts',(3.95093229497363,37.7744828223189,-9.74413037141234));
#9993=CARTESIAN_POINT('Ctrl Pts',(4.98035424853465,37.8267427820846,-9.26429604315755));
#9994=CARTESIAN_POINT('Ctrl Pts',(5.50154477174102,37.8544943192975,-8.96460592972659));
#9995=CARTESIAN_POINT('Ctrl Pts',(6.25555846737383,37.8960118213246,-8.44039357706595));
#9996=CARTESIAN_POINT('Ctrl Pts',(6.50843760648304,37.9102647424265,-8.24696908397847));
#9997=CARTESIAN_POINT('Ctrl Pts',(7.18833163006239,37.9500905056219,-7.6761487026352));
#9998=CARTESIAN_POINT('Ctrl Pts',(7.59399490846076,37.9756913960834,-7.27506651489101));
#9999=CARTESIAN_POINT('Ctrl Pts',(8.26437312698382,38.0226453103723,-6.49476775697042));
#10000=CARTESIAN_POINT('Ctrl Pts',(8.54044653188181,38.0437961782442,-6.12720442133533));
#10001=CARTESIAN_POINT('Ctrl Pts',(8.99504740759032,38.0820942285981,-5.43125770824885));
#10002=CARTESIAN_POINT('Ctrl Pts',(9.18183133665637,38.0991923168503,-5.10915135950574));
#10003=CARTESIAN_POINT('Ctrl Pts',(9.47966242311408,38.1288368754527,-4.52623557170313));
#10004=CARTESIAN_POINT('Ctrl Pts',(9.59799392918533,38.1415133374784,-4.26958124020874));
#10005=CARTESIAN_POINT('Ctrl Pts',(9.95489857914898,38.1834602424146,-3.40539605679225));
#10006=CARTESIAN_POINT('Ctrl Pts',(10.1472103829282,38.2127179562829,-2.78043637764054));
#10007=CARTESIAN_POINT('Ctrl Pts',(10.3758195659338,38.2639163761495,-1.68309454794301));
#10008=CARTESIAN_POINT('Ctrl Pts',(10.440564379196,38.2855095746426,-1.21862389289477));
#10009=CARTESIAN_POINT('Ctrl Pts',(10.4985530174163,38.3228346917503,-0.410288687911039));
#10010=CARTESIAN_POINT('Ctrl Pts',(10.5063464927678,38.3385339041418,-0.0681825709019842));
#10011=CARTESIAN_POINT('Ctrl Pts',(10.4901281404209,38.3667168772567,0.553848274071962));
#10012=CARTESIAN_POINT('Ctrl Pts',(10.4716122148784,38.3792935880818,0.833592965782277));
#10013=CARTESIAN_POINT('Ctrl Pts',(10.3728913525475,38.4211091065636,1.76038397983086));
#10014=CARTESIAN_POINT('Ctrl Pts',(10.2436638455507,38.4503293711814,2.40065726962739));
#10015=CARTESIAN_POINT('Ctrl Pts',(9.92175328152203,38.5013651471385,3.47084560352994));
#10016=CARTESIAN_POINT('Ctrl Pts',(9.7580567830438,38.522831439781,3.90746400638749));
#10017=CARTESIAN_POINT('Ctrl Pts',(9.41973061163887,38.5606096343644,4.65459655315724));
#10018=CARTESIAN_POINT('Ctrl Pts',(9.25728787107139,38.576881052438,4.96983196561479));
#10019=CARTESIAN_POINT('Ctrl Pts',(8.75756552048223,38.6219139102628,5.8297379395082));
#10020=CARTESIAN_POINT('Ctrl Pts',(8.38597842898762,38.6503417503912,6.35265165756233));
#10021=CARTESIAN_POINT('Ctrl Pts',(7.61834100524716,38.7035717469729,7.24720422801135));
#10022=CARTESIAN_POINT('Ctrl Pts',(7.23667634886596,38.7281402557982,7.62834059879137));
#10023=CARTESIAN_POINT('Ctrl Pts',(6.38221701622929,38.7798927307959,8.35952978542744));
#10024=CARTESIAN_POINT('Ctrl Pts',(5.90583190373884,38.8069933455544,8.70262161585597));
#10025=CARTESIAN_POINT('Ctrl Pts',(5.14023112974277,38.8473792103231,9.16204970181207));
#10026=CARTESIAN_POINT('Ctrl Pts',(4.87036283062654,38.8611285463629,9.30831350363304));
#10027=CARTESIAN_POINT('Ctrl Pts',(4.05603717759795,38.9017532074208,9.70454111941243));
#10028=CARTESIAN_POINT('Ctrl Pts',(3.49618632051631,38.9286507952904,9.91999073676913));
#10029=CARTESIAN_POINT('Ctrl Pts',(2.47579919000137,38.9771556318177,10.2154924447661));
#10030=CARTESIAN_POINT('Ctrl Pts',(2.02251223623083,38.9985143726746,10.3148098128499));
#10031=CARTESIAN_POINT('Ctrl Pts',(1.20823159854175,39.0364477633893,10.4374678467502));
#10032=CARTESIAN_POINT('Ctrl Pts',(0.849774263710614,39.05297889355,10.4727483234094));
#10033=CARTESIAN_POINT('Ctrl Pts',(-0.150557562894974,39.0983254819715,
10.5194964790874));
#10034=CARTESIAN_POINT('Ctrl Pts',(-0.792721234902023,39.1268098596827,
10.4906666181723));
#10035=CARTESIAN_POINT('Ctrl Pts',(-1.96185848709003,39.1801001668114,10.33016123741));
#10036=CARTESIAN_POINT('Ctrl Pts',(-2.48904105681407,39.2046700212431,10.2159566660736));
#10037=CARTESIAN_POINT('Ctrl Pts',(-3.56660513830276,39.2564220553846,9.89412535282592));
#10038=CARTESIAN_POINT('Ctrl Pts',(-4.11308549598285,39.2835206738592,9.67971888053443));
#10039=CARTESIAN_POINT('Ctrl Pts',(-4.91444035227622,39.3239230545017,9.28513076552596));
#10040=CARTESIAN_POINT('Ctrl Pts',(-5.18396213346218,39.3376903890689,9.13739117525792));
#10041=CARTESIAN_POINT('Ctrl Pts',(-5.9588643346019,39.3783492217483,8.66728915003368));
#10042=CARTESIAN_POINT('Ctrl Pts',(-6.44356352423443,39.4052637002322,8.31326851901633));
#10043=CARTESIAN_POINT('Ctrl Pts',(-7.24559578786201,39.4538217092952,7.61497987927717));
#10044=CARTESIAN_POINT('Ctrl Pts',(-7.57516283688475,39.4752169540367,7.28721308807987));
#10045=CARTESIAN_POINT('Ctrl Pts',(-8.11832879363577,39.5130830508623,6.67021071066468));
#10046=CARTESIAN_POINT('Ctrl Pts',(-8.34083831023809,39.529511718192,6.38978908018728));
#10047=CARTESIAN_POINT('Ctrl Pts',(-8.92008950432261,39.5746764430164,5.57782727539355));
#10048=CARTESIAN_POINT('Ctrl Pts',(-9.24322060555003,39.6030796878232,5.02424581969796));
#10049=CARTESIAN_POINT('Ctrl Pts',(-9.74010614398457,39.6560841395034,3.96065361798012));
#10050=CARTESIAN_POINT('Ctrl Pts',(-9.92896772308112,39.6804485897593,3.46006088302585));
#10051=CARTESIAN_POINT('Ctrl Pts',(-10.2479972573181,39.7327488282212,2.36906749788065));
#10052=CARTESIAN_POINT('Ctrl Pts',(-10.3670148749052,39.7606089961443,1.77735091653152));
#10053=CARTESIAN_POINT('Ctrl Pts',(-10.4707089883898,39.8023742578623,0.859370525804358));
#10054=CARTESIAN_POINT('Ctrl Pts',(-10.4921025603994,39.8167677730611,0.538564742257382));
#10055=CARTESIAN_POINT('Ctrl Pts',(-10.5031253573529,39.8406699778085,0.00595797520689834));
#10056=CARTESIAN_POINT('Ctrl Pts',(-10.5011174646234,39.8501577388957,-0.205448543471378));
#10057=CARTESIAN_POINT('Ctrl Pts',(-10.474427538646,39.8804582490252,-0.877597004694431));
#10058=CARTESIAN_POINT('Ctrl Pts',(-10.4257701944779,39.9013847797024,-1.3368282622233));
#10059=CARTESIAN_POINT('Ctrl Pts',(-10.2512300573561,39.948272470248,-2.34498902998284));
#10060=CARTESIAN_POINT('Ctrl Pts',(-10.111105597097,39.9742790179436,-2.89001950066633));
#10061=CARTESIAN_POINT('Ctrl Pts',(-9.92805791774766,39.9999999999999,-3.42120840958979));
#10062=CARTESIAN_POINT('',(-1.99079507083261,40.,10.3105642903746));
#10063=CARTESIAN_POINT('Origin',(0.,40.,0.));
#10064=CARTESIAN_POINT('Ctrl Pts',(-9.83826089695936,37.8294631792708,-3.67146067980586));
#10065=CARTESIAN_POINT('Ctrl Pts',(-9.77094254382746,37.8382187820919,-3.85185087842846));
#10066=CARTESIAN_POINT('Ctrl Pts',(-9.69866848483662,37.846974384913,-4.03037036327237));
#10067=CARTESIAN_POINT('Ctrl Pts',(-9.62155384401236,37.8557299877341,-4.20674489680216));
#10068=CARTESIAN_POINT('Ctrl Pts',(-9.51967913321628,37.8672968509875,-4.43974999678165));
#10069=CARTESIAN_POINT('Ctrl Pts',(-9.40932061872495,37.8788637142408,-4.66908884410418));
#10070=CARTESIAN_POINT('Ctrl Pts',(-9.29076776060943,37.8904305774941,-4.89414297077848));
#10071=CARTESIAN_POINT('Ctrl Pts',(-9.17223566898852,37.90199541462,-5.1191576754989));
#10072=CARTESIAN_POINT('Ctrl Pts',(-9.04551222811113,37.9135602517459,-5.33988891303509));
#10073=CARTESIAN_POINT('Ctrl Pts',(-8.91093325131949,37.9251250888717,-5.55574203779555));
#10074=CARTESIAN_POINT('Ctrl Pts',(-8.77636931441923,37.9366886335677,-5.77157103986145));
#10075=CARTESIAN_POINT('Ctrl Pts',(-8.63395174090342,37.9482521782636,-5.98252278281403));
#10076=CARTESIAN_POINT('Ctrl Pts',(-8.48406072464668,37.9598157229596,-6.18802994663953));
#10077=CARTESIAN_POINT('Ctrl Pts',(-8.33415787571415,37.9713801805033,-6.39355333358303));
#10078=CARTESIAN_POINT('Ctrl Pts',(-8.17678056561697,37.982944638047,-6.5936310568969));
#10079=CARTESIAN_POINT('Ctrl Pts',(-8.01235129321971,37.9945090955907,-6.78772625803666));
#10080=CARTESIAN_POINT('Ctrl Pts',(-7.84792499971485,38.0060733436262,-6.98181794283954));
#10081=CARTESIAN_POINT('Ctrl Pts',(-7.67644717980999,38.0176375916618,-7.16992711216884));
#10082=CARTESIAN_POINT('Ctrl Pts',(-7.49837995428014,38.0292018396973,-7.35155079294497));
#10083=CARTESIAN_POINT('Ctrl Pts',(-7.32027095783454,38.040768800468,-7.53321707890824));
#10084=CARTESIAN_POINT('Ctrl Pts',(-7.13556965973243,38.0523357612388,-7.70839463730592));
#10085=CARTESIAN_POINT('Ctrl Pts',(-6.94477534909153,38.0639027220095,-7.87661706258788));
#10086=CARTESIAN_POINT('Ctrl Pts',(-6.77939063709363,38.0739292184461,-8.02243596705831));
#10087=CARTESIAN_POINT('Ctrl Pts',(-6.60942841200211,38.0839557148826,-8.16302942840252));
#10088=CARTESIAN_POINT('Ctrl Pts',(-6.43523447667231,38.0939822113192,-8.2981177522525));
#10089=CARTESIAN_POINT('Ctrl Pts',(-6.23426730180032,38.1055497590579,-8.45396886584565));
#10090=CARTESIAN_POINT('Ctrl Pts',(-6.02760467181233,38.1171173067966,-8.60254000476339));
#10091=CARTESIAN_POINT('Ctrl Pts',(-5.81579678690838,38.1286848545354,-8.74342660136094));
#10092=CARTESIAN_POINT('Ctrl Pts',(-5.6040259696663,38.1402503778832,-8.88428854195134));
#10093=CARTESIAN_POINT('Ctrl Pts',(-5.38711192540109,38.151815901231,-9.01746847168526));
#10094=CARTESIAN_POINT('Ctrl Pts',(-5.16563415427181,38.1633814245789,-9.14260492333671));
#10095=CARTESIAN_POINT('Ctrl Pts',(-4.94418113678743,38.1749456552965,-9.26772738900991));
#10096=CARTESIAN_POINT('Ctrl Pts',(-4.71816565177371,38.1865098860141,-9.38480803549227));
#10097=CARTESIAN_POINT('Ctrl Pts',(-4.48819309123835,38.1980741167318,-9.49353062752527));
#10098=CARTESIAN_POINT('Ctrl Pts',(-4.25820248152583,38.209639255057,-9.60226175254725));
#10099=CARTESIAN_POINT('Ctrl Pts',(-4.0242544245351,38.2212043933823,-9.70263339102094));
#10100=CARTESIAN_POINT('Ctrl Pts',(-3.78697688107134,38.2327695317075,-9.79437629980752));
#10101=CARTESIAN_POINT('Ctrl Pts',(-3.54970371597984,38.2443344566267,-9.88611751570483));
#10102=CARTESIAN_POINT('Ctrl Pts',(-3.30910144613982,38.2558993815458,-9.969230222245));
#10103=CARTESIAN_POINT('Ctrl Pts',(-3.06581660782314,38.2674643064649,-10.0434938904345));
#10104=CARTESIAN_POINT('Ctrl Pts',(-2.82247493856302,38.2790319329318,-10.1177749064964));
#10105=CARTESIAN_POINT('Ctrl Pts',(-2.57644971301954,38.2905995593986,-10.1832026711533));
#10106=CARTESIAN_POINT('Ctrl Pts',(-2.32840260480898,38.3021671858654,-10.2396065505428));
#10107=CARTESIAN_POINT('Ctrl Pts',(-2.11348977034709,38.3121896022117,-10.2884759676535));
#10108=CARTESIAN_POINT('Ctrl Pts',(-1.8970594779061,38.322212018558,-10.3305720727984));
#10109=CARTESIAN_POINT('Ctrl Pts',(-1.67954864780435,38.3322344349043,-10.3658148420497));
#10110=CARTESIAN_POINT('Ctrl Pts',(-1.42852518973776,38.3438010387753,-10.406487583748));
#10111=CARTESIAN_POINT('Ctrl Pts',(-1.17598466307407,38.3553676426462,-10.4380439947674));
#10112=CARTESIAN_POINT('Ctrl Pts',(-0.922603674343791,38.3669342465172,
-10.4603921274533));
#10113=CARTESIAN_POINT('Ctrl Pts',(-0.669267061252899,38.3784988246819,
-10.4827363462202));
#10114=CARTESIAN_POINT('Ctrl Pts',(-0.415090555598662,38.3900634028467,
-10.4958754816972));
#10115=CARTESIAN_POINT('Ctrl Pts',(-0.160755867377762,38.4016279810114,
-10.4997694522834));
#10116=CARTESIAN_POINT('Ctrl Pts',(0.0935504220672181,38.4131912678861,
-10.5036629880725));
#10117=CARTESIAN_POINT('Ctrl Pts',(0.348014582076939,38.4247545547607,-10.4983134159245));
#10118=CARTESIAN_POINT('Ctrl Pts',(0.601953812652019,38.4363178416354,-10.4837327611607));
#10119=CARTESIAN_POINT('Ctrl Pts',(0.855913169215033,38.4478820449599,-10.4691509508051));
#10120=CARTESIAN_POINT('Ctrl Pts',(1.10934723657866,38.4594462482844,-10.4453366084573));
#10121=CARTESIAN_POINT('Ctrl Pts',(1.36157588496065,38.4710104516089,-10.4123538217587));
#10122=CARTESIAN_POINT('Ctrl Pts',(1.61380001522755,38.4825744477865,-10.3793716258734));
#10123=CARTESIAN_POINT('Ctrl Pts',(1.8648184953714,38.494138443964,-10.3372213518512));
#10124=CARTESIAN_POINT('Ctrl Pts',(2.11395819808633,38.5057024401416,-10.2860187505538));
#10125=CARTESIAN_POINT('Ctrl Pts',(2.36315646670326,38.517269154697,-10.2348041129309));
#10126=CARTESIAN_POINT('Ctrl Pts',(2.61047480368251,38.5288358692525,-10.1745329500001));
#10127=CARTESIAN_POINT('Ctrl Pts',(2.85525066777235,38.5404025838079,-10.105372067578));
#10128=CARTESIAN_POINT('Ctrl Pts',(3.06746464147513,38.5504306087018,-10.0454114757192));
#10129=CARTESIAN_POINT('Ctrl Pts',(3.2777676572117,38.5604586335956,-9.97876982858072));
#10130=CARTESIAN_POINT('Ctrl Pts',(3.48573704249832,38.5704866584894,-9.90558621539155));
#10131=CARTESIAN_POINT('Ctrl Pts',(3.7256265304417,38.5820538310016,-9.82117004293616));
#10132=CARTESIAN_POINT('Ctrl Pts',(3.96248524580083,38.5936210035138,-9.7280223607574));
#10133=CARTESIAN_POINT('Ctrl Pts',(4.19567502657272,38.605188176026,-9.62638624154433));
#10134=CARTESIAN_POINT('Ctrl Pts',(4.42882392223932,38.6167533204687,-9.52476794216635));
#10135=CARTESIAN_POINT('Ctrl Pts',(4.65830491383272,38.6283184649115,-9.41466428731077));
#10136=CARTESIAN_POINT('Ctrl Pts',(4.88350017832237,38.6398836093542,-9.29636633359107));
#10137=CARTESIAN_POINT('Ctrl Pts',(5.10867022262449,38.6514474585872,-9.17808162835856));
#10138=CARTESIAN_POINT('Ctrl Pts',(5.32955525319949,38.6630113078201,-9.0516045853062));
#10139=CARTESIAN_POINT('Ctrl Pts',(5.54556142486565,38.6745751570531,-8.91727253609768));
#10140=CARTESIAN_POINT('Ctrl Pts',(5.76158452743253,38.6861399126786,-8.78292995773359));
#10141=CARTESIAN_POINT('Ctrl Pts',(5.97272777009596,38.6977046683041,-8.64073128630361));
#10142=CARTESIAN_POINT('Ctrl Pts',(6.17842456612679,38.7092694239296,-8.4910582897941));
#10143=CARTESIAN_POINT('Ctrl Pts',(6.38411756461389,38.7208339660483,-8.34138805652523));
#10144=CARTESIAN_POINT('Ctrl Pts',(6.58436409479135,38.732398508167,-8.18424393853169));
#10145=CARTESIAN_POINT('Ctrl Pts',(6.77862844023465,38.7439630502857,-8.02004971737968));
#10146=CARTESIAN_POINT('Ctrl Pts',(6.9729382103727,38.7555302965331,-7.85581710280887));
#10147=CARTESIAN_POINT('Ctrl Pts',(7.16126278800572,38.7670975427805,-7.68453126845112));
#10148=CARTESIAN_POINT('Ctrl Pts',(7.34310018304362,38.7786647890279,-7.50665576017609));
#10149=CARTESIAN_POINT('Ctrl Pts',(7.50068867675949,38.7886894867101,-7.35250081634749));
#10150=CARTESIAN_POINT('Ctrl Pts',(7.65340527614783,38.7987141843923,-7.19339723453153));
#10151=CARTESIAN_POINT('Ctrl Pts',(7.80094570771884,38.8087388820745,-7.02966905801567));
#10152=CARTESIAN_POINT('Ctrl Pts',(7.97121434138562,38.8203078571622,-6.8407190013345));
#10153=CARTESIAN_POINT('Ctrl Pts',(8.13464093951674,38.8318768322498,-6.64555079086006));
#10154=CARTESIAN_POINT('Ctrl Pts',(8.29078139631834,38.8434458073375,-6.44468345525688));
#10155=CARTESIAN_POINT('Ctrl Pts',(8.44689466556719,38.8550127680073,-6.2438510951584));
#10156=CARTESIAN_POINT('Ctrl Pts',(8.59572415644224,38.8665797286772,-6.0373218092466));
#10157=CARTESIAN_POINT('Ctrl Pts',(8.73686658849573,38.878146689347,-5.82564702113225));
#10158=CARTESIAN_POINT('Ctrl Pts',(8.87799331885964,38.8897123632257,-5.61399578122921));
#10159=CARTESIAN_POINT('Ctrl Pts',(9.01143454448961,38.9012780371045,-5.39720041215829));
#10160=CARTESIAN_POINT('Ctrl Pts',(9.13683018625149,38.9128437109832,-5.17584149173867));
#10161=CARTESIAN_POINT('Ctrl Pts',(9.26223565280135,38.9244102910361,-4.954465227778));
#10162=CARTESIAN_POINT('Ctrl Pts',(9.37959413660401,38.935976871089,-4.72852493708156));
#10163=CARTESIAN_POINT('Ctrl Pts',(9.48859075957795,38.947543451142,-4.49862716806493));
#10164=CARTESIAN_POINT('Ctrl Pts',(9.59758534383811,38.9591098148492,-4.26873369914254));
#10165=CARTESIAN_POINT('Ctrl Pts',(9.69821826319937,38.9706761785565,-4.03488315072581));
#10166=CARTESIAN_POINT('Ctrl Pts',(9.79022185148132,38.9822425422637,-3.79770418789796));
#10167=CARTESIAN_POINT('Ctrl Pts',(9.88224680885461,38.9938115924171,-3.56047013701305));
#10168=CARTESIAN_POINT('Ctrl Pts',(9.96563832845879,39.0053806425705,-3.31990638438948));
#10169=CARTESIAN_POINT('Ctrl Pts',(10.0401773872344,39.0169496927239,-3.07666037008744));
#10170=CARTESIAN_POINT('Ctrl Pts',(10.1046960415992,39.0269634970358,-2.86611430497557));
#10171=CARTESIAN_POINT('Ctrl Pts',(10.1625830940346,39.0369773013477,-2.6535590560069));
#10172=CARTESIAN_POINT('Ctrl Pts',(10.2137267948667,39.0469911056596,-2.43942328426641));
#10173=CARTESIAN_POINT('Ctrl Pts',(10.2727689972203,39.0585514161357,-2.19221693508691));
#10174=CARTESIAN_POINT('Ctrl Pts',(10.3228415404747,39.0701117266117,-1.94282670607944));
#10175=CARTESIAN_POINT('Ctrl Pts',(10.3638027893578,39.0816720370877,-1.69191983950168));
#10176=CARTESIAN_POINT('Ctrl Pts',(10.404756765153,39.0932302949127,-1.44105752399942));
#10177=CARTESIAN_POINT('Ctrl Pts',(10.4366026314068,39.1047885527376,-1.18867938222004));
#10178=CARTESIAN_POINT('Ctrl Pts',(10.4592500983269,39.1163468105625,-0.935461586944217));
#10179=CARTESIAN_POINT('Ctrl Pts',(10.4818950172023,39.1279037679789,-0.682272280959553));
#10180=CARTESIAN_POINT('Ctrl Pts',(10.495343578375,39.1394607253953,-0.428243786373147));
#10181=CARTESIAN_POINT('Ctrl Pts',(10.4995573756991,39.1510176828117,-0.174057215886499));
#10182=CARTESIAN_POINT('Ctrl Pts',(10.5037715185744,39.1625755879527,0.0801501990879922));
#10183=CARTESIAN_POINT('Ctrl Pts',(10.498749376384,39.1741334930937,0.334515438451618));
#10184=CARTESIAN_POINT('Ctrl Pts',(10.4845046605004,39.1856913982347,0.588356204985865));
#10185=CARTESIAN_POINT('Ctrl Pts',(10.4702601673197,39.1972491226785,0.842193002955999));
#10186=CARTESIAN_POINT('Ctrl Pts',(10.4467934063272,39.2088068471224,1.0955050675247));
#10187=CARTESIAN_POINT('Ctrl Pts',(10.4141701280644,39.2203645715663,1.347613276772));
#10188=CARTESIAN_POINT('Ctrl Pts',(10.381538928838,39.2319251022369,1.59978269813591));
#10189=CARTESIAN_POINT('Ctrl Pts',(10.3397468037936,39.2434856329074,1.85074740453948));
#10190=CARTESIAN_POINT('Ctrl Pts',(10.2889112005542,39.255046163578,2.09983506664455));
#10191=CARTESIAN_POINT('Ctrl Pts',(10.2446487822583,39.2651118854669,2.31671500097967));
#10192=CARTESIAN_POINT('Ctrl Pts',(10.1935311964916,39.2751776073558,2.53217192609222));
#10193=CARTESIAN_POINT('Ctrl Pts',(10.1356674049065,39.2852433292447,2.74576897373338));
#10194=CARTESIAN_POINT('Ctrl Pts',(10.0690759979193,39.296827267396,2.99158293685373));
#10195=CARTESIAN_POINT('Ctrl Pts',(9.99352834835741,39.3084112055473,3.2350090451317));
#10196=CARTESIAN_POINT('Ctrl Pts',(9.90922078800109,39.3199951436986,3.47539125490169));
#10197=CARTESIAN_POINT('Ctrl Pts',(9.82492758520526,39.3315771091076,3.71573252762991));
#10198=CARTESIAN_POINT('Ctrl Pts',(9.73187754086394,39.3431590745166,3.95303067716415));
#10199=CARTESIAN_POINT('Ctrl Pts',(9.63031632810827,39.3547410399256,4.18664644083677));
#10200=CARTESIAN_POINT('Ctrl Pts',(9.52876641285088,39.3663217169763,4.42023621748527));
#10201=CARTESIAN_POINT('Ctrl Pts',(9.41870732932391,39.3779023940269,4.65014417391184));
#10202=CARTESIAN_POINT('Ctrl Pts',(9.30043265936412,39.3894830710776,4.87575156756713));
#10203=CARTESIAN_POINT('Ctrl Pts',(9.18214987722267,39.4010645424197,5.10137443510336));
#10204=CARTESIAN_POINT('Ctrl Pts',(9.05565050760297,39.4126460137618,5.32269590522329));
#10205=CARTESIAN_POINT('Ctrl Pts',(8.92127444893441,39.4242274851039,5.53912115834182));
#10206=CARTESIAN_POINT('Ctrl Pts',(8.7869018820538,39.4358086554992,5.75554078760817));
#10207=CARTESIAN_POINT('Ctrl Pts',(8.64465318193162,39.4473898258945,5.96706422131363));
#10208=CARTESIAN_POINT('Ctrl Pts',(8.49491242743469,39.4589709962898,6.17312431838334));
#10209=CARTESIAN_POINT('Ctrl Pts',(8.34514009761801,39.4705546087668,6.37922786663955));
#10210=CARTESIAN_POINT('Ctrl Pts',(8.18787271707229,39.4821382212438,6.57986555252028));
#10211=CARTESIAN_POINT('Ctrl Pts',(8.02353650941438,39.4937218337208,6.77450093232664));
#10212=CARTESIAN_POINT('Ctrl Pts',(7.88273702232438,39.5036464067572,6.94126005398868));
#10213=CARTESIAN_POINT('Ctrl Pts',(7.73674929148776,39.5135709797935,7.10361351542315));
#10214=CARTESIAN_POINT('Ctrl Pts',(7.58586439719135,39.5234955528298,7.26124385676619));
#10215=CARTESIAN_POINT('Ctrl Pts',(7.41051234539617,39.5350294724659,7.44443518223697));
#10216=CARTESIAN_POINT('Ctrl Pts',(7.22849149706608,39.5465633921019,7.62130277938994));
#10217=CARTESIAN_POINT('Ctrl Pts',(7.04028338094605,39.558097311738,7.79136771792828));
#10218=CARTESIAN_POINT('Ctrl Pts',(6.85210898568282,39.5696291648657,7.96140218628521));
#10219=CARTESIAN_POINT('Ctrl Pts',(6.65774974306552,39.5811610179933,8.12463624128184));
#10220=CARTESIAN_POINT('Ctrl Pts',(6.45772254452777,39.592692871121,8.28062923562563));
#10221=CARTESIAN_POINT('Ctrl Pts',(6.2577168989946,39.6042234816872,8.43660542166661));
#10222=CARTESIAN_POINT('Ctrl Pts',(6.05204473760968,39.6157540922535,8.58534193270929));
#10223=CARTESIAN_POINT('Ctrl Pts',(5.84125523482977,39.6272847028197,8.72643903786498));
#10224=CARTESIAN_POINT('Ctrl Pts',(5.63044338606736,39.6388165357562,8.86755110085016));
#10225=CARTESIAN_POINT('Ctrl Pts',(5.41451334264833,39.6503483686927,9.00102198096848));
#10226=CARTESIAN_POINT('Ctrl Pts',(5.19404353388615,39.6618802016292,9.12649509768649));
#10227=CARTESIAN_POINT('Ctrl Pts',(4.97357359805668,39.6734120412121,9.25196828672065));
#10228=CARTESIAN_POINT('Ctrl Pts',(4.74856413637869,39.6849438807949,9.36944356696252));
#10229=CARTESIAN_POINT('Ctrl Pts',(4.51961908132821,39.6964757203778,9.47860983265447));
#10230=CARTESIAN_POINT('Ctrl Pts',(4.2906085924439,39.7080108558277,9.58780729870271));
#10231=CARTESIAN_POINT('Ctrl Pts',(4.05766051472073,39.7195459912777,9.68869088273747));
#10232=CARTESIAN_POINT('Ctrl Pts',(3.82140107039531,39.7310811267276,9.7809966189127));
#10233=CARTESIAN_POINT('Ctrl Pts',(3.61203246650753,39.74130334329,9.86279619805342));
#10234=CARTESIAN_POINT('Ctrl Pts',(3.40006381849039,39.7515255598525,9.93786007685317));
#10235=CARTESIAN_POINT('Ctrl Pts',(3.18594275547069,39.7617477764149,10.0060366658764));
#10236=CARTESIAN_POINT('Ctrl Pts',(2.94219156771723,39.7733845457893,10.0836475478562));
#10237=CARTESIAN_POINT('Ctrl Pts',(2.69557041193126,39.7850213151637,10.1523578833729));
#10238=CARTESIAN_POINT('Ctrl Pts',(2.44674288382941,39.7966580845381,10.2119758254919));
#10239=CARTESIAN_POINT('Ctrl Pts',(2.19796065802866,39.8082927352867,10.2715829133858));
#10240=CARTESIAN_POINT('Ctrl Pts',(1.94697312436059,39.8199273860353,10.3221008501457));
#10241=CARTESIAN_POINT('Ctrl Pts',(1.69445649222457,39.8315620367839,10.3633883549715));
#10242=CARTESIAN_POINT('Ctrl Pts',(1.44197452343055,39.8431950904262,10.4046701921987));
#10243=CARTESIAN_POINT('Ctrl Pts',(1.18796414163377,39.8548281440686,10.4367240840553));
#10244=CARTESIAN_POINT('Ctrl Pts',(0.933110299572317,39.866461197711,10.4594601279814));
#10245=CARTESIAN_POINT('Ctrl Pts',(0.678258384732152,39.8780941633835,10.482195999976));
#10246=CARTESIAN_POINT('Ctrl Pts',(0.422563290990595,39.8897271290559,10.4956141379029));
#10247=CARTESIAN_POINT('Ctrl Pts',(0.166714969412438,39.9013600947284,10.4996765244923));
#10248=CARTESIAN_POINT('Ctrl Pts',(-0.0891139888816756,39.912992179987,
10.5037386036294));
#10249=CARTESIAN_POINT('Ctrl Pts',(-0.345095881899718,39.9246242652456,
10.4984463426919));
#10250=CARTESIAN_POINT('Ctrl Pts',(-0.600539942610578,39.9362563505041,
10.4838138469418));
#10251=CARTESIAN_POINT('Ctrl Pts',(-0.856008621241452,39.9478895567821,
10.4691799410137));
#10252=CARTESIAN_POINT('Ctrl Pts',(-1.11093909430189,39.9595227630601,10.4452040152679));
#10253=CARTESIAN_POINT('Ctrl Pts',(-1.36464347042229,39.971155969338,10.411952228023));
#10254=CARTESIAN_POINT('Ctrl Pts',(-1.57432647122329,39.9807706462253,10.3844701063579));
#10255=CARTESIAN_POINT('Ctrl Pts',(-1.7831719369394,39.9903853231127,10.3506527957081));
#10256=CARTESIAN_POINT('Ctrl Pts',(-1.99079507083262,40.,10.3105642903746));
#10257=CARTESIAN_POINT('Origin',(0.,13.3748739960349,0.));
#10258=CARTESIAN_POINT('',(-12.1744999965607,38.6251260039651,0.00028938649696687));
#10259=CARTESIAN_POINT('Ctrl Pts',(1.59078448392769,37.8125509746976,12.0701224093087));
#10260=CARTESIAN_POINT('Ctrl Pts',(1.30897780039443,37.8236982341459,12.1072631842262));
#10261=CARTESIAN_POINT('Ctrl Pts',(1.02589220353336,37.8348454935942,12.134527500853));
#10262=CARTESIAN_POINT('Ctrl Pts',(0.74223387350245,37.8459927530425,12.1518533206678));
#10263=CARTESIAN_POINT('Ctrl Pts',(0.547788829828789,37.8536340916558,12.1637300026965));
#10264=CARTESIAN_POINT('Ctrl Pts',(0.353074788441565,37.8612754302692,12.170937692811));
#10265=CARTESIAN_POINT('Ctrl Pts',(0.158319908679642,37.8689167688825,12.173470542804));
#10266=CARTESIAN_POINT('Ctrl Pts',(-0.12579174714368,37.8800640806664,12.1771655064749));
#10267=CARTESIAN_POINT('Ctrl Pts',(-0.410075244090132,37.8912113924504,
12.1709105297779));
#10268=CARTESIAN_POINT('Ctrl Pts',(-0.69382202769014,37.9023587042343,12.1547135401823));
#10269=CARTESIAN_POINT('Ctrl Pts',(-0.97752061690601,37.9135041226476,12.138519301645));
#10270=CARTESIAN_POINT('Ctrl Pts',(-1.26068240856565,37.9246495410609,12.1123864367957));
#10271=CARTESIAN_POINT('Ctrl Pts',(-1.54260128195161,37.9357949594742,12.0763749335188));
#10272=CARTESIAN_POINT('Ctrl Pts',(-1.82448885756292,37.9469391405571,12.0403674281293));
#10273=CARTESIAN_POINT('Ctrl Pts',(-2.10513352590578,37.95808332164,11.9944835080307));
#10274=CARTESIAN_POINT('Ctrl Pts',(-2.3838354609949,37.9692275027229,11.9388348989716));
#10275=CARTESIAN_POINT('Ctrl Pts',(-2.67131404013712,37.9807226268683,11.8814338512953));
#10276=CARTESIAN_POINT('Ctrl Pts',(-2.95672525267232,37.9922177510137,11.8136431952157));
#10277=CARTESIAN_POINT('Ctrl Pts',(-3.23931225686388,38.0037128751591,11.735642562405));
#10278=CARTESIAN_POINT('Ctrl Pts',(-3.51328659390697,38.0148576517066,11.6600192274806));
#10279=CARTESIAN_POINT('Ctrl Pts',(-3.78460605649641,38.0260024282542,11.5747991324066));
#10280=CARTESIAN_POINT('Ctrl Pts',(-4.05259512972827,38.0371472048018,11.4801969915373));
#10281=CARTESIAN_POINT('Ctrl Pts',(-4.33322097422901,38.0488175027461,11.3811339761955));
#10282=CARTESIAN_POINT('Ctrl Pts',(-4.61019448973532,38.0604878006904,11.2717829285034));
#10283=CARTESIAN_POINT('Ctrl Pts',(-4.88276104735215,38.0721580986347,11.152447928794));
#10284=CARTESIAN_POINT('Ctrl Pts',(-5.15532760496899,38.0838283965791,11.0331129290845));
#10285=CARTESIAN_POINT('Ctrl Pts',(-5.42348690088374,38.0954986945234,10.9037941199549));
#10286=CARTESIAN_POINT('Ctrl Pts',(-5.68651039168178,38.1071689924677,10.7648525217624));
#10287=CARTESIAN_POINT('Ctrl Pts',(-5.93774685158698,38.1183163022865,10.6321373975067));
#10288=CARTESIAN_POINT('Ctrl Pts',(-6.18437272836615,38.1294636121054,10.4906033555107));
#10289=CARTESIAN_POINT('Ctrl Pts',(-6.42576965953203,38.1406109219243,10.340596430218));
#10290=CARTESIAN_POINT('Ctrl Pts',(-6.66712559058785,38.1517563384261,10.1906149828815));
#10291=CARTESIAN_POINT('Ctrl Pts',(-6.9032541226648,38.1629017549279,10.0321636661054));
#10292=CARTESIAN_POINT('Ctrl Pts',(-7.13356394341092,38.1740471714297,9.86563306206286));
#10293=CARTESIAN_POINT('Ctrl Pts',(-7.36384819705636,38.1851913506591,9.69912094487725));
#10294=CARTESIAN_POINT('Ctrl Pts',(-7.58831481311788,38.1963355298885,9.52453148764227));
#10295=CARTESIAN_POINT('Ctrl Pts',(-7.80640276521373,38.2074797091179,9.34229768939438));
#10296=CARTESIAN_POINT('Ctrl Pts',(-8.03135862286497,38.2189748346958,9.15432508483766));
#10297=CARTESIAN_POINT('Ctrl Pts',(-8.24952732595125,38.2304699602737,8.95821905765051));
#10298=CARTESIAN_POINT('Ctrl Pts',(-8.46033028003315,38.2419650858516,8.75449951754835));
#10299=CARTESIAN_POINT('Ctrl Pts',(-8.66470833983174,38.2531098607101,8.55698898203202));
#10300=CARTESIAN_POINT('Ctrl Pts',(-8.86216279097333,38.2642546355686,8.35232234771498));
#10301=CARTESIAN_POINT('Ctrl Pts',(-9.05220323824906,38.2753994104272,8.14101141034904));
#10302=CARTESIAN_POINT('Ctrl Pts',(-9.25120494426631,38.2870697113648,7.91973621531168));
#10303=CARTESIAN_POINT('Ctrl Pts',(-9.44207640298544,38.2987400123023,7.69117525897117));
#10304=CARTESIAN_POINT('Ctrl Pts',(-9.6243005169155,38.3104103132399,7.45595666632393));
#10305=CARTESIAN_POINT('Ctrl Pts',(-9.80652463084557,38.3220806141775,7.22073807367666));
#10306=CARTESIAN_POINT('Ctrl Pts',(-9.98010120145821,38.3337509151151,6.97886211532039));
#10307=CARTESIAN_POINT('Ctrl Pts',(-10.144563284333,38.3454212160527,6.73099443025792));
#10308=CARTESIAN_POINT('Ctrl Pts',(-10.3016546456759,38.3565684873844,6.49423546795641));
#10309=CARTESIAN_POINT('Ctrl Pts',(-10.4504774518845,38.367715758716,6.25193932153469));
#10310=CARTESIAN_POINT('Ctrl Pts',(-10.5906543344632,38.3788630300476,6.00470573949428));
#10311=CARTESIAN_POINT('Ctrl Pts',(-10.7308074057654,38.3900084078376,5.7575141540162));
#10312=CARTESIAN_POINT('Ctrl Pts',(-10.8623173540756,38.4011537856276,5.50538703934738));
#10313=CARTESIAN_POINT('Ctrl Pts',(-10.9848518805822,38.4122991634176,5.24895031522197));
#10314=CARTESIAN_POINT('Ctrl Pts',(-11.1073728029286,38.4234433038135,4.99254206149096));
#10315=CARTESIAN_POINT('Ctrl Pts',(-11.2209201783031,38.4345874442093,4.73182539434702));
#10316=CARTESIAN_POINT('Ctrl Pts',(-11.3252085991643,38.4457315846052,4.46744898520573));
#10317=CARTESIAN_POINT('Ctrl Pts',(-11.4327818597973,38.4572267391913,4.19474534149411));
#10318=CARTESIAN_POINT('Ctrl Pts',(-11.5305033242619,38.4687218937773,3.91814794521018));
#10319=CARTESIAN_POINT('Ctrl Pts',(-11.6181137451896,38.4802170483634,3.63839020087693));
#10320=CARTESIAN_POINT('Ctrl Pts',(-11.7030534493892,38.4913617845709,3.36716059371813));
#10321=CARTESIAN_POINT('Ctrl Pts',(-11.7784893469094,38.5025065207784,3.09296073127381));
#10322=CARTESIAN_POINT('Ctrl Pts',(-11.8442357567959,38.513651256986,2.81647467367221));
#10323=CARTESIAN_POINT('Ctrl Pts',(-11.9130830140131,38.5253216207613,2.52694849638708));
#10324=CARTESIAN_POINT('Ctrl Pts',(-11.9713047289161,38.5369919845366,2.23491559225353));
#10325=CARTESIAN_POINT('Ctrl Pts',(-12.0187474391742,38.5486623483119,1.94117496463956));
#10326=CARTESIAN_POINT('Ctrl Pts',(-12.0661901494323,38.5603327120872,1.64743433702562));
#10327=CARTESIAN_POINT('Ctrl Pts',(-12.1028538102164,38.5720030758626,1.35198631855737));
#10328=CARTESIAN_POINT('Ctrl Pts',(-12.1286469510863,38.5836734396379,1.05563885202526));
#10329=CARTESIAN_POINT('Ctrl Pts',(-12.1549901730804,38.5955926931028,0.752971288674556));
#10330=CARTESIAN_POINT('Ctrl Pts',(-12.1700001024465,38.6075119465678,0.449311157315627));
#10331=CARTESIAN_POINT('Ctrl Pts',(-12.173630879507,38.6194312000327,0.145469789009793));
#10332=CARTESIAN_POINT('Ctrl Pts',(-12.1742091193982,38.6213294680102,0.0970798171563845));
#10333=CARTESIAN_POINT('Ctrl Pts',(-12.1744988461963,38.6232277359876,0.0486852550215822));
#10334=CARTESIAN_POINT('Ctrl Pts',(-12.1744999965607,38.6251260039651,0.00028938649696687));
#10335=CARTESIAN_POINT('',(11.7598063682261,40.,-3.15424737243508));
#10336=CARTESIAN_POINT('Ctrl Pts',(-12.1748649577908,38.6251260151384,0.000289110302658423));
#10337=CARTESIAN_POINT('Ctrl Pts',(-12.1731836483798,38.6907258978333,-1.67221371080106));
#10338=CARTESIAN_POINT('Ctrl Pts',(-11.4051697641933,38.8357431883897,-5.37100026957135));
#10339=CARTESIAN_POINT('Ctrl Pts',(-7.77755196994913,39.060177886808,-10.0290176561892));
#10340=CARTESIAN_POINT('Ctrl Pts',(-2.02988957584845,39.2984301103931,-12.5280053565324));
#10341=CARTESIAN_POINT('Ctrl Pts',(4.21283654000685,39.5366823339782,-11.9717980432598));
#10342=CARTESIAN_POINT('Ctrl Pts',(9.3318903658005,39.7705389638472,-8.56008252992691));
#10343=CARTESIAN_POINT('Ctrl Pts',(11.263434788298,39.9249781858544,-5.00116413859683));
#10344=CARTESIAN_POINT('Ctrl Pts',(11.7598063682261,40.,-3.15424737243508));
#10345=CARTESIAN_POINT('',(8.61094305413662,40.,-8.60639936142963));
#10346=CARTESIAN_POINT('Origin',(0.,40.,0.));
#10347=CARTESIAN_POINT('',(-12.1744916248676,38.8748739948544,0.000309104184771874));
#10348=CARTESIAN_POINT('Ctrl Pts',(-12.1742135449704,38.8748739960349,0.000309067021438125));
#10349=CARTESIAN_POINT('Ctrl Pts',(-12.1728218038936,38.9322463659098,-1.46265402061263));
#10350=CARTESIAN_POINT('Ctrl Pts',(-11.5435367915227,39.0690361436464,-4.95189231269601));
#10351=CARTESIAN_POINT('Ctrl Pts',(-8.28522524716096,39.2852433292447,-9.61375508410346));
#10352=CARTESIAN_POINT('Ctrl Pts',(-2.67484068581488,39.5234955528298,-12.4063460053113));
#10353=CARTESIAN_POINT('Ctrl Pts',(3.58926667070469,39.7617477764149,-12.1735736829301));
#10354=CARTESIAN_POINT('Ctrl Pts',(7.17942834059384,39.9205825921383,-10.0386698338782));
#10355=CARTESIAN_POINT('Ctrl Pts',(8.61094305413662,40.,-8.60639936142963));
#10356=CARTESIAN_POINT('Ctrl Pts',(1.59078448392772,38.0622997972676,12.0701224093087));
#10357=CARTESIAN_POINT('Ctrl Pts',(1.32384075218273,38.0728606019514,12.1053043181693));
#10358=CARTESIAN_POINT('Ctrl Pts',(1.05575738715399,38.0834214066353,12.131623455312));
#10359=CARTESIAN_POINT('Ctrl Pts',(0.787134657080782,38.0939822113192,12.1490275035339));
#10360=CARTESIAN_POINT('Ctrl Pts',(0.503583140229768,38.1051299358117,12.1673987868252));
#10361=CARTESIAN_POINT('Ctrl Pts',(0.219345890921422,38.1162776603042,12.1758415742294));
#10362=CARTESIAN_POINT('Ctrl Pts',(-0.0648690228389137,38.1274253847967,
12.1743271789399));
#10363=CARTESIAN_POINT('Ctrl Pts',(-0.349035688152791,38.1385712168467,
12.1728130407349));
#10364=CARTESIAN_POINT('Ctrl Pts',(-0.633179758886583,38.1497170488967,
12.1613450960154));
#10365=CARTESIAN_POINT('Ctrl Pts',(-0.916592908336909,38.1608628809466,
12.1399467746109));
#10366=CARTESIAN_POINT('Ctrl Pts',(-1.19997459133722,38.1720074755108,12.1185508289933));
#10367=CARTESIAN_POINT('Ctrl Pts',(-1.48262524921969,38.1831520700749,12.0872267283601));
#10368=CARTESIAN_POINT('Ctrl Pts',(-1.76384016867791,38.194296664639,12.0460498965162));
#10369=CARTESIAN_POINT('Ctrl Pts',(-2.05389228566501,38.2057914788278,12.0035790799957));
#10370=CARTESIAN_POINT('Ctrl Pts',(-2.34241667380791,38.2172862930165,11.9506263064734));
#10371=CARTESIAN_POINT('Ctrl Pts',(-2.62864831310905,38.2287811072053,11.8873318409132));
#10372=CARTESIAN_POINT('Ctrl Pts',(-2.90617384669823,38.2399262917455,11.8259625584302));
#10373=CARTESIAN_POINT('Ctrl Pts',(-3.18154377189134,38.2510714762857,11.7548714598031));
#10374=CARTESIAN_POINT('Ctrl Pts',(-3.45407233157046,38.2622166608259,11.6742380727086));
#10375=CARTESIAN_POINT('Ctrl Pts',(-3.73942491370659,38.2738862898389,11.5898104250489));
#10376=CARTESIAN_POINT('Ctrl Pts',(-4.02166199993082,38.285555918852,11.4949209773659));
#10377=CARTESIAN_POINT('Ctrl Pts',(-4.30001441364412,38.2972255478651,11.3898343399916));
#10378=CARTESIAN_POINT('Ctrl Pts',(-4.57836682735739,38.3088951768782,11.2847477026174));
#10379=CARTESIAN_POINT('Ctrl Pts',(-4.85283425796642,38.3205648058912,11.1694640021579));
#10380=CARTESIAN_POINT('Ctrl Pts',(-5.12267062571763,38.3322344349043,11.0443060402367));
#10381=CARTESIAN_POINT('Ctrl Pts',(-5.38041794246529,38.343381248029,10.9247553320664));
#10382=CARTESIAN_POINT('Ctrl Pts',(-5.63401694334377,38.3545280611537,10.796160008172));
#10383=CARTESIAN_POINT('Ctrl Pts',(-5.88283226064311,38.3656748742783,10.6588336530381));
#10384=CARTESIAN_POINT('Ctrl Pts',(-6.1316053072015,38.376819793693,10.5215306280063));
#10385=CARTESIAN_POINT('Ctrl Pts',(-6.37559605922401,38.3879647131077,10.3754996620031));
#10386=CARTESIAN_POINT('Ctrl Pts',(-6.61419386041611,38.3991096325224,10.2211002258482));
#10387=CARTESIAN_POINT('Ctrl Pts',(-6.85276519254124,38.4102533155651,10.066717918137));
#10388=CARTESIAN_POINT('Ctrl Pts',(-7.08594454455926,38.4213969986079,9.90396913897554));
#10389=CARTESIAN_POINT('Ctrl Pts',(-7.31314931363975,38.4325406816507,9.7332572845071));
#10390=CARTESIAN_POINT('Ctrl Pts',(-7.54752711982908,38.4440361797206,9.55715591963368));
#10391=CARTESIAN_POINT('Ctrl Pts',(-7.77554672721654,38.4555316777905,9.37258068116194));
#10392=CARTESIAN_POINT('Ctrl Pts',(-7.99660336458607,38.4670271758604,9.18002096291129));
#10393=CARTESIAN_POINT('Ctrl Pts',(-8.21090626771047,38.4781714628565,8.99334433950392));
#10394=CARTESIAN_POINT('Ctrl Pts',(-8.41866514053532,38.4893157498526,8.79916406173953));
#10395=CARTESIAN_POINT('Ctrl Pts',(-8.61936384853658,38.5004600368487,8.59796586970085));
#10396=CARTESIAN_POINT('Ctrl Pts',(-8.82955005566236,38.5121311404555,8.38725656675452));
#10397=CARTESIAN_POINT('Ctrl Pts',(-9.03199227177261,38.5238022440623,8.16885006407581));
#10398=CARTESIAN_POINT('Ctrl Pts',(-9.22614151152845,38.535473347669,7.94334709421989));
#10399=CARTESIAN_POINT('Ctrl Pts',(-9.42029075128428,38.5471444512758,7.71784412436397));
#10400=CARTESIAN_POINT('Ctrl Pts',(-9.60614680231032,38.5588155548826,7.4852449475224));
#10401=CARTESIAN_POINT('Ctrl Pts',(-9.78320885115772,38.5704866584894,7.24619036629795));
#10402=CARTESIAN_POINT('Ctrl Pts',(-9.95232519265855,38.5816340181642,7.01786342408272));
#10403=CARTESIAN_POINT('Ctrl Pts',(-10.1134700589456,38.592781377839,6.78357934184873));
#10404=CARTESIAN_POINT('Ctrl Pts',(-10.2662355845482,38.6039287375138,6.54391757073364));
#10405=CARTESIAN_POINT('Ctrl Pts',(-10.4189751284731,38.6150742012955,6.30429656022115));
#10406=CARTESIAN_POINT('Ctrl Pts',(-10.5633380336435,38.6262196650772,6.05929991170006));
#10407=CARTESIAN_POINT('Ctrl Pts',(-10.6989600913802,38.6373651288589,5.80953554193913));
#10408=CARTESIAN_POINT('Ctrl Pts',(-10.8345670610239,38.6485093526963,5.55979895872045));
#10409=CARTESIAN_POINT('Ctrl Pts',(-10.9614349977632,38.6596535765337,5.30529594776737));
#10410=CARTESIAN_POINT('Ctrl Pts',(-11.0792453455692,38.6707978003711,5.04665957071439));
#10411=CARTESIAN_POINT('Ctrl Pts',(-11.20076485087,38.682292890513,4.77988024973298));
#10412=CARTESIAN_POINT('Ctrl Pts',(-11.3126470548315,38.693787980655,4.50870334116523));
#10413=CARTESIAN_POINT('Ctrl Pts',(-11.4145951579047,38.7052830707969,4.23384785167571));
#10414=CARTESIAN_POINT('Ctrl Pts',(-11.5134367040608,38.7164278831925,3.96736774334894));
#10415=CARTESIAN_POINT('Ctrl Pts',(-11.6029405119847,38.7275726955881,3.69743018378309));
#10416=CARTESIAN_POINT('Ctrl Pts',(-11.6828857891978,38.7387175079836,3.42470873017855));
#10417=CARTESIAN_POINT('Ctrl Pts',(-11.7666000466156,38.7503877369988,3.13912995972093));
#10418=CARTESIAN_POINT('Ctrl Pts',(-11.8398327384508,38.7620579660139,2.85049879505899));
#10419=CARTESIAN_POINT('Ctrl Pts',(-11.9023893162427,38.7737281950291,2.55960520678335));
#10420=CARTESIAN_POINT('Ctrl Pts',(-11.9649458940345,38.7853984240442,2.26871161850769));
#10421=CARTESIAN_POINT('Ctrl Pts',(-12.0168262958164,38.7970686530593,1.97555593644156));
#10422=CARTESIAN_POINT('Ctrl Pts',(-12.0578974154622,38.8087388820745,1.68094026312326));
#10423=CARTESIAN_POINT('Ctrl Pts',(-12.0989059319874,38.8203913226104,1.38677366109214));
#10424=CARTESIAN_POINT('Ctrl Pts',(-12.1291472088389,38.8320437631464,1.0910923577));
#10425=CARTESIAN_POINT('Ctrl Pts',(-12.1485371754145,38.8436962036824,0.794666437929197));
#10426=CARTESIAN_POINT('Ctrl Pts',(-12.1658307293892,38.8540888007279,0.530289621029534));
#10427=CARTESIAN_POINT('Ctrl Pts',(-12.1744932675459,38.8644813977734,0.265320699870421));
#10428=CARTESIAN_POINT('Ctrl Pts',(-12.174499996076,38.8748739948188,0.000309105303522327));
#10429=CARTESIAN_POINT('Ctrl Pts',(7.93208051261574,20.0005837734501,-6.87965285147223));
#10430=CARTESIAN_POINT('Ctrl Pts',(9.07668263151754,20.0800217251941,-5.55995978932681));
#10431=CARTESIAN_POINT('Ctrl Pts',(10.6930139230921,20.2388770847998,-2.33991560351307));
#10432=CARTESIAN_POINT('Ctrl Pts',(10.5082240576505,20.4771498522672,3.06359191036739));
#10433=CARTESIAN_POINT('Ctrl Pts',(7.7610444220363,20.7154020758523,7.71831352629605));
#10434=CARTESIAN_POINT('Ctrl Pts',(3.12105089944607,20.9536542994374,10.4913407524211));
#10435=CARTESIAN_POINT('Ctrl Pts',(-2.28002032107308,21.1919065230225,10.7055409903604));
#10436=CARTESIAN_POINT('Ctrl Pts',(-7.12508829170954,21.4301587466076,8.30910926435329));
#10437=CARTESIAN_POINT('Ctrl Pts',(-10.2325364964883,21.6684109701927,3.88625151956404));
#10438=CARTESIAN_POINT('Ctrl Pts',(-10.8445684035224,21.9066631937778,-1.48431630400501));
#10439=CARTESIAN_POINT('Ctrl Pts',(-8.81191628458542,22.1449154173629,-6.49291954617507));
#10440=CARTESIAN_POINT('Ctrl Pts',(-4.63029122950666,22.383167640948,-9.91807630779845));
#10441=CARTESIAN_POINT('Ctrl Pts',(0.680530483683632,22.6214198645331,-10.9245019479025));
#10442=CARTESIAN_POINT('Ctrl Pts',(5.82538981214024,22.8596720881182,-9.26675138990805));
#10443=CARTESIAN_POINT('Ctrl Pts',(9.54960316733972,23.0979243117033,-5.34910593878247));
#10444=CARTESIAN_POINT('Ctrl Pts',(10.9449409563647,23.3361765352884,-0.126965784354505));
#10445=CARTESIAN_POINT('Ctrl Pts',(9.67112030848427,23.5744287588735,5.12613742673736));
#10446=CARTESIAN_POINT('Ctrl Pts',(6.03878961601208,23.8126809824586,9.12912226706514));
#10447=CARTESIAN_POINT('Ctrl Pts',(0.933770628914186,24.0509332060437,10.9057748640797));
#10448=CARTESIAN_POINT('Ctrl Pts',(-4.3989683509955,24.2891854296288,10.0228204950036));
#10449=CARTESIAN_POINT('Ctrl Pts',(-8.65892458966233,24.5274376532139,6.69558646125051));
#10450=CARTESIAN_POINT('Ctrl Pts',(-10.8072164379082,24.765689876799,1.7354901366115));
#10451=CARTESIAN_POINT('Ctrl Pts',(-10.3199368707579,25.0039421003841,-3.64784266760709));
#10452=CARTESIAN_POINT('Ctrl Pts',(-7.31591945824722,25.2421943239692,-8.14157083244356));
#10453=CARTESIAN_POINT('Ctrl Pts',(-2.52775824622543,25.4804465475543,-10.6498024110112));
#10454=CARTESIAN_POINT('Ctrl Pts',(2.8768510043701,25.7186987711394,-10.5608513596116));
#10455=CARTESIAN_POINT('Ctrl Pts',(7.5798784633816,25.9569509947245,-7.89641029984006));
#10456=CARTESIAN_POINT('Ctrl Pts',(10.4343900608802,26.1952032183096,-3.30626030429192));
#10457=CARTESIAN_POINT('Ctrl Pts',(10.7442519485492,26.4334554418947,2.09019214633302));
#10458=CARTESIAN_POINT('Ctrl Pts',(8.43389766221118,26.6717076654798,6.9769064323582));
#10459=CARTESIAN_POINT('Ctrl Pts',(4.06675662420537,26.9099598890649,10.1621525132199));
#10460=CARTESIAN_POINT('Ctrl Pts',(-1.29215020014935,27.14821211265,10.8691398464998));
#10461=CARTESIAN_POINT('Ctrl Pts',(-6.33593849695176,27.3864643362351,8.92545441450063));
#10462=CARTESIAN_POINT('Ctrl Pts',(-9.83457236079029,27.6247165598202,4.80510557874393));
#10463=CARTESIAN_POINT('Ctrl Pts',(-10.934834919905,27.8629687834053,-0.487071264723974));
#10464=CARTESIAN_POINT('Ctrl Pts',(-9.36840356171729,28.1012210069904,-5.66046533840602));
#10465=CARTESIAN_POINT('Ctrl Pts',(-5.51728615423312,28.3394732305755,-9.45343358969647));
#10466=CARTESIAN_POINT('Ctrl Pts',(-0.320660237907371,28.5777254541606,
-10.9409793964854));
#10467=CARTESIAN_POINT('Ctrl Pts',(4.95416555177833,28.8159776777457,-9.76033282363192));
#10468=CARTESIAN_POINT('Ctrl Pts',(9.02081186376675,29.0542299013308,-6.1994198487454));
#10469=CARTESIAN_POINT('Ctrl Pts',(10.8875398137095,29.2924821249159,-1.12664543996017));
#10470=CARTESIAN_POINT('Ctrl Pts',(10.0991077719128,29.530734348501,4.22088561249689));
#10471=CARTESIAN_POINT('Ctrl Pts',(6.84779179425367,29.7689865720861,8.53906322057902));
#10472=CARTESIAN_POINT('Ctrl Pts',(1.92649498392104,30.0072387956712,10.7748072010324));
#10473=CARTESIAN_POINT('Ctrl Pts',(-3.46461892863268,30.2454910192563,10.3828834541207));
#10474=CARTESIAN_POINT('Ctrl Pts',(-8.0108112405926,30.4837432428414,7.45887098762869));
#10475=CARTESIAN_POINT('Ctrl Pts',(-10.6033954949622,30.7219954664265,2.71585292678186));
#10476=CARTESIAN_POINT('Ctrl Pts',(-10.6101144412331,30.9602476900116,-2.68948409298712));
#10477=CARTESIAN_POINT('Ctrl Pts',(-8.02932952031574,31.1984999135967,-7.43893275925249));
#10478=CARTESIAN_POINT('Ctrl Pts',(-3.49042046230085,31.4367521371818,-10.3742381955904));
#10479=CARTESIAN_POINT('Ctrl Pts',(1.89970245342874,31.6750043607669,-10.7795632439784));
#10480=CARTESIAN_POINT('Ctrl Pts',(6.8265421998787,31.913256584352,-8.55606070196843));
#10481=CARTESIAN_POINT('Ctrl Pts',(10.0885832827944,32.1515088079371,-4.24597933209919));
#10482=CARTESIAN_POINT('Ctrl Pts',(10.8903070521443,32.3897610315222,1.09957512363163));
#10483=CARTESIAN_POINT('Ctrl Pts',(9.03619597933803,32.6280132551074,6.1769746126635));
#10484=CARTESIAN_POINT('Ctrl Pts',(4.97841479809776,32.8662654786924,9.7479864197984));
#10485=CARTESIAN_POINT('Ctrl Pts',(-0.293459559412273,33.1045177022776,
10.9417427601586));
#10486=CARTESIAN_POINT('Ctrl Pts',(-5.49376751214475,33.3427699258626,9.46712055827954));
#10487=CARTESIAN_POINT('Ctrl Pts',(-9.35430248110292,33.5810221494478,5.68373805118744));
#10488=CARTESIAN_POINT('Ctrl Pts',(-10.9335902515748,33.8192743730328,0.514254171769246));
#10489=CARTESIAN_POINT('Ctrl Pts',(-9.84648764379592,34.0575265966179,-4.78064161206769));
#10490=CARTESIAN_POINT('Ctrl Pts',(-6.35810793409936,34.295778820203,-8.90967545092836));
#10491=CARTESIAN_POINT('Ctrl Pts',(-1.3191672989035,34.5340310437881,-10.8658939245695));
#10492=CARTESIAN_POINT('Ctrl Pts',(4.04148056253829,34.7722832673732,-10.1722312205807));
#10493=CARTESIAN_POINT('Ctrl Pts',(8.41652674720532,35.0105354909583,-6.9978518601521));
#10494=CARTESIAN_POINT('Ctrl Pts',(10.7390224500958,35.2487877145434,-2.11689630296171));
#10495=CARTESIAN_POINT('Ctrl Pts',(10.4425773045532,35.4870399381285,3.28030979990781));
#10496=CARTESIAN_POINT('Ctrl Pts',(7.59948581375965,35.7252921617136,7.87754203452586));
#10497=CARTESIAN_POINT('Ctrl Pts',(2.90309678978814,35.9635443852987,10.5536667643604));
#10498=CARTESIAN_POINT('Ctrl Pts',(-2.50127462534687,36.2017966088839,10.6560536034062));
#10499=CARTESIAN_POINT('Ctrl Pts',(-7.29565659631146,36.4400488324689,8.15973332519128));
#10500=CARTESIAN_POINT('Ctrl Pts',(-10.310836309689,36.678301056054,3.67348714751023));
#10501=CARTESIAN_POINT('Ctrl Pts',(-10.811497527272,36.9165532796391,-1.70861762580354));
#10502=CARTESIAN_POINT('Ctrl Pts',(-8.67554332886272,37.1548055032242,-6.67403935727874));
#10503=CARTESIAN_POINT('Ctrl Pts',(-4.42387183430699,37.3930577268093,-10.0118535213315));
#10504=CARTESIAN_POINT('Ctrl Pts',(0.906655509484174,37.6313099503944,-10.9080625518847));
#10505=CARTESIAN_POINT('Ctrl Pts',(6.01607574523276,37.8695621739795,-9.14410671556304));
#10506=CARTESIAN_POINT('Ctrl Pts',(9.65834638546719,38.1078143975646,-5.15016435505535));
#10507=CARTESIAN_POINT('Ctrl Pts',(10.9452233105833,38.3460666211498,0.0997558540279738));
#10508=CARTESIAN_POINT('Ctrl Pts',(9.56287066352806,38.5843188447348,5.32534873881454));
#10509=CARTESIAN_POINT('Ctrl Pts',(5.84841145753922,38.82257106832,9.25224060771052));
#10510=CARTESIAN_POINT('Ctrl Pts',(0.70768278248567,39.060823291905,10.9227763791256));
#10511=CARTESIAN_POINT('Ctrl Pts',(-4.60561153353682,39.2990755154902,9.92955670850569));
#10512=CARTESIAN_POINT('Ctrl Pts',(-8.79576482446728,39.5373277390752,6.51480629675831));
#10513=CARTESIAN_POINT('Ctrl Pts',(-10.8408098726847,39.7755799626604,1.51127160533644));
#10514=CARTESIAN_POINT('Ctrl Pts',(-10.2422364118163,40.0138321862454,-3.86080079579494));
#10515=CARTESIAN_POINT('Ctrl Pts',(-7.14558203450444,40.2520844098305,-8.29137091192963));
#10516=CARTESIAN_POINT('Ctrl Pts',(-2.30691296609827,40.4903366334156,-10.6998374196014));
#10517=CARTESIAN_POINT('Ctrl Pts',(3.09555850011698,40.7285888570008,-10.4990832245953));
#10518=CARTESIAN_POINT('Ctrl Pts',(6.19188889114855,40.8874236727241,-8.65783810040184));
#10519=CARTESIAN_POINT('Ctrl Pts',(7.42649694513297,40.9668410805858,-7.4225782431051));
#10520=CARTESIAN_POINT('Ctrl Pts',(8.35397305039485,19.6781514844946,-7.24556872889312));
#10521=CARTESIAN_POINT('Ctrl Pts',(9.5594544167933,19.7575894362386,-5.8556836592167));
#10522=CARTESIAN_POINT('Ctrl Pts',(11.2617553489193,19.9164447958442,-2.46437134127127));
#10523=CARTESIAN_POINT('Ctrl Pts',(11.0671368558985,20.1547175633116,3.22653863837005));
#10524=CARTESIAN_POINT('Ctrl Pts',(8.17383986981593,20.3929697868967,8.12883619759329));
#10525=CARTESIAN_POINT('Ctrl Pts',(3.28705376368968,20.6312220104819,11.0493555592179));
#10526=CARTESIAN_POINT('Ctrl Pts',(-2.40129034069979,20.869474234067,11.2749487074831));
#10527=CARTESIAN_POINT('Ctrl Pts',(-7.5040584214893,21.1077264576521,8.75105525678824));
#10528=CARTESIAN_POINT('Ctrl Pts',(-10.776785988605,21.3459786812371,4.0929539746676));
#10529=CARTESIAN_POINT('Ctrl Pts',(-11.4213707289154,21.5842309048223,-1.5632643140974));
#10530=CARTESIAN_POINT('Ctrl Pts',(-9.28060564270375,21.8224831284073,-6.83826580187362));
#10531=CARTESIAN_POINT('Ctrl Pts',(-4.87656776620671,22.0607353519925,-10.4456002501902));
#10532=CARTESIAN_POINT('Ctrl Pts',(0.716726628231168,22.2989875755775,-11.505555789129));
#10533=CARTESIAN_POINT('Ctrl Pts',(6.13523140886729,22.5372397991627,-9.75963257721301));
#10534=CARTESIAN_POINT('Ctrl Pts',(10.0575287120496,22.7754920227477,-5.63361488643787));
#10535=CARTESIAN_POINT('Ctrl Pts',(11.5270819102518,23.0137442463329,-0.133718857131222));
#10536=CARTESIAN_POINT('Ctrl Pts',(10.1855091228218,23.2519964699179,5.39878709595479));
#10537=CARTESIAN_POINT('Ctrl Pts',(6.35998154947282,23.4902486935031,9.61468321854846));
#10538=CARTESIAN_POINT('Ctrl Pts',(0.983436143492576,23.7285009170882,11.4858326467177));
#10539=CARTESIAN_POINT('Ctrl Pts',(-4.63294125611917,23.9667531406733,10.5559155849508));
#10540=CARTESIAN_POINT('Ctrl Pts',(-9.119476605462,24.2050053642584,7.05171219138697));
#10541=CARTESIAN_POINT('Ctrl Pts',(-11.3820320820593,24.4432575878435,1.82779761342809));
#10542=CARTESIAN_POINT('Ctrl Pts',(-10.868835025435,24.6815098114285,-3.84186460145004));
#10543=CARTESIAN_POINT('Ctrl Pts',(-7.70503954112062,24.9197620350137,-8.57460576880672));
#10544=CARTESIAN_POINT('Ctrl Pts',(-2.66220498308041,25.1580142585987,-11.216245497271));
#10545=CARTESIAN_POINT('Ctrl Pts',(3.02986533259278,25.3962664821839,-11.1225633056928));
#10546=CARTESIAN_POINT('Ctrl Pts',(7.98303803241107,25.6345187057689,-8.31640560566758));
#10547=CARTESIAN_POINT('Ctrl Pts',(10.9893757668322,25.8727709293541,-3.48211411063157));
#10548=CARTESIAN_POINT('Ctrl Pts',(11.3157186291889,26.1110231529392,2.20136556012525));
#10549=CARTESIAN_POINT('Ctrl Pts',(8.88248091630454,26.3492753765243,7.34799504598405));
#10550=CARTESIAN_POINT('Ctrl Pts',(4.28305980846921,26.5875276001094,10.702658412811));
#10551=CARTESIAN_POINT('Ctrl Pts',(-1.3608772543271,26.8257798236945,11.4472490810218));
#10552=CARTESIAN_POINT('Ctrl Pts',(-6.67293522403238,27.0640320472796,9.4001826535517));
#10553=CARTESIAN_POINT('Ctrl Pts',(-10.3576548843057,27.3022842708646,5.06068016396008));
#10554=CARTESIAN_POINT('Ctrl Pts',(-11.5164383526005,27.5405364944498,-0.512977674981265));
#10555=CARTESIAN_POINT('Ctrl Pts',(-9.86669143805761,27.7787887180349,-5.96153491061126));
#10556=CARTESIAN_POINT('Ctrl Pts',(-5.8107402932274,28.0170409416199,-9.95624405430786));
#10557=CARTESIAN_POINT('Ctrl Pts',(-0.337715556662699,28.2552931652051,
-11.5229096424065));
#10558=CARTESIAN_POINT('Ctrl Pts',(5.21766835837407,28.4935453887901,-10.2794666849161));
#10559=CARTESIAN_POINT('Ctrl Pts',(9.50061198732568,28.7317976123753,-6.52915540407486));
#10560=CARTESIAN_POINT('Ctrl Pts',(11.4666277080989,28.9700498359604,-1.1865696052641));
#10561=CARTESIAN_POINT('Ctrl Pts',(10.6362604395415,29.2083020595455,4.44538662958811));
#10562=CARTESIAN_POINT('Ctrl Pts',(7.21201304158794,29.4465542831306,8.99324003417244));
#10563=CARTESIAN_POINT('Ctrl Pts',(2.02896165158692,29.6848065067157,11.3478990584454));
#10564=CARTESIAN_POINT('Ctrl Pts',(-3.64889553423618,29.9230587303008,10.9351296199225));
#10565=CARTESIAN_POINT('Ctrl Pts',(-8.43689131864875,30.1613109538859,7.85559439518017));
#10566=CARTESIAN_POINT('Ctrl Pts',(-11.1673702840897,30.3995631774709,2.86030406815548));
#10567=CARTESIAN_POINT('Ctrl Pts',(-11.1744465985554,30.6378154010561,-2.83253272537331));
#10568=CARTESIAN_POINT('Ctrl Pts',(-8.45639455106058,30.8760676246412,-7.83459568970025));
#10569=CARTESIAN_POINT('Ctrl Pts',(-3.67606940325828,31.1143198482262,-10.9260245362485));
#10570=CARTESIAN_POINT('Ctrl Pts',(2.00074407647172,31.3525720718114,-11.3529080664269));
#10571=CARTESIAN_POINT('Ctrl Pts',(7.18963322100266,31.5908242953965,-9.01114157982946));
#10572=CARTESIAN_POINT('Ctrl Pts',(10.6251761725167,31.8290765189816,-4.47181503723706));
#10573=CARTESIAN_POINT('Ctrl Pts',(11.4695421307741,32.0673287425667,1.15805946940319));
#10574=CARTESIAN_POINT('Ctrl Pts',(9.51681435525202,32.3055809661518,6.50551634783486));
#10575=CARTESIAN_POINT('Ctrl Pts',(5.24320737678452,32.5438331897369,10.2664635989375));
#10576=CARTESIAN_POINT('Ctrl Pts',(-0.309068124915233,32.782085413322,11.5237136079667));
#10577=CARTESIAN_POINT('Ctrl Pts',(-5.78597073852161,33.020337636907,9.97065900716958));
#10578=CARTESIAN_POINT('Ctrl Pts',(-9.85184034731961,33.2585898604922,5.98604545548992));
#10579=CARTESIAN_POINT('Ctrl Pts',(-11.515127482688,33.4968420840773,0.541606390048691));
#10580=CARTESIAN_POINT('Ctrl Pts',(-10.3702039189452,33.7350943076624,-5.03491500461833));
#10581=CARTESIAN_POINT('Ctrl Pts',(-6.69628381210821,33.9733465312475,-9.38356443639719));
#10582=CARTESIAN_POINT('Ctrl Pts',(-1.3893313420703,34.2115987548326,-11.4438305145706));
#10583=CARTESIAN_POINT('Ctrl Pts',(4.25643936032185,34.4498509784177,-10.7132731877799));
#10584=CARTESIAN_POINT('Ctrl Pts',(8.8641860747949,34.6881032020028,-7.37005452193625));
#10585=CARTESIAN_POINT('Ctrl Pts',(11.3102109834865,34.9263554255879,-2.22949006093621));
#10586=CARTESIAN_POINT('Ctrl Pts',(10.9979984746946,35.164607649173,3.45478334741955));
#10587=CARTESIAN_POINT('Ctrl Pts',(8.00368826111052,35.4028598727581,8.29653377258524));
#10588=CARTESIAN_POINT('Ctrl Pts',(3.05750708228506,35.6411120963432,11.114996575248));
#10589=CARTESIAN_POINT('Ctrl Pts',(-2.63431274790397,35.8793643199283,11.2228291789063));
#10590=CARTESIAN_POINT('Ctrl Pts',(-7.68369893542883,36.1176165435133,8.59373429059882));
#10591=CARTESIAN_POINT('Ctrl Pts',(-10.8592504225313,36.3558687670984,3.86887306331091));
#10592=CARTESIAN_POINT('Ctrl Pts',(-11.3865408745652,36.5941209906836,-1.79949580399373));
#10593=CARTESIAN_POINT('Ctrl Pts',(-9.13697926434082,36.8323732142686,-7.02901903722545));
#10594=CARTESIAN_POINT('Ctrl Pts',(-4.65916930916454,37.0706254378537,-10.544365298446));
#10595=CARTESIAN_POINT('Ctrl Pts',(0.954878821536958,37.3088776614389,-11.4882420123614));
#10596=CARTESIAN_POINT('Ctrl Pts',(6.33605957035795,37.547129885024,-9.63046466185671));
#10597=CARTESIAN_POINT('Ctrl Pts',(10.1720557787132,37.7853821086091,-5.42409197168482));
#10598=CARTESIAN_POINT('Ctrl Pts',(11.5273792823635,38.0236343321941,0.105061681464705));
#10599=CARTESIAN_POINT('Ctrl Pts',(10.0715018815638,38.2618865557793,5.60859408540474));
#10600=CARTESIAN_POINT('Ctrl Pts',(6.15947753255868,38.5001387793643,9.74434999363035));
#10601=CARTESIAN_POINT('Ctrl Pts',(0.74532310706011,38.7383910029495,11.5037384405739));
#10602=CARTESIAN_POINT('Ctrl Pts',(-4.85057540333342,38.9766432265345,10.4576912719547));
#10603=CARTESIAN_POINT('Ctrl Pts',(-9.26359511660826,39.2148954501196,6.86131666781508));
#10604=CARTESIAN_POINT('Ctrl Pts',(-11.4174122888469,39.4531476737047,1.59165331752844));
#10605=CARTESIAN_POINT('Ctrl Pts',(-10.7870018243007,39.6913998972899,-4.06614957446744));
#10606=CARTESIAN_POINT('Ctrl Pts',(-7.52564218816163,39.929652120875,-8.73237343455133));
#10607=CARTESIAN_POINT('Ctrl Pts',(-2.42961335525277,40.1679043444601,-11.268941774455));
#10608=CARTESIAN_POINT('Ctrl Pts',(3.26020547128437,40.4061565680452,-11.0575098390168));
#10609=CARTESIAN_POINT('Ctrl Pts',(6.52122388891844,40.5649913837685,-9.11833232786835));
#10610=CARTESIAN_POINT('Ctrl Pts',(7.82149843786967,40.6444087916303,-7.81737130740481));
#10611=CARTESIAN_POINT('Ctrl Pts',(8.77586558817396,19.3557191955389,-7.61148460631401));
#10612=CARTESIAN_POINT('Ctrl Pts',(10.0422262020691,19.4351571472829,-6.15140752910658));
#10613=CARTESIAN_POINT('Ctrl Pts',(11.8304967747464,19.5940125068886,-2.58882707902948));
#10614=CARTESIAN_POINT('Ctrl Pts',(11.6260496541463,19.832285274356,3.38948536637273));
#10615=CARTESIAN_POINT('Ctrl Pts',(8.58663531759557,20.0705374979411,8.53935886889055));
#10616=CARTESIAN_POINT('Ctrl Pts',(3.45305662793327,20.3087897215262,11.6073703660148));
#10617=CARTESIAN_POINT('Ctrl Pts',(-2.52256036032647,20.5470419451113,11.8443564246056));
#10618=CARTESIAN_POINT('Ctrl Pts',(-7.8830285512691,20.7852941686964,9.1930012492232));
#10619=CARTESIAN_POINT('Ctrl Pts',(-11.3210354807218,21.0235463922815,4.29965642977116));
#10620=CARTESIAN_POINT('Ctrl Pts',(-11.9981730543084,21.2617986158666,-1.64221232418978));
#10621=CARTESIAN_POINT('Ctrl Pts',(-9.74929500082207,21.5000508394517,-7.18361205757219));
#10622=CARTESIAN_POINT('Ctrl Pts',(-5.12284430290676,21.7383030630368,-10.973124192582));
#10623=CARTESIAN_POINT('Ctrl Pts',(0.752922772778707,21.9765552866219,-12.0866096303556));
#10624=CARTESIAN_POINT('Ctrl Pts',(6.44507300559435,22.214807510207,-10.2525137645179));
#10625=CARTESIAN_POINT('Ctrl Pts',(10.5654542567593,22.4530597337921,-5.91812383409328));
#10626=CARTESIAN_POINT('Ctrl Pts',(12.1092228641389,22.6913119573772,-0.140471929907933));
#10627=CARTESIAN_POINT('Ctrl Pts',(10.6998979371592,22.9295641809623,5.67143676517222));
#10628=CARTESIAN_POINT('Ctrl Pts',(6.6811734829336,23.1678164045474,10.1002441700318));
#10629=CARTESIAN_POINT('Ctrl Pts',(1.03310165807095,23.4060686281325,12.0658904293558));
#10630=CARTESIAN_POINT('Ctrl Pts',(-4.86691416124282,23.6443208517176,11.089010674898));
#10631=CARTESIAN_POINT('Ctrl Pts',(-9.5800286212617,23.8825730753027,7.40783792152343));
#10632=CARTESIAN_POINT('Ctrl Pts',(-11.9568477262104,24.1208252988878,1.92010509024469));
#10633=CARTESIAN_POINT('Ctrl Pts',(-11.4177331801119,24.3590775224729,-4.03588653529299));
#10634=CARTESIAN_POINT('Ctrl Pts',(-8.09415962399401,24.597329746058,-9.00764070516989));
#10635=CARTESIAN_POINT('Ctrl Pts',(-2.79665171993538,24.8355819696431,-11.7826885835309));
#10636=CARTESIAN_POINT('Ctrl Pts',(3.18287966081545,25.0738341932282,-11.6842752517741));
#10637=CARTESIAN_POINT('Ctrl Pts',(8.38619760144056,25.3120864168133,-8.73640091149512));
#10638=CARTESIAN_POINT('Ctrl Pts',(11.5443614727842,25.5503386403984,-3.65796791697122));
#10639=CARTESIAN_POINT('Ctrl Pts',(11.8871853098286,25.7885908639836,2.3125389739175));
#10640=CARTESIAN_POINT('Ctrl Pts',(9.33106417039787,26.0268430875686,7.71908365960987));
#10641=CARTESIAN_POINT('Ctrl Pts',(4.49936299273306,26.2650953111537,11.2431643124021));
#10642=CARTESIAN_POINT('Ctrl Pts',(-1.42960430850484,26.5033475347388,12.0253583155439));
#10643=CARTESIAN_POINT('Ctrl Pts',(-7.00993195111298,26.7415997583239,9.87491089260278));
#10644=CARTESIAN_POINT('Ctrl Pts',(-10.880737407821,26.979851981909,5.31625474917623));
#10645=CARTESIAN_POINT('Ctrl Pts',(-12.098041785296,27.2181042054941,-0.538884085238557));
#10646=CARTESIAN_POINT('Ctrl Pts',(-10.3649793143979,27.4563564290792,-6.26260448281651));
#10647=CARTESIAN_POINT('Ctrl Pts',(-6.10419443222168,27.6946086526643,-10.4590545189192));
#10648=CARTESIAN_POINT('Ctrl Pts',(-0.354770875418026,27.9328608762494,
-12.1048398883276));
#10649=CARTESIAN_POINT('Ctrl Pts',(5.4811711649698,28.1711130998345,-10.7986005462002));
#10650=CARTESIAN_POINT('Ctrl Pts',(9.98041211088462,28.4093653234196,-6.85889095940433));
#10651=CARTESIAN_POINT('Ctrl Pts',(12.0457156024881,28.6476175470047,-1.24649377056803));
#10652=CARTESIAN_POINT('Ctrl Pts',(11.1734131071702,28.8858697705898,4.66988764667932));
#10653=CARTESIAN_POINT('Ctrl Pts',(7.57623428892219,29.1241219941749,9.44741684776587));
#10654=CARTESIAN_POINT('Ctrl Pts',(2.13142831925279,29.36237421776,11.9209909158584));
#10655=CARTESIAN_POINT('Ctrl Pts',(-3.83317213983967,29.6006264413451,11.4873757857244));
#10656=CARTESIAN_POINT('Ctrl Pts',(-8.86297139670491,29.8388786649302,8.25231780273166));
#10657=CARTESIAN_POINT('Ctrl Pts',(-11.7313450732173,30.0771308885153,3.00475520952911));
#10658=CARTESIAN_POINT('Ctrl Pts',(-11.7387787558777,30.3153831121004,-2.97558135775951));
#10659=CARTESIAN_POINT('Ctrl Pts',(-8.88345958180541,30.5536353356855,-8.23025862014802));
#10660=CARTESIAN_POINT('Ctrl Pts',(-3.86171834421572,30.7918875592706,-11.4778108769068));
#10661=CARTESIAN_POINT('Ctrl Pts',(2.10178569951469,31.0301397828557,-11.9262528888754));
#10662=CARTESIAN_POINT('Ctrl Pts',(7.55272424212662,31.2683920064408,-9.46622245769049));
#10663=CARTESIAN_POINT('Ctrl Pts',(11.1617690622389,31.5066442300259,-4.69765074237494));
#10664=CARTESIAN_POINT('Ctrl Pts',(12.0487772094039,31.744896453611,1.21654381517477));
#10665=CARTESIAN_POINT('Ctrl Pts',(9.99743273116598,31.9831486771961,6.83405808300622));
#10666=CARTESIAN_POINT('Ctrl Pts',(5.50799995547129,32.2214009007812,10.7849407780765));
#10667=CARTESIAN_POINT('Ctrl Pts',(-0.324676690418206,32.4596531243664,
12.1056844557749));
#10668=CARTESIAN_POINT('Ctrl Pts',(-6.07817396489844,32.6979053479514,10.4741974560597));
#10669=CARTESIAN_POINT('Ctrl Pts',(-10.3493782135363,32.9361575715365,6.28835285979241));
#10670=CARTESIAN_POINT('Ctrl Pts',(-12.0966647138013,33.1744097951216,0.568958608328141));
#10671=CARTESIAN_POINT('Ctrl Pts',(-10.8939201940946,33.4126620187067,-5.28918839716898));
#10672=CARTESIAN_POINT('Ctrl Pts',(-7.03445969011705,33.6509142422919,-9.85745342186599));
#10673=CARTESIAN_POINT('Ctrl Pts',(-1.45949538523709,33.8891664658769,-12.0217671045718));
#10674=CARTESIAN_POINT('Ctrl Pts',(4.4713981581054,34.127418689462,-11.2543151549789));
#10675=CARTESIAN_POINT('Ctrl Pts',(9.31184540238453,34.3656709130471,-7.7422571837204));
#10676=CARTESIAN_POINT('Ctrl Pts',(11.8813995168772,34.6039231366322,-2.34208381891072));
#10677=CARTESIAN_POINT('Ctrl Pts',(11.5534196448359,34.8421753602173,3.62925689493129));
#10678=CARTESIAN_POINT('Ctrl Pts',(8.4078907084614,35.0804275838025,8.71552551064461));
#10679=CARTESIAN_POINT('Ctrl Pts',(3.21191737478198,35.3186798073875,11.6763263861354));
#10680=CARTESIAN_POINT('Ctrl Pts',(-2.76735087046106,35.5569320309727,11.7896047544065));
#10681=CARTESIAN_POINT('Ctrl Pts',(-8.07174127454621,35.7951842545577,9.0277352560064));
#10682=CARTESIAN_POINT('Ctrl Pts',(-11.4076645353736,36.0334364781429,4.06425897911157));
#10683=CARTESIAN_POINT('Ctrl Pts',(-11.9615842218583,36.2716887017279,-1.89037398218391));
#10684=CARTESIAN_POINT('Ctrl Pts',(-9.59841519981894,36.5099409253131,-7.38399871717217));
#10685=CARTESIAN_POINT('Ctrl Pts',(-4.89446678402209,36.7481931488981,-11.0768770755603));
#10686=CARTESIAN_POINT('Ctrl Pts',(1.00310213358974,36.9864453724833,-12.0684214728383));
#10687=CARTESIAN_POINT('Ctrl Pts',(6.65604339548311,37.2246975960683,-10.1168226081503));
#10688=CARTESIAN_POINT('Ctrl Pts',(10.6857651719592,37.4629498196534,-5.69801958831428));
#10689=CARTESIAN_POINT('Ctrl Pts',(12.1095352541438,37.7012020432385,0.110367508901437));
#10690=CARTESIAN_POINT('Ctrl Pts',(10.5801330995995,37.9394542668236,5.89183943199493));
#10691=CARTESIAN_POINT('Ctrl Pts',(6.47054360757812,38.1777064904088,10.2364593795502));
#10692=CARTESIAN_POINT('Ctrl Pts',(0.782963431634552,38.4159587139938,12.0847005020222));
#10693=CARTESIAN_POINT('Ctrl Pts',(-5.09553927313002,38.654210937579,10.9858258354038));
#10694=CARTESIAN_POINT('Ctrl Pts',(-9.73142540874922,38.892463161164,7.20782703887185));
#10695=CARTESIAN_POINT('Ctrl Pts',(-11.9940147050091,39.1307153847492,1.67203502972045));
#10696=CARTESIAN_POINT('Ctrl Pts',(-11.3317672367851,39.3689676083343,-4.27149835313993));
#10697=CARTESIAN_POINT('Ctrl Pts',(-7.90570234181881,39.6072198319193,-9.17337595717302));
#10698=CARTESIAN_POINT('Ctrl Pts',(-2.55231374440726,39.8454720555045,-11.8380461293086));
#10699=CARTESIAN_POINT('Ctrl Pts',(3.42485244245177,40.0837242790895,-11.6159364534383));
#10700=CARTESIAN_POINT('Ctrl Pts',(6.85055888668833,40.2425590948129,-9.57882655533488));
#10701=CARTESIAN_POINT('Ctrl Pts',(8.21649993060639,40.3219765026746,-8.21216437170453));
#10702=CARTESIAN_POINT('Ctrl Pts',(9.19775812595308,19.0332869065834,-7.9774004837349));
#10703=CARTESIAN_POINT('Ctrl Pts',(10.5249979873448,19.1127248583274,-6.44713139899647));
#10704=CARTESIAN_POINT('Ctrl Pts',(12.3992382005735,19.2715802179331,-2.71328281678768));
#10705=CARTESIAN_POINT('Ctrl Pts',(12.1849624523942,19.5098529854005,3.5524320943754));
#10706=CARTESIAN_POINT('Ctrl Pts',(8.9994307653752,19.7481052089856,8.9498815401878));
#10707=CARTESIAN_POINT('Ctrl Pts',(3.61905949217688,19.9863574325707,12.1653851728116));
#10708=CARTESIAN_POINT('Ctrl Pts',(-2.64383037995317,20.2246096561558,12.4137641417282));
#10709=CARTESIAN_POINT('Ctrl Pts',(-8.26199868104885,20.4628618797409,9.63494724165815));
#10710=CARTESIAN_POINT('Ctrl Pts',(-11.8652849728387,20.701114103326,4.50635888487473));
#10711=CARTESIAN_POINT('Ctrl Pts',(-12.5749753797014,20.9393663269111,-1.72116033428216));
#10712=CARTESIAN_POINT('Ctrl Pts',(-10.2179843589404,21.1776185504962,-7.52895831327076));
#10713=CARTESIAN_POINT('Ctrl Pts',(-5.36912083960681,21.4158707740812,-11.5006481349737));
#10714=CARTESIAN_POINT('Ctrl Pts',(0.789118917326245,21.6541229976664,-12.6676634715821));
#10715=CARTESIAN_POINT('Ctrl Pts',(6.7549146023214,21.8923752212515,-10.7453949518229));
#10716=CARTESIAN_POINT('Ctrl Pts',(11.0733798014692,22.1306274448366,-6.20263278174869));
#10717=CARTESIAN_POINT('Ctrl Pts',(12.6913638180259,22.3688796684217,-0.147225002684643));
#10718=CARTESIAN_POINT('Ctrl Pts',(11.2142867514966,22.6071318920068,5.94408643438964));
#10719=CARTESIAN_POINT('Ctrl Pts',(7.00236541639435,22.8453841155919,10.585805121515));
#10720=CARTESIAN_POINT('Ctrl Pts',(1.08276717264934,23.083636339177,12.6459482119938));
#10721=CARTESIAN_POINT('Ctrl Pts',(-5.10088706636649,23.3218885627621,11.6221057648453));
#10722=CARTESIAN_POINT('Ctrl Pts',(-10.0405806370614,23.5601407863472,7.76396365165987));
#10723=CARTESIAN_POINT('Ctrl Pts',(-12.5316633703614,23.7983930099322,2.01241256706129));
#10724=CARTESIAN_POINT('Ctrl Pts',(-11.966631334789,24.0366452335174,-4.22990846913595));
#10725=CARTESIAN_POINT('Ctrl Pts',(-8.48327970686742,24.2748974571024,-9.44067564153303));
#10726=CARTESIAN_POINT('Ctrl Pts',(-2.93109845679036,24.5131496806876,-12.3491316697907));
#10727=CARTESIAN_POINT('Ctrl Pts',(3.33589398903813,24.7514019042726,-12.2459871978553));
#10728=CARTESIAN_POINT('Ctrl Pts',(8.78935717047004,24.9896541278578,-9.15639621732265));
#10729=CARTESIAN_POINT('Ctrl Pts',(12.0993471787362,25.2279063514429,-3.83382172331087));
#10730=CARTESIAN_POINT('Ctrl Pts',(12.4586519904683,25.466158575028,2.42371238770974));
#10731=CARTESIAN_POINT('Ctrl Pts',(9.77964742449122,25.7044107986131,8.09017227323569));
#10732=CARTESIAN_POINT('Ctrl Pts',(4.71566617699691,25.9426630221981,11.7836702119933));
#10733=CARTESIAN_POINT('Ctrl Pts',(-1.49833136268259,26.1809152457833,12.603467550066));
#10734=CARTESIAN_POINT('Ctrl Pts',(-7.34692867819359,26.4191674693684,10.3496391316539));
#10735=CARTESIAN_POINT('Ctrl Pts',(-11.4038199313364,26.6574196929535,5.57182933439236));
#10736=CARTESIAN_POINT('Ctrl Pts',(-12.6796452179915,26.8956719165386,-0.564790495495845));
#10737=CARTESIAN_POINT('Ctrl Pts',(-10.8632671907382,27.1339241401237,-6.56367405502175));
#10738=CARTESIAN_POINT('Ctrl Pts',(-6.39764857121597,27.3721763637088,-10.9618649835306));
#10739=CARTESIAN_POINT('Ctrl Pts',(-0.371826194173351,27.6104285872939,
-12.6867701342486));
#10740=CARTESIAN_POINT('Ctrl Pts',(5.74467397156553,27.848680810879,-11.3177344074843));
#10741=CARTESIAN_POINT('Ctrl Pts',(10.4602122344436,28.0869330344641,-7.1886265147338));
#10742=CARTESIAN_POINT('Ctrl Pts',(12.6248034968774,28.3251852580492,-1.30641793587195));
#10743=CARTESIAN_POINT('Ctrl Pts',(11.7105657747989,28.5634374816343,4.89438866377053));
#10744=CARTESIAN_POINT('Ctrl Pts',(7.94045553625644,28.8016897052194,9.90159366135931));
#10745=CARTESIAN_POINT('Ctrl Pts',(2.23389498691868,29.0399419288045,12.4940827732714));
#10746=CARTESIAN_POINT('Ctrl Pts',(-4.01744874544316,29.2781941523896,12.0396219515263));
#10747=CARTESIAN_POINT('Ctrl Pts',(-9.28905147476106,29.5164463759747,8.64904121028314));
#10748=CARTESIAN_POINT('Ctrl Pts',(-12.2953198623448,29.7546985995598,3.14920635090273));
#10749=CARTESIAN_POINT('Ctrl Pts',(-12.3031109132,29.9929508231448,-3.1186299901457));
#10750=CARTESIAN_POINT('Ctrl Pts',(-9.31052461255024,30.23120304673,-8.6259215505958));
#10751=CARTESIAN_POINT('Ctrl Pts',(-4.04736728517316,30.4694552703151,-12.0295972175649));
#10752=CARTESIAN_POINT('Ctrl Pts',(2.20282732255767,30.7077074939002,-12.4995977113237));
#10753=CARTESIAN_POINT('Ctrl Pts',(7.91581526325055,30.9459597174853,-9.92130333555153));
#10754=CARTESIAN_POINT('Ctrl Pts',(11.6983619519613,31.1842119410704,-4.92348644751282));
#10755=CARTESIAN_POINT('Ctrl Pts',(12.6280122880337,31.4224641646555,1.27502816094633));
#10756=CARTESIAN_POINT('Ctrl Pts',(10.47805110708,31.6607163882406,7.16259981817759));
#10757=CARTESIAN_POINT('Ctrl Pts',(5.77279253415804,31.8989686118257,11.3034179572156));
#10758=CARTESIAN_POINT('Ctrl Pts',(-0.340285255921168,32.1372208354108,
12.687655303583));
#10759=CARTESIAN_POINT('Ctrl Pts',(-6.37037719127529,32.3754730589959,10.9777359049497));
#10760=CARTESIAN_POINT('Ctrl Pts',(-10.846916079753,32.613725282581,6.59066026409488));
#10761=CARTESIAN_POINT('Ctrl Pts',(-12.6782019449145,32.8519775061661,0.596310826607595));
#10762=CARTESIAN_POINT('Ctrl Pts',(-11.4176364692439,33.0902297297512,-5.54346178971963));
#10763=CARTESIAN_POINT('Ctrl Pts',(-7.3726355681259,33.3284819533363,-10.3313424073348));
#10764=CARTESIAN_POINT('Ctrl Pts',(-1.52965942840387,33.5667341769214,-12.5997036945729));
#10765=CARTESIAN_POINT('Ctrl Pts',(4.68635695588896,33.8049864005065,-11.7953571221779));
#10766=CARTESIAN_POINT('Ctrl Pts',(9.75950472997414,34.0432386240916,-8.11445984550458));
#10767=CARTESIAN_POINT('Ctrl Pts',(12.4525880502679,34.2814908476767,-2.45467757688521));
#10768=CARTESIAN_POINT('Ctrl Pts',(12.1088408149773,34.5197430712618,3.80373044244303));
#10769=CARTESIAN_POINT('Ctrl Pts',(8.81209315581226,34.7579952948469,9.13451724870399));
#10770=CARTESIAN_POINT('Ctrl Pts',(3.3663276672789,34.996247518432,12.237656197023));
#10771=CARTESIAN_POINT('Ctrl Pts',(-2.90038899301814,35.2344997420171,12.3563803299066));
#10772=CARTESIAN_POINT('Ctrl Pts',(-8.45978361366359,35.4727519656022,9.46173622141396));
#10773=CARTESIAN_POINT('Ctrl Pts',(-11.9560786482159,35.7110041891873,4.25964489491223));
#10774=CARTESIAN_POINT('Ctrl Pts',(-12.5366275691515,35.9492564127724,-1.98125216037409));
#10775=CARTESIAN_POINT('Ctrl Pts',(-10.0598511352971,36.1875086363575,-7.7389783971189));
#10776=CARTESIAN_POINT('Ctrl Pts',(-5.12976425887965,36.4257608599426,-11.6093888526747));
#10777=CARTESIAN_POINT('Ctrl Pts',(1.05132544564253,36.6640130835277,-12.648600933315));
#10778=CARTESIAN_POINT('Ctrl Pts',(6.97602722060828,36.9022653071128,-10.6031805544441));
#10779=CARTESIAN_POINT('Ctrl Pts',(11.1994745652053,37.1405175306979,-5.97194720494374));
#10780=CARTESIAN_POINT('Ctrl Pts',(12.6916912259241,37.378769754283,0.115673336338169));
#10781=CARTESIAN_POINT('Ctrl Pts',(11.0887643176353,37.6170219778681,6.17508477858514));
#10782=CARTESIAN_POINT('Ctrl Pts',(6.78160968259758,37.8552742014532,10.7285687654699));
#10783=CARTESIAN_POINT('Ctrl Pts',(0.820603756208998,38.0935264250383,12.6656625634705));
#10784=CARTESIAN_POINT('Ctrl Pts',(-5.34050314292663,38.3317786486234,11.5139603988529));
#10785=CARTESIAN_POINT('Ctrl Pts',(-10.1992557008902,38.5700308722085,7.55433740992864));
#10786=CARTESIAN_POINT('Ctrl Pts',(-12.5706171211714,38.8082830957936,1.75241674191245));
#10787=CARTESIAN_POINT('Ctrl Pts',(-11.8765326492695,39.0465353193787,-4.47684713181242));
#10788=CARTESIAN_POINT('Ctrl Pts',(-8.28576249547599,39.2847875429638,-9.61437847979471));
#10789=CARTESIAN_POINT('Ctrl Pts',(-2.67501413356175,39.5230397665489,-12.4071504841623));
#10790=CARTESIAN_POINT('Ctrl Pts',(3.58949941361916,39.761291990134,-12.1743630678598));
#10791=CARTESIAN_POINT('Ctrl Pts',(7.17989388445823,39.9201268058574,-10.0393207828014));
#10792=CARTESIAN_POINT('Ctrl Pts',(8.61150142334309,39.9995442137191,-8.60695743600425));
#10793=CARTESIAN_POINT('',(-9.92496439632576,40.0002541663958,-3.43141021993915));
#10794=CARTESIAN_POINT('Ctrl Pts',(8.61094305413662,40.,-8.60639936142963));
#10795=CARTESIAN_POINT('Ctrl Pts',(8.39826176691632,40.,-8.79212327549388));
#10796=CARTESIAN_POINT('Ctrl Pts',(8.17937308111424,40.,-8.96994937667224));
#10797=CARTESIAN_POINT('Ctrl Pts',(7.95478109509821,40.,-9.13970638711401));
#10798=CARTESIAN_POINT('Ctrl Pts',(7.72804274042583,40.,-9.31108572225611));
#10799=CARTESIAN_POINT('Ctrl Pts',(7.49549100836207,40.,-9.4742413025714));
#10800=CARTESIAN_POINT('Ctrl Pts',(7.2576130834412,40.,-9.628954303971));
#10801=CARTESIAN_POINT('Ctrl Pts',(7.01927567556664,40.,-9.78396614767336));
#10802=CARTESIAN_POINT('Ctrl Pts',(6.77559089375214,40.,-9.93050302185609));
#10803=CARTESIAN_POINT('Ctrl Pts',(6.52702586473483,40.,-10.06829815855));
#10804=CARTESIAN_POINT('Ctrl Pts',(6.27982630250056,40.,-10.2053363316325));
#10805=CARTESIAN_POINT('Ctrl Pts',(6.02779937924827,40.,-10.3337287424236));
#10806=CARTESIAN_POINT('Ctrl Pts',(5.77139073271193,40.,-10.4531635932807));
#10807=CARTESIAN_POINT('Ctrl Pts',(5.51880872753046,40.,-10.5708159990226));
#10808=CARTESIAN_POINT('Ctrl Pts',(5.26197426321313,40.,-10.6797763194938));
#10809=CARTESIAN_POINT('Ctrl Pts',(5.00130823957099,40.,-10.7796963454939));
#10810=CARTESIAN_POINT('Ctrl Pts',(4.90713970256531,40.,-10.8157935803178));
#10811=CARTESIAN_POINT('Ctrl Pts',(4.81247110078974,40.,-10.8507104814013));
#10812=CARTESIAN_POINT('Ctrl Pts',(4.71732232047202,40.,-10.8844289444319));
#10813=CARTESIAN_POINT('Ctrl Pts',(4.68473084450778,40.,-10.8959785877772));
#10814=CARTESIAN_POINT('Ctrl Pts',(4.65208303079231,40.,-10.9073876128803));
#10815=CARTESIAN_POINT('Ctrl Pts',(4.61937968084376,40.,-10.9186552672316));
#10816=CARTESIAN_POINT('Ctrl Pts',(4.59185356383537,40.,-10.9281391510713));
#10817=CARTESIAN_POINT('Ctrl Pts',(4.56428866349076,40.,-10.9375226531726));
#10818=CARTESIAN_POINT('Ctrl Pts',(4.53669821841154,40.,-10.9468011456384));
#10819=CARTESIAN_POINT('Ctrl Pts',(4.27228656872567,40.,-11.0357211138538));
#10820=CARTESIAN_POINT('Ctrl Pts',(4.00522676966766,40.,-11.1151060432447));
#10821=CARTESIAN_POINT('Ctrl Pts',(3.73596790268647,40.,-11.1847326159485));
#10822=CARTESIAN_POINT('Ctrl Pts',(3.59988597511653,40.,-11.2199214969307));
#10823=CARTESIAN_POINT('Ctrl Pts',(3.46324208617,40.,-11.2526170856896));
#10824=CARTESIAN_POINT('Ctrl Pts',(3.3260929489447,40.,-11.2827856394737));
#10825=CARTESIAN_POINT('Ctrl Pts',(3.05396201990355,40.,-11.3426459983151));
#10826=CARTESIAN_POINT('Ctrl Pts',(2.77984200145982,40.,-11.3925606000749));
#10827=CARTESIAN_POINT('Ctrl Pts',(2.5042778621081,40.,-11.4325612835728));
#10828=CARTESIAN_POINT('Ctrl Pts',(2.22869992434682,40.,-11.4725639700375));
#10829=CARTESIAN_POINT('Ctrl Pts',(1.95167706598645,40.,-11.5026516740376));
#10830=CARTESIAN_POINT('Ctrl Pts',(1.67375680737823,40.,-11.5228042109087));
#10831=CARTESIAN_POINT('Ctrl Pts',(1.398642054319,40.,-11.5427533151323));
#10832=CARTESIAN_POINT('Ctrl Pts',(1.12264732111162,40.,-11.5529666784398));
#10833=CARTESIAN_POINT('Ctrl Pts',(0.846315503642963,40.,-11.5533754837982));
#10834=CARTESIAN_POINT('Ctrl Pts',(0.643529263690987,40.,-11.5536754858113));
#10835=CARTESIAN_POINT('Ctrl Pts',(0.440561695111733,40.,-11.5486943579065));
#10836=CARTESIAN_POINT('Ctrl Pts',(0.237634295057578,40.,-11.5383883933861));
#10837=CARTESIAN_POINT('Ctrl Pts',(0.200021572236072,40.,-11.5364781762995));
#10838=CARTESIAN_POINT('Ctrl Pts',(0.162410249405167,40.,-11.5343849868962));
#10839=CARTESIAN_POINT('Ctrl Pts',(0.124801765584846,40.,-11.5321084946763));
#10840=CARTESIAN_POINT('Ctrl Pts',(0.0953789719671696,40.,-11.5303274933182));
#10841=CARTESIAN_POINT('Ctrl Pts',(0.0659671184443719,40.,-11.5284348486951));
#10842=CARTESIAN_POINT('Ctrl Pts',(0.0365696537066474,40.,-11.5264308156415));
#10843=CARTESIAN_POINT('Ctrl Pts',(-0.236604483961971,40.,-11.5078084614291));
#10844=CARTESIAN_POINT('Ctrl Pts',(-0.508615486317793,40.,-11.4795673079924));
#10845=CARTESIAN_POINT('Ctrl Pts',(-0.778950107545348,40.,-11.4417467199426));
#10846=CARTESIAN_POINT('Ctrl Pts',(-1.05191932377349,40.,-11.4035575445037));
#10847=CARTESIAN_POINT('Ctrl Pts',(-1.32317999343784,40.,-11.355601299064));
#10848=CARTESIAN_POINT('Ctrl Pts',(-1.5921940890953,40.,-11.2978654190554));
#10849=CARTESIAN_POINT('Ctrl Pts',(-1.86120818475262,40.,-11.2401295390468));
#10850=CARTESIAN_POINT('Ctrl Pts',(-2.12797635797297,40.,-11.1726139378876));
#10851=CARTESIAN_POINT('Ctrl Pts',(-2.39194108188819,40.,-11.0952540671311));
#10852=CARTESIAN_POINT('Ctrl Pts',(-2.65358663251955,40.,-11.018573874109));
#10853=CARTESIAN_POINT('Ctrl Pts',(-2.91247824429409,40.,-10.9322209570423));
#10854=CARTESIAN_POINT('Ctrl Pts',(-3.16812267150498,40.,-10.8364284814825));
#10855=CARTESIAN_POINT('Ctrl Pts',(-3.42177931939053,40.,-10.7413808463422));
#10856=CARTESIAN_POINT('Ctrl Pts',(-3.67223957309176,40.,-10.6370394684347));
#10857=CARTESIAN_POINT('Ctrl Pts',(-3.91898715115294,40.,-10.5235942862973));
#10858=CARTESIAN_POINT('Ctrl Pts',(-3.96835687438594,40.,-10.5008959591719));
#10859=CARTESIAN_POINT('Ctrl Pts',(-4.01757784425976,40.,-10.4778330708281));
#10860=CARTESIAN_POINT('Ctrl Pts',(-4.06664573143816,40.,-10.4544069809796));
#10861=CARTESIAN_POINT('Ctrl Pts',(-4.10490890648528,40.,-10.43613929863));
#10862=CARTESIAN_POINT('Ctrl Pts',(-4.14308479220665,40.,-10.4176478398036));
#10863=CARTESIAN_POINT('Ctrl Pts',(-4.18113965154256,40.,-10.3989489818942));
#10864=CARTESIAN_POINT('Ctrl Pts',(-4.42108222934683,40.,-10.28104939569));
#10865=CARTESIAN_POINT('Ctrl Pts',(-4.65640472965588,40.,-10.154821243158));
#10866=CARTESIAN_POINT('Ctrl Pts',(-4.88668744403159,40.,-10.0205608401689));
#10867=CARTESIAN_POINT('Ctrl Pts',(-5.11739045524781,40.,-9.88605539393666));
#10868=CARTESIAN_POINT('Ctrl Pts',(-5.34303579544783,40.,-9.74348797347264));
#10869=CARTESIAN_POINT('Ctrl Pts',(-5.56317346295674,40.,-9.59311273009281));
#10870=CARTESIAN_POINT('Ctrl Pts',(-5.78203974193378,40.,-9.4436059676144));
#10871=CARTESIAN_POINT('Ctrl Pts',(-5.99546225346409,40.,-9.28638090254399));
#10872=CARTESIAN_POINT('Ctrl Pts',(-6.2029636998557,40.,-9.12164999441353));
#10873=CARTESIAN_POINT('Ctrl Pts',(-6.40709362068619,40.,-8.95959566746902));
#10874=CARTESIAN_POINT('Ctrl Pts',(-6.6054936866607,40.,-8.79027700894159));
#10875=CARTESIAN_POINT('Ctrl Pts',(-6.79766944482237,40.,-8.61386626430386));
#10876=CARTESIAN_POINT('Ctrl Pts',(-6.91421310725171,40.,-8.50688318553972));
#10877=CARTESIAN_POINT('Ctrl Pts',(-7.02846683556768,40.,-8.39729127275609));
#10878=CARTESIAN_POINT('Ctrl Pts',(-7.1403121407595,40.,-8.28512438529733));
#10879=CARTESIAN_POINT('Ctrl Pts',(-7.2322458360855,40.,-8.19292635839208));
#10880=CARTESIAN_POINT('Ctrl Pts',(-7.32255217347813,40.,-8.09898847748874));
#10881=CARTESIAN_POINT('Ctrl Pts',(-7.41118873118237,40.,-8.00335941612173));
#10882=CARTESIAN_POINT('Ctrl Pts',(-7.44595173802253,40.,-7.96585396915354));
#10883=CARTESIAN_POINT('Ctrl Pts',(-7.48045783348702,40.,-7.92808841917705));
#10884=CARTESIAN_POINT('Ctrl Pts',(-7.51470444838488,40.,-7.89006554590154));
#10885=CARTESIAN_POINT('Ctrl Pts',(-7.54132180621626,40.,-7.86051318206149));
#10886=CARTESIAN_POINT('Ctrl Pts',(-7.56778132931981,40.,-7.83080646494714));
#10887=CARTESIAN_POINT('Ctrl Pts',(-7.59406823367193,40.,-7.8009624951305));
#10888=CARTESIAN_POINT('Ctrl Pts',(-7.76810920210893,40.,-7.60337082213176));
#10889=CARTESIAN_POINT('Ctrl Pts',(-7.93474819741371,40.,-7.39958702375726));
#10890=CARTESIAN_POINT('Ctrl Pts',(-8.09372374437956,40.,-7.19007656351675));
#10891=CARTESIAN_POINT('Ctrl Pts',(-8.25269853624522,40.,-6.98056709840658));
#10892=CARTESIAN_POINT('Ctrl Pts',(-8.40401024026009,40.,-6.76533042182595));
#10893=CARTESIAN_POINT('Ctrl Pts',(-8.54735114309888,40.,-6.5448081825227));
#10894=CARTESIAN_POINT('Ctrl Pts',(-8.68948029878482,40.,-6.32615015078565));
#10895=CARTESIAN_POINT('Ctrl Pts',(-8.82377305934234,40.,-6.10229494668581));
#10896=CARTESIAN_POINT('Ctrl Pts',(-8.94988036808553,40.,-5.87365868822008));
#10897=CARTESIAN_POINT('Ctrl Pts',(-8.9666093409471,40.,-5.84332856856911));
#10898=CARTESIAN_POINT('Ctrl Pts',(-8.98319419398911,40.,-5.81291429953107));
#10899=CARTESIAN_POINT('Ctrl Pts',(-8.9996340436321,40.,-5.78241684186142));
#10900=CARTESIAN_POINT('Ctrl Pts',(-9.02204332078306,40.,-5.74084553822058));
#10901=CARTESIAN_POINT('Ctrl Pts',(-9.04417775820945,40.,-5.69912961527342));
#10902=CARTESIAN_POINT('Ctrl Pts',(-9.06603067483243,40.,-5.65728118478675));
#10903=CARTESIAN_POINT('Ctrl Pts',(-9.18590518867724,40.,-5.42772096880703));
#10904=CARTESIAN_POINT('Ctrl Pts',(-9.2973605568515,40.,-5.1940857613916));
#10905=CARTESIAN_POINT('Ctrl Pts',(-9.40010767792124,40.,-4.95680439652004));
#10906=CARTESIAN_POINT('Ctrl Pts',(-9.50150771815981,40.,-4.7226339429313));
#10907=CARTESIAN_POINT('Ctrl Pts',(-9.59442650170164,40.,-4.48491173585104));
#10908=CARTESIAN_POINT('Ctrl Pts',(-9.67853712541855,40.,-4.24403874401865));
#10909=CARTESIAN_POINT('Ctrl Pts',(-9.73985884517572,40.,-4.06842779917617));
#10910=CARTESIAN_POINT('Ctrl Pts',(-9.79649777669627,40.,-3.89114186081739));
#10911=CARTESIAN_POINT('Ctrl Pts',(-9.84830976294177,40.,-3.71233506504282));
#10912=CARTESIAN_POINT('Ctrl Pts',(-9.87531187063298,40.,-3.6191488989586));
#10913=CARTESIAN_POINT('Ctrl Pts',(-9.90100270302723,40.,-3.52554965431835));
#10914=CARTESIAN_POINT('Ctrl Pts',(-9.92537747903998,40.,-3.43156570488038));
#10915=CARTESIAN_POINT('Ctrl Pts',(-9.9245821948243,40.0002541663958,-3.43127807940082));
#10916=CARTESIAN_POINT('Ctrl Pts',(-9.92574247154754,40.0001694442638,-3.42792211073779));
#10917=CARTESIAN_POINT('Ctrl Pts',(-9.92690104605405,40.0000847221319,-3.42456555355841));
#10918=CARTESIAN_POINT('Ctrl Pts',(-9.92805791774767,39.9999999999999,-3.42120840958977));
#10919=CARTESIAN_POINT('Ctrl Pts',(7.93381306740072,20.,-6.87936125025729));
#10920=CARTESIAN_POINT('Ctrl Pts',(8.11334533077575,20.,-6.70251189458677));
#10921=CARTESIAN_POINT('Ctrl Pts',(8.28605380477994,20.,-6.51937440106475));
#10922=CARTESIAN_POINT('Ctrl Pts',(8.45179833248054,20.,-6.33047258793705));
#10923=CARTESIAN_POINT('Ctrl Pts',(8.62014953567792,20.,-6.13859990310451));
#10924=CARTESIAN_POINT('Ctrl Pts',(8.78131641961311,20.,-5.94077982210926));
#10925=CARTESIAN_POINT('Ctrl Pts',(8.9351278146894,20.,-5.73751337470593));
#10926=CARTESIAN_POINT('Ctrl Pts',(9.0913599031574,20.,-5.53104790719269));
#10927=CARTESIAN_POINT('Ctrl Pts',(9.24000360361905,20.,-5.31896290747305));
#10928=CARTESIAN_POINT('Ctrl Pts',(9.38084825717968,20.,-5.10173994365898));
#10929=CARTESIAN_POINT('Ctrl Pts',(9.52214874513409,20.,-4.88381395210817));
#10930=CARTESIAN_POINT('Ctrl Pts',(9.65560002896776,20.,-4.66071618702915));
#10931=CARTESIAN_POINT('Ctrl Pts',(9.78095181325634,20.,-4.43289630140568));
#10932=CARTESIAN_POINT('Ctrl Pts',(9.90574239039269,20.,-4.20609637852114));
#10933=CARTESIAN_POINT('Ctrl Pts',(10.0225061927535,20.,-3.97461598352399));
#10934=CARTESIAN_POINT('Ctrl Pts',(10.1309533974595,20.,-3.73887036917977));
#10935=CARTESIAN_POINT('Ctrl Pts',(10.1620449658876,20.,-3.67128263448554));
#10936=CARTESIAN_POINT('Ctrl Pts',(10.192452657003,20.,-3.6033441665067));
#10937=CARTESIAN_POINT('Ctrl Pts',(10.22216892119,20.,-3.53506441406799));
#10938=CARTESIAN_POINT('Ctrl Pts',(10.239684090736,20.,-3.49481940100045));
#10939=CARTESIAN_POINT('Ctrl Pts',(10.2569611674518,20.,-3.45445054561043));
#10940=CARTESIAN_POINT('Ctrl Pts',(10.2739835311413,20.,-3.41399615802963));
#10941=CARTESIAN_POINT('Ctrl Pts',(10.3769729884857,20.,-3.16923723382034));
#10942=CARTESIAN_POINT('Ctrl Pts',(10.4707505425509,20.,-2.92110624344397));
#10943=CARTESIAN_POINT('Ctrl Pts',(10.5551246852778,20.,-2.67011766558322));
#10944=CARTESIAN_POINT('Ctrl Pts',(10.5927935636692,20.,-2.55806368895609));
#10945=CARTESIAN_POINT('Ctrl Pts',(10.628587702233,20.,-2.44543962428696));
#10946=CARTESIAN_POINT('Ctrl Pts',(10.6624876486376,20.,-2.33228893760792));
#10947=CARTESIAN_POINT('Ctrl Pts',(10.7376977925035,20.,-2.08125374946669));
#10948=CARTESIAN_POINT('Ctrl Pts',(10.8035876329606,20.,-1.82762824132245));
#10949=CARTESIAN_POINT('Ctrl Pts',(10.8602429504416,20.,-1.57194508022933));
#10950=CARTESIAN_POINT('Ctrl Pts',(10.9173812906677,20.,-1.31408205698315));
#10951=CARTESIAN_POINT('Ctrl Pts',(10.9651271233675,20.,-1.05412557318626));
#10952=CARTESIAN_POINT('Ctrl Pts',(11.0035202228593,20.,-0.792598803439725));
#10953=CARTESIAN_POINT('Ctrl Pts',(11.04208073776,20.,-0.529931630555835));
#10954=CARTESIAN_POINT('Ctrl Pts',(11.0712069012117,20.,-0.265679827708335));
#10955=CARTESIAN_POINT('Ctrl Pts',(11.0908885652408,20.,-0.000359128635273066));
#10956=CARTESIAN_POINT('Ctrl Pts',(11.1054206053252,20.,0.195541534461971));
#10957=CARTESIAN_POINT('Ctrl Pts',(11.1148027799559,19.9999999999999,0.392025269686389));
#10958=CARTESIAN_POINT('Ctrl Pts',(11.1190128627105,20.,0.588886412300436));
#10959=CARTESIAN_POINT('Ctrl Pts',(11.1196345841872,20.,0.617957764914658));
#10960=CARTESIAN_POINT('Ctrl Pts',(11.1201435132142,20.,0.647039404376552));
#10961=CARTESIAN_POINT('Ctrl Pts',(11.1205394628636,20.,0.676124093961359));
#10962=CARTESIAN_POINT('Ctrl Pts',(11.1242136969702,20.,0.946016891253714));
#10963=CARTESIAN_POINT('Ctrl Pts',(11.1181568313559,20.,1.21559421576547));
#10964=CARTESIAN_POINT('Ctrl Pts',(11.1024699155507,20.,1.4843035710275));
#10965=CARTESIAN_POINT('Ctrl Pts',(11.0859047811347,20.,1.76805639051346));
#10966=CARTESIAN_POINT('Ctrl Pts',(11.0586017438614,20.,2.05084190407223));
#10967=CARTESIAN_POINT('Ctrl Pts',(11.0206211947832,20.,2.33203086493943));
#10968=CARTESIAN_POINT('Ctrl Pts',(10.9826406457049,20.,2.61321982580663));
#10969=CARTESIAN_POINT('Ctrl Pts',(10.9339826723985,20.,2.89281305830034));
#10970=CARTESIAN_POINT('Ctrl Pts',(10.87464624646,20.,3.17019109503699));
#10971=CARTESIAN_POINT('Ctrl Pts',(10.8153870220998,20.,3.4472082400973));
#10972=CARTESIAN_POINT('Ctrl Pts',(10.7454772306754,20.,3.72201679033749));
#10973=CARTESIAN_POINT('Ctrl Pts',(10.6652311260161,20.,3.99411127683229));
#10974=CARTESIAN_POINT('Ctrl Pts',(10.5849850213568,20.,4.26620576332708));
#10975=CARTESIAN_POINT('Ctrl Pts',(10.4944023351477,20.,4.53558691968042));
#10976=CARTESIAN_POINT('Ctrl Pts',(10.3937362784269,20.,4.80173496530221));
#10977=CARTESIAN_POINT('Ctrl Pts',(10.3777423329852,20.,4.84402089026791));
#10978=CARTESIAN_POINT('Ctrl Pts',(10.3614937302683,20.,4.88622515835007));
#10979=CARTESIAN_POINT('Ctrl Pts',(10.3449913509334,20.,4.92834563232135));
#10980=CARTESIAN_POINT('Ctrl Pts',(10.3343844651706,20.,4.95541851960774));
#10981=CARTESIAN_POINT('Ctrl Pts',(10.3236726703155,20.,4.98245685781199));
#10982=CARTESIAN_POINT('Ctrl Pts',(10.3128617315938,20.,5.00944653944195));
#10983=CARTESIAN_POINT('Ctrl Pts',(10.2113685957594,20.,5.26282577822009));
#10984=CARTESIAN_POINT('Ctrl Pts',(10.1010260091921,20.,5.51221436662185));
#10985=CARTESIAN_POINT('Ctrl Pts',(9.98219337299342,20.,5.75718786449119));
#10986=CARTESIAN_POINT('Ctrl Pts',(9.86134406368381,20.,6.00631873429003));
#10987=CARTESIAN_POINT('Ctrl Pts',(9.73171400193977,20.,6.25088396566522));
#10988=CARTESIAN_POINT('Ctrl Pts',(9.59362742884161,20.,6.49043373047328));
#10989=CARTESIAN_POINT('Ctrl Pts',(9.45505341266511,20.,6.73082910157132));
#10990=CARTESIAN_POINT('Ctrl Pts',(9.30796286005019,20.,6.9661741367737));
#10991=CARTESIAN_POINT('Ctrl Pts',(9.15263229120085,20.,7.19600189655872));
#10992=CARTESIAN_POINT('Ctrl Pts',(8.99804398992683,20.,7.42473139413262));
#10993=CARTESIAN_POINT('Ctrl Pts',(8.83529395846679,20.,7.64799680126327));
#10994=CARTESIAN_POINT('Ctrl Pts',(8.66460799086994,20.,7.86531682614724));
#10995=CARTESIAN_POINT('Ctrl Pts',(8.55444285882568,20.,8.00558078325092));
#10996=CARTESIAN_POINT('Ctrl Pts',(8.44097088268035,20.,8.14336759877014));
#10997=CARTESIAN_POINT('Ctrl Pts',(8.32424315342715,20.,8.27854145188553));
#10998=CARTESIAN_POINT('Ctrl Pts',(8.23663382474174,20.,8.37999541319385));
#10999=CARTESIAN_POINT('Ctrl Pts',(8.14719031008403,20.,8.47997733921384));
#11000=CARTESIAN_POINT('Ctrl Pts',(8.05595931410645,20.,8.57845490970599));
#11001=CARTESIAN_POINT('Ctrl Pts',(8.01761638595146,20.,8.61984345720345));
#11002=CARTESIAN_POINT('Ctrl Pts',(7.97895769437451,20.,8.66096625350117));
#11003=CARTESIAN_POINT('Ctrl Pts',(7.93998660061812,20.,8.70182079230146));
#11004=CARTESIAN_POINT('Ctrl Pts',(7.91066081913535,20.,8.73256386779547));
#11005=CARTESIAN_POINT('Ctrl Pts',(7.88115851935513,20.,8.76315450964986));
#11006=CARTESIAN_POINT('Ctrl Pts',(7.85149823336609,20.,8.79357447451951));
#11007=CARTESIAN_POINT('Ctrl Pts',(7.65681753608095,20.,8.99324146270702));
#11008=CARTESIAN_POINT('Ctrl Pts',(7.45515097010471,20.,9.18575086315305));
#11009=CARTESIAN_POINT('Ctrl Pts',(7.24701145539745,20.,9.37088205580245));
#11010=CARTESIAN_POINT('Ctrl Pts',(7.03612872419095,20.,9.5584532221537));
#11011=CARTESIAN_POINT('Ctrl Pts',(6.81860092022066,20.,9.73845086260295));
#11012=CARTESIAN_POINT('Ctrl Pts',(6.59491638245657,20.,9.910616184975));
#11013=CARTESIAN_POINT('Ctrl Pts',(6.37323524877219,20.,10.0812395290205));
#11014=CARTESIAN_POINT('Ctrl Pts',(6.14550664682392,20.,10.2441705629266));
#11015=CARTESIAN_POINT('Ctrl Pts',(5.91216887742395,20.,10.399123041683));
#11016=CARTESIAN_POINT('Ctrl Pts',(5.86175766100923,20.,10.4325995892675));
#11017=CARTESIAN_POINT('Ctrl Pts',(5.81108451494134,20.,10.4657035986193));
#11018=CARTESIAN_POINT('Ctrl Pts',(5.76015366565449,20.,10.4984319462714));
#11019=CARTESIAN_POINT('Ctrl Pts',(5.72101534194005,20.,10.5235823744104));
#11020=CARTESIAN_POINT('Ctrl Pts',(5.6817272115307,20.,10.548509349187));
#11021=CARTESIAN_POINT('Ctrl Pts',(5.64230701889093,20.,10.5732018577602));
#11022=CARTESIAN_POINT('Ctrl Pts',(5.39975652942212,20.,10.7251336378856));
#11023=CARTESIAN_POINT('Ctrl Pts',(5.1520474982564,20.,10.8682962685956));
#11024=CARTESIAN_POINT('Ctrl Pts',(4.89968271153781,20.,11.0024328305905));
#11025=CARTESIAN_POINT('Ctrl Pts',(4.64696653025092,20.,11.1367561653119));
#11026=CARTESIAN_POINT('Ctrl Pts',(4.38958112307547,20.,11.2620286878548));
#11027=CARTESIAN_POINT('Ctrl Pts',(4.12799552824453,20.,11.3779546569627));
#11028=CARTESIAN_POINT('Ctrl Pts',(3.90990991980607,20.,11.474602889917));
#11029=CARTESIAN_POINT('Ctrl Pts',(3.6889041237799,20.,11.5647540978177));
#11030=CARTESIAN_POINT('Ctrl Pts',(3.46523470555786,20.,11.6482137561969));
#11031=CARTESIAN_POINT('Ctrl Pts',(3.36017632166553,20.,11.6874150779477));
#11032=CARTESIAN_POINT('Ctrl Pts',(3.25453010754725,20.,11.7251397777184));
#11033=CARTESIAN_POINT('Ctrl Pts',(3.14832787575819,20.,11.7613864006883));
#11034=CARTESIAN_POINT('Ctrl Pts',(-3.14809266229074,20.0004548598273,11.7612561652465));
#11035=CARTESIAN_POINT('Ctrl Pts',(-5.10435921967941,20.079872267689,11.2376294107338));
#11036=CARTESIAN_POINT('Ctrl Pts',(-8.74855648214142,20.2387070834124,9.19577637638592));
#11037=CARTESIAN_POINT('Ctrl Pts',(-12.0824131583271,20.4769593069975,3.88694525557923));
#11038=CARTESIAN_POINT('Ctrl Pts',(-12.4691756011198,20.7152115305826,-2.36849165908917));
#11039=CARTESIAN_POINT('Ctrl Pts',(-9.81532842158459,20.9534637541677,-8.04695416362741));
#11040=CARTESIAN_POINT('Ctrl Pts',(-4.76767052948596,21.1917159777528,-11.7626807483446));
#11041=CARTESIAN_POINT('Ctrl Pts',(1.44262007163241,21.4299682013379,-12.6099815538241));
#11042=CARTESIAN_POINT('Ctrl Pts',(7.30112969128478,21.668220424923,-10.3819902917566));
#11043=CARTESIAN_POINT('Ctrl Pts',(11.3790859526647,21.9064726485081,-5.62216684002108));
#11044=CARTESIAN_POINT('Ctrl Pts',(12.6820163068472,22.1447248720932,0.508761805007711));
#11045=CARTESIAN_POINT('Ctrl Pts',(10.8921610480429,22.3829770956783,6.51560837433268));
#11046=CARTESIAN_POINT('Ctrl Pts',(6.44602083161166,22.6212293192634,10.9334889418598));
#11047=CARTESIAN_POINT('Ctrl Pts',(0.427879238319787,22.8594815428485,12.6850014557692));
#11048=CARTESIAN_POINT('Ctrl Pts',(-5.69460937880687,23.0977337664336,11.343005608659));
#11049=CARTESIAN_POINT('Ctrl Pts',(-10.4283456669994,23.3359859900187,7.23477408056129));
#11050=CARTESIAN_POINT('Ctrl Pts',(-12.6189061760199,23.5742382136038,1.36218808736743));
#11051=CARTESIAN_POINT('Ctrl Pts',(-11.7320759505821,23.8124904371889,-4.8425968202088));
#11052=CARTESIAN_POINT('Ctrl Pts',(-7.9841274603316,24.050742660774,-9.86641060411259));
#11053=CARTESIAN_POINT('Ctrl Pts',(-2.28907833971999,24.2889948843591,-12.4840886814594));
#11054=CARTESIAN_POINT('Ctrl Pts',(3.96421161517394,24.5272471079442,-12.0572540805866));
#11055=CARTESIAN_POINT('Ctrl Pts',(9.25074357873224,24.7654993315293,-8.68999959656226));
#11056=CARTESIAN_POINT('Ctrl Pts',(12.2812834041494,25.0037515551144,-3.20350240934556));
#11057=CARTESIAN_POINT('Ctrl Pts',(12.3167689831387,25.2420037786995,3.06423751515814));
#11058=CARTESIAN_POINT('Ctrl Pts',(9.34854639793627,25.4802560022846,8.58469743127442));
#11059=CARTESIAN_POINT('Ctrl Pts',(4.10048035829082,25.7185082258697,12.0115948386183));
#11060=CARTESIAN_POINT('Ctrl Pts',(-2.14757572311472,25.9567604494548,12.5092073390711));
#11061=CARTESIAN_POINT('Ctrl Pts',(-7.87189942455396,26.1950126730399,9.95618145611697));
#11062=CARTESIAN_POINT('Ctrl Pts',(-11.6764916927204,26.433264896625,4.97512728354432));
#11063=CARTESIAN_POINT('Ctrl Pts',(-12.6335211398357,26.6715171202101,-1.21921833443057));
#11064=CARTESIAN_POINT('Ctrl Pts',(-10.5095956183063,26.9097693437952,-7.11623142381309));
#11065=CARTESIAN_POINT('Ctrl Pts',(-5.82267989949552,27.1480215673803,-11.2777989220269));
#11066=CARTESIAN_POINT('Ctrl Pts',(0.284221140002502,27.3862737909654,-12.6890333785201));
#11067=CARTESIAN_POINT('Ctrl Pts',(6.32180876134884,27.6245260145505,-11.0057750168977));
#11068=CARTESIAN_POINT('Ctrl Pts',(10.8176877886728,27.8627782381356,-6.63852247449934));
#11069=CARTESIAN_POINT('Ctrl Pts',(12.6754417380569,28.1010304617207,-0.652323909386644));
#11070=CARTESIAN_POINT('Ctrl Pts',(11.4420174822295,28.3392826853058,5.49295782561536));
#11071=CARTESIAN_POINT('Ctrl Pts',(7.41821196824626,28.5775349088909,10.2986640362622));
#11072=CARTESIAN_POINT('Ctrl Pts',(1.58531643343681,28.815787132476,12.592820237878));
#11073=CARTESIAN_POINT('Ctrl Pts',(-4.63419249983834,29.0540393560611,11.8159472583486));
#11074=CARTESIAN_POINT('Ctrl Pts',(-9.72355424374603,29.2922915796462,8.15750222841293));
#11075=CARTESIAN_POINT('Ctrl Pts',(-12.4416188307888,29.5305438032313,2.50967539873089));
#11076=CARTESIAN_POINT('Ctrl Pts',(-12.125527941276,29.7687960268164,-3.75018957960365));
#11077=CARTESIAN_POINT('Ctrl Pts',(-8.85236711500348,30.0070482504015,-9.0954904320129));
#11078=CARTESIAN_POINT('Ctrl Pts',(-3.42036678980662,30.2453004739866,-12.2226609525431));
#11079=CARTESIAN_POINT('Ctrl Pts',(2.8457633032496,30.4835526975717,-12.3690735691688));
#11080=CARTESIAN_POINT('Ctrl Pts',(8.41789300705035,30.7218049211568,-9.49902242651769));
#11081=CARTESIAN_POINT('Ctrl Pts',(11.9371390374505,30.9600571447419,-4.31243102416829));
#11082=CARTESIAN_POINT('Ctrl Pts',(12.5452578039889,31.198309368327,1.92583913375176));
#11083=CARTESIAN_POINT('Ctrl Pts',(10.0939465085343,31.4365615919121,7.69445213257467));
#11084=CARTESIAN_POINT('Ctrl Pts',(5.18100996193967,31.6748138154972,11.5866080244356));
#11085=CARTESIAN_POINT('Ctrl Pts',(-0.995426934883139,31.9130660390823,
12.6531211546773));
#11086=CARTESIAN_POINT('Ctrl Pts',(-6.92910763357261,32.1513182626674,10.6338994324754));
#11087=CARTESIAN_POINT('Ctrl Pts',(-11.1729768889136,32.3895704862526,6.02137336306566));
#11088=CARTESIAN_POINT('Ctrl Pts',(-12.692076202498,32.6278227098376,-0.0595936877313756));
#11089=CARTESIAN_POINT('Ctrl Pts',(-11.1159406401054,32.8660749334227,-6.12602754019977));
#11090=CARTESIAN_POINT('Ctrl Pts',(-6.82894464797713,33.1043271570078,-10.6984982465997));
#11091=CARTESIAN_POINT('Ctrl Pts',(-0.876564103841478,33.3425793805929,
-12.6619108000923));
#11092=CARTESIAN_POINT('Ctrl Pts',(5.28958538888388,33.580831604178,-11.5374449576727));
#11093=CARTESIAN_POINT('Ctrl Pts',(10.1657560858716,33.8190838277631,-7.5993258214283));
#11094=CARTESIAN_POINT('Ctrl Pts',(12.5627892268212,34.0573360513483,-1.80794816851931));
#11095=CARTESIAN_POINT('Ctrl Pts',(11.8961168924868,34.2955882749333,4.42433640425057));
#11096=CARTESIAN_POINT('Ctrl Pts',(8.32832142376291,34.5338404985185,9.57765169549019));
#11097=CARTESIAN_POINT('Ctrl Pts',(2.72948623249549,34.7720927221035,12.395251294106));
#11098=CARTESIAN_POINT('Ctrl Pts',(-3.53499269162053,35.0103449456886,12.1900031340674));
#11099=CARTESIAN_POINT('Ctrl Pts',(-8.9373878642459,35.2485971692737,9.01196137918274));
#11100=CARTESIAN_POINT('Ctrl Pts',(-12.1602094057867,35.4868493928589,3.63615964285339));
#11101=CARTESIAN_POINT('Ctrl Pts',(-12.4175031914886,35.7251016164439,-2.62639757513609));
#11102=CARTESIAN_POINT('Ctrl Pts',(-9.6465226171822,35.9633538400291,-8.24845143865874));
#11103=CARTESIAN_POINT('Ctrl Pts',(-4.52303069773245,36.2016060636141,-11.858943589337));
#11104=CARTESIAN_POINT('Ctrl Pts',(1.70349921887366,36.4398582871992,-12.5773781093279));
#11105=CARTESIAN_POINT('Ctrl Pts',(7.51459433853916,36.6781105107843,-10.2285493487157));
#11106=CARTESIAN_POINT('Ctrl Pts',(11.4930945153334,36.9163627343694,-5.38526953581525));
#11107=CARTESIAN_POINT('Ctrl Pts',(12.6687572341596,37.1546149579545,0.771323677356681));
#11108=CARTESIAN_POINT('Ctrl Pts',(10.7548718477098,37.3928671815396,6.73981312826219));
#11109=CARTESIAN_POINT('Ctrl Pts',(6.2181805169326,37.6311194051247,11.0646545543017));
#11110=CARTESIAN_POINT('Ctrl Pts',(0.165052320677689,37.8693716287098,12.6911429724317));
#11111=CARTESIAN_POINT('Ctrl Pts',(-5.92832693959693,38.107623852295,11.2226236804367));
#11112=CARTESIAN_POINT('Ctrl Pts',(-10.5759575529497,38.34587607588,7.01722786017004));
#11113=CARTESIAN_POINT('Ctrl Pts',(-12.644412242237,38.5841282994652,1.10052888764604));
#11114=CARTESIAN_POINT('Ctrl Pts',(-11.6292598420606,38.8223805230502,-5.08455422895767));
#11115=CARTESIAN_POINT('Ctrl Pts',(-7.77805527350331,39.0606327466353,-10.0296666573467));
#11116=CARTESIAN_POINT('Ctrl Pts',(-2.03002093474416,39.2988849702204,-12.528816073021));
#11117=CARTESIAN_POINT('Ctrl Pts',(4.21310916249937,39.5371371938055,-11.972572766274));
#11118=CARTESIAN_POINT('Ctrl Pts',(9.42871875276412,39.7753894173906,-8.49650536082229));
#11119=CARTESIAN_POINT('Ctrl Pts',(12.3450606821512,40.0136416409757,-2.94849454622041));
#11120=CARTESIAN_POINT('Ctrl Pts',(12.2505387102373,40.2518938645608,3.31879409118882));
#11121=CARTESIAN_POINT('Ctrl Pts',(9.16897630005181,40.4901460881459,8.77627054946899));
#11122=CARTESIAN_POINT('Ctrl Pts',(3.84984706557643,40.7284188590102,12.0946935166284));
#11123=CARTESIAN_POINT('Ctrl Pts',(-0.32088071557368,40.8872742220127,12.3384797159896));
#11124=CARTESIAN_POINT('Ctrl Pts',(-2.30975236282056,40.9667121771535,11.9541908119849));
#11125=CARTESIAN_POINT('Ctrl Pts',(-3.00369270810988,19.6780228441179,11.2217787630359));
#11126=CARTESIAN_POINT('Ctrl Pts',(-4.87022721769824,19.7574402519795,10.7221702594042));
#11127=CARTESIAN_POINT('Ctrl Pts',(-8.34726868959891,19.916275067703,8.77397504146546));
#11128=CARTESIAN_POINT('Ctrl Pts',(-11.5282045966303,20.154527291288,3.70865485023876));
#11129=CARTESIAN_POINT('Ctrl Pts',(-11.8972266216495,20.3927795148732,-2.25985124607116));
#11130=CARTESIAN_POINT('Ctrl Pts',(-9.36510883582578,20.6310317384582,-7.67784818830401));
#11131=CARTESIAN_POINT('Ctrl Pts',(-4.54898211085908,20.8692839620433,-11.2231380018903));
#11132=CARTESIAN_POINT('Ctrl Pts',(1.3764484894743,21.1075361856285,-12.031573942001));
#11133=CARTESIAN_POINT('Ctrl Pts',(6.96623396044474,21.3457884092135,-9.90577847614093));
#11134=CARTESIAN_POINT('Ctrl Pts',(10.8571383270859,21.5840406327987,-5.364283505194));
#11135=CARTESIAN_POINT('Ctrl Pts',(12.1003045308358,21.8222928563837,0.485425394929287));
#11136=CARTESIAN_POINT('Ctrl Pts',(10.3925481951215,22.0605450799689,6.21674374369965));
#11137=CARTESIAN_POINT('Ctrl Pts',(6.15034811400611,22.2987973035539,10.431980418571));
#11138=CARTESIAN_POINT('Ctrl Pts',(0.408252833052742,22.5370495271391,12.1031527538748));
#11139=CARTESIAN_POINT('Ctrl Pts',(-5.43340317505451,22.7753017507242,10.8227129534321));
#11140=CARTESIAN_POINT('Ctrl Pts',(-9.95000757532424,23.0135539743092,6.90292201716564));
#11141=CARTESIAN_POINT('Ctrl Pts',(-12.0400892004408,23.2518061978944,1.2997058422424));
#11142=CARTESIAN_POINT('Ctrl Pts',(-11.1939370164893,23.4900584214795,-4.62047160536659));
#11143=CARTESIAN_POINT('Ctrl Pts',(-7.61790328489481,23.7283106450646,-9.41384792823294));
#11144=CARTESIAN_POINT('Ctrl Pts',(-2.18408053856523,23.9665628686497,-11.911455653472));
#11145=CARTESIAN_POINT('Ctrl Pts',(3.78237707693078,24.2048150922347,-11.5041995413608));
#11146=CARTESIAN_POINT('Ctrl Pts',(8.82642095160353,24.4430673158199,-8.29139775151294));
#11147=CARTESIAN_POINT('Ctrl Pts',(11.7179528573444,24.6813195394049,-3.05656086386032));
#11148=CARTESIAN_POINT('Ctrl Pts',(11.7518107472756,24.9195717629901,2.92368391516781));
#11149=CARTESIAN_POINT('Ctrl Pts',(8.91973765043983,25.1578239865751,8.19092569431719));
#11150=CARTESIAN_POINT('Ctrl Pts',(3.9123953050936,25.3960762101603,11.4606346444945));
#11151=CARTESIAN_POINT('Ctrl Pts',(-2.04906850960975,25.6343284337454,11.9354221426448));
#11152=CARTESIAN_POINT('Ctrl Pts',(-7.51082304016482,25.8725806573305,9.49950107840742));
#11153=CARTESIAN_POINT('Ctrl Pts',(-11.1409023545732,26.1108328809156,4.74692302501242));
#11154=CARTESIAN_POINT('Ctrl Pts',(-12.0540337900549,26.3490851045007,-1.16329397307453));
#11155=CARTESIAN_POINT('Ctrl Pts',(-10.0275306702439,26.5873373280858,-6.78981679699862));
#11156=CARTESIAN_POINT('Ctrl Pts',(-5.55559922529289,26.8255895516709,-10.7604972342117));
#11157=CARTESIAN_POINT('Ctrl Pts',(0.271184192238789,27.063841775256,-12.1069997362434));
#11158=CARTESIAN_POINT('Ctrl Pts',(6.03183353081841,27.3020939988411,-10.500950801524));
#11159=CARTESIAN_POINT('Ctrl Pts',(10.3214909518584,27.5403462224262,-6.3340198934194));
#11160=CARTESIAN_POINT('Ctrl Pts',(12.0940315311332,27.7785984460113,-0.622402444953652));
#11161=CARTESIAN_POINT('Ctrl Pts',(10.9171832484849,28.0168506695964,5.24100118284009));
#11162=CARTESIAN_POINT('Ctrl Pts',(7.07794578702808,28.2551028931814,9.82627431509112));
#11163=CARTESIAN_POINT('Ctrl Pts',(1.51259950769554,28.4933551167666,12.0151997989567));
#11164=CARTESIAN_POINT('Ctrl Pts',(-4.42162658884796,28.7316073403516,11.2739612287927));
#11165=CARTESIAN_POINT('Ctrl Pts',(-9.27754425042827,28.9698595639368,7.78332552068034));
#11166=CARTESIAN_POINT('Ctrl Pts',(-11.870933853621,29.2081117875218,2.39455902463984));
#11167=CARTESIAN_POINT('Ctrl Pts',(-11.5693417463421,29.446364011107,-3.57817202435472));
#11168=CARTESIAN_POINT('Ctrl Pts',(-8.44631762951329,29.6846162346921,-8.678289116001));
#11169=CARTESIAN_POINT('Ctrl Pts',(-3.26347788572639,29.9228684582772,-11.6620193606813));
#11170=CARTESIAN_POINT('Ctrl Pts',(2.71523090325989,30.1611206818622,-11.801716172723));
#11171=CARTESIAN_POINT('Ctrl Pts',(8.03177242709483,30.3993729054474,-9.06331148967571));
#11172=CARTESIAN_POINT('Ctrl Pts',(11.3895940586429,30.6376251290325,-4.11462399969371));
#11173=CARTESIAN_POINT('Ctrl Pts',(11.9698190077354,30.8758773526176,1.83750276233406));
#11174=CARTESIAN_POINT('Ctrl Pts',(9.63094698161567,31.1141295762027,7.34151508319885));
#11175=CARTESIAN_POINT('Ctrl Pts',(4.94336206482527,31.3523817997878,11.0551415628917));
#11176=CARTESIAN_POINT('Ctrl Pts',(-0.949767667762671,31.5906340233729,
12.0727347712439));
#11177=CARTESIAN_POINT('Ctrl Pts',(-6.61127619335253,31.828886246958,10.1461327891339));
#11178=CARTESIAN_POINT('Ctrl Pts',(-10.6604832859937,32.0671384705431,5.7451788125851));
#11179=CARTESIAN_POINT('Ctrl Pts',(-12.1099029888395,32.3053906941281,-0.0568601831300151));
#11180=CARTESIAN_POINT('Ctrl Pts',(-10.6060632345463,32.5436429177133,-5.84503260421468));
#11181=CARTESIAN_POINT('Ctrl Pts',(-6.51570758666586,32.7818951412983,-10.2077685183684));
#11182=CARTESIAN_POINT('Ctrl Pts',(-0.836356959386205,33.0201473648835,
-12.0811212441569));
#11183=CARTESIAN_POINT('Ctrl Pts',(5.04695724234298,33.2583995884685,-11.0082335582726));
#11184=CARTESIAN_POINT('Ctrl Pts',(9.69946272335483,33.4966518120537,-7.25075212359403));
#11185=CARTESIAN_POINT('Ctrl Pts',(11.9865462812223,33.7349040356388,-1.72501934122564));
#11186=CARTESIAN_POINT('Ctrl Pts',(11.3504535596434,33.9731562592238,4.22139638863183));
#11187=CARTESIAN_POINT('Ctrl Pts',(7.94630940537469,34.211408482809,9.13833411041546));
#11188=CARTESIAN_POINT('Ctrl Pts',(2.6042873488569,34.4496607063941,11.8266931508312));
#11189=CARTESIAN_POINT('Ctrl Pts',(-3.37284600870548,34.6879129299792,11.630859524634));
#11190=CARTESIAN_POINT('Ctrl Pts',(-8.52743855952799,34.9261651535643,8.5985914597323));
#11191=CARTESIAN_POINT('Ctrl Pts',(-11.6024324057451,35.1644173771494,3.46937253010039));
#11192=CARTESIAN_POINT('Ctrl Pts',(-11.8479243752835,35.4026696007345,-2.5059272681298));
#11193=CARTESIAN_POINT('Ctrl Pts',(-9.20404598979087,35.6409218243196,-7.8701029789477));
#11194=CARTESIAN_POINT('Ctrl Pts',(-4.31556367068634,35.8791740479047,-11.3149853598205));
#11195=CARTESIAN_POINT('Ctrl Pts',(1.62536136349889,36.1174262714898,-12.0004659858516));
#11196=CARTESIAN_POINT('Ctrl Pts',(7.16990719156578,36.3556784950749,-9.75937572019344));
#11197=CARTESIAN_POINT('Ctrl Pts',(10.965917427667,36.59393071866,-5.1382524503469));
#11198=CARTESIAN_POINT('Ctrl Pts',(12.0876536389402,36.8321829422451,0.735943809094519));
#11199=CARTESIAN_POINT('Ctrl Pts',(10.2615563171244,37.0704351658302,6.43066444322939));
#11200=CARTESIAN_POINT('Ctrl Pts',(5.93295861336892,37.3086873894153,10.5571295917087));
#11201=CARTESIAN_POINT('Ctrl Pts',(0.157481530964674,37.5469396130003,12.1090125651303));
#11202=CARTESIAN_POINT('Ctrl Pts',(-5.65640033822935,37.7851918365855,10.7078528273879));
#11203=CARTESIAN_POINT('Ctrl Pts',(-10.0908486473709,38.0234440601705,6.69535443070501));
#11204=CARTESIAN_POINT('Ctrl Pts',(-12.0644253281625,38.2616962837557,1.05004869598765));
#11205=CARTESIAN_POINT('Ctrl Pts',(-11.0958369830495,38.4999485073408,-4.85133066267378));
#11206=CARTESIAN_POINT('Ctrl Pts',(-7.42128342921687,38.7382007309259,-9.56961558479783));
#11207=CARTESIAN_POINT('Ctrl Pts',(-1.93690584525694,38.976452954511,-11.954131443005));
#11208=CARTESIAN_POINT('Ctrl Pts',(4.01985793539565,39.2147051780961,-11.4234024767251));
#11209=CARTESIAN_POINT('Ctrl Pts',(8.99623257718483,39.4529574016812,-8.10677890851787));
#11210=CARTESIAN_POINT('Ctrl Pts',(11.7788047335206,39.6912096252663,-2.8132499638494));
#11211=CARTESIAN_POINT('Ctrl Pts',(11.6886183926944,39.9294618488514,3.16656422818516));
#11212=CARTESIAN_POINT('Ctrl Pts',(8.74840425861466,40.1677140724365,8.3737115395636));
#11213=CARTESIAN_POINT('Ctrl Pts',(3.67325831819566,40.4059868433008,11.5399216668183));
#11214=CARTESIAN_POINT('Ctrl Pts',(-0.306162228668456,40.5648422063033,
11.7725256298878));
#11215=CARTESIAN_POINT('Ctrl Pts',(-2.20380626429698,40.6442801614442,11.4058636848336));
#11216=CARTESIAN_POINT('Ctrl Pts',(-2.85929275392902,19.3555908284084,10.6823013608252));
#11217=CARTESIAN_POINT('Ctrl Pts',(-4.63609521571708,19.4350082362701,10.2067111080746));
#11218=CARTESIAN_POINT('Ctrl Pts',(-7.94598089705643,19.5938430519935,8.35217370654499));
#11219=CARTESIAN_POINT('Ctrl Pts',(-10.9739960349335,19.8320952755786,3.53036444489831));
#11220=CARTESIAN_POINT('Ctrl Pts',(-11.3252776421793,20.0703474991637,-2.15121083305315));
#11221=CARTESIAN_POINT('Ctrl Pts',(-8.91488925006696,20.3085997227488,-7.3087422129806));
#11222=CARTESIAN_POINT('Ctrl Pts',(-4.33029369223223,20.5468519463339,-10.683595255436));
#11223=CARTESIAN_POINT('Ctrl Pts',(1.31027690731619,20.785104169919,-11.4531663301778));
#11224=CARTESIAN_POINT('Ctrl Pts',(6.6313382296047,21.0233563935041,-9.42956666052528));
#11225=CARTESIAN_POINT('Ctrl Pts',(10.3351907015071,21.2616086170892,-5.10640017036693));
#11226=CARTESIAN_POINT('Ctrl Pts',(11.5185927548245,21.4998608406743,0.46208898485087));
#11227=CARTESIAN_POINT('Ctrl Pts',(9.89293534220016,21.7381130642594,5.91787911306662));
#11228=CARTESIAN_POINT('Ctrl Pts',(5.85467539640056,21.9763652878445,9.93047189528233));
#11229=CARTESIAN_POINT('Ctrl Pts',(0.388626427785698,22.2146175114296,11.5213040519803));
#11230=CARTESIAN_POINT('Ctrl Pts',(-5.17219697130216,22.4528697350147,10.3024202982052));
#11231=CARTESIAN_POINT('Ctrl Pts',(-9.47166948364905,22.6911219585998,6.57106995376998));
#11232=CARTESIAN_POINT('Ctrl Pts',(-11.4612722248617,22.9293741821849,1.23722359711736));
#11233=CARTESIAN_POINT('Ctrl Pts',(-10.6557980823965,23.16762640577,-4.39834639052438));
#11234=CARTESIAN_POINT('Ctrl Pts',(-7.25167910945802,23.4058786293551,-8.96128525235328));
#11235=CARTESIAN_POINT('Ctrl Pts',(-2.07908273741047,23.6441308529403,-11.3388226254846));
#11236=CARTESIAN_POINT('Ctrl Pts',(3.6005425386876,23.8823830765253,-10.9511450021349));
#11237=CARTESIAN_POINT('Ctrl Pts',(8.40209832447484,24.1206353001105,-7.89279590646365));
#11238=CARTESIAN_POINT('Ctrl Pts',(11.1546223105393,24.3588875236955,-2.90961931837506));
#11239=CARTESIAN_POINT('Ctrl Pts',(11.1868525114124,24.5971397472806,2.78313031517747));
#11240=CARTESIAN_POINT('Ctrl Pts',(8.49092890294339,24.8353919708657,7.79715395735995));
#11241=CARTESIAN_POINT('Ctrl Pts',(3.72431025189639,25.0736441944508,10.9096744503706));
#11242=CARTESIAN_POINT('Ctrl Pts',(-1.95056129610478,25.3118964180359,11.3616369462185));
#11243=CARTESIAN_POINT('Ctrl Pts',(-7.14974665577569,25.550148641621,9.04282070069786));
#11244=CARTESIAN_POINT('Ctrl Pts',(-10.6053130164261,25.7884008652061,4.51871876648054));
#11245=CARTESIAN_POINT('Ctrl Pts',(-11.4745464402741,26.0266530887912,-1.1073696117185));
#11246=CARTESIAN_POINT('Ctrl Pts',(-9.54546572218151,26.2649053123763,-6.46340217018414));
#11247=CARTESIAN_POINT('Ctrl Pts',(-5.28851855109027,26.5031575359614,-10.2431955463965));
#11248=CARTESIAN_POINT('Ctrl Pts',(0.258147244475094,26.7414097595465,-11.5249660939666));
#11249=CARTESIAN_POINT('Ctrl Pts',(5.74185830028796,26.9796619831316,-9.9961265861502));
#11250=CARTESIAN_POINT('Ctrl Pts',(9.82529411504405,27.2179142067167,-6.02951731233947));
#11251=CARTESIAN_POINT('Ctrl Pts',(11.5126213242094,27.4561664303018,-0.592480980520653));
#11252=CARTESIAN_POINT('Ctrl Pts',(10.3923490147401,27.6944186538869,4.98904454006481));
#11253=CARTESIAN_POINT('Ctrl Pts',(6.73767960580988,27.932670877472,9.35388459392002));
#11254=CARTESIAN_POINT('Ctrl Pts',(1.43988258195426,28.1709231010571,11.4375793600353));
#11255=CARTESIAN_POINT('Ctrl Pts',(-4.2090606778576,28.4091753246422,10.7319751992368));
#11256=CARTESIAN_POINT('Ctrl Pts',(-8.83153425711049,28.6474275482273,7.40914881294773));
#11257=CARTESIAN_POINT('Ctrl Pts',(-11.3002488764531,28.8856797718124,2.27944265054878));
#11258=CARTESIAN_POINT('Ctrl Pts',(-11.0131555514081,29.1239319953975,-3.40615446910582));
#11259=CARTESIAN_POINT('Ctrl Pts',(-8.04026814402308,29.3621842189826,-8.2610877999891));
#11260=CARTESIAN_POINT('Ctrl Pts',(-3.10658898164615,29.6004364425677,-11.1013777688193));
#11261=CARTESIAN_POINT('Ctrl Pts',(2.58469850327018,29.8386886661528,-11.2343587762771));
#11262=CARTESIAN_POINT('Ctrl Pts',(7.64565184713929,30.0769408897379,-8.62760055283371));
#11263=CARTESIAN_POINT('Ctrl Pts',(10.8420490798353,30.315193113323,-3.91681697521912));
#11264=CARTESIAN_POINT('Ctrl Pts',(11.3943802114819,30.5534453369081,1.74916639091636));
#11265=CARTESIAN_POINT('Ctrl Pts',(9.16794745469711,30.7916975604932,6.98857803382302));
#11266=CARTESIAN_POINT('Ctrl Pts',(4.70571416771088,31.0299497840783,10.5236751013477));
#11267=CARTESIAN_POINT('Ctrl Pts',(-0.904108400642208,31.2682020076634,
11.4923483878104));
#11268=CARTESIAN_POINT('Ctrl Pts',(-6.29344475313245,31.5064542312485,9.65836614579251));
#11269=CARTESIAN_POINT('Ctrl Pts',(-10.1479896830738,31.7447064548336,5.46898426210454));
#11270=CARTESIAN_POINT('Ctrl Pts',(-11.527729775181,31.9829586784187,-0.0541266785286571));
#11271=CARTESIAN_POINT('Ctrl Pts',(-10.0961858289872,32.2212109020038,-5.56403766822957));
#11272=CARTESIAN_POINT('Ctrl Pts',(-6.20247052535459,32.4594631255889,-9.71703879013706));
#11273=CARTESIAN_POINT('Ctrl Pts',(-0.79614981493094,32.6977153491741,-11.5003316882214));
#11274=CARTESIAN_POINT('Ctrl Pts',(4.80432909580209,32.9359675727591,-10.4790221588725));
#11275=CARTESIAN_POINT('Ctrl Pts',(9.23316936083815,33.1742197963443,-6.90217842575973));
#11276=CARTESIAN_POINT('Ctrl Pts',(11.4103033356234,33.4124720199293,-1.64209051393198));
#11277=CARTESIAN_POINT('Ctrl Pts',(10.8047902268001,33.6507242435144,4.01845637301311));
#11278=CARTESIAN_POINT('Ctrl Pts',(7.56429738698645,33.8889764670995,8.69901652534074));
#11279=CARTESIAN_POINT('Ctrl Pts',(2.47908846521831,34.1272286906846,11.2581350075564));
#11280=CARTESIAN_POINT('Ctrl Pts',(-3.21069932579042,34.3654809142697,11.0717159152007));
#11281=CARTESIAN_POINT('Ctrl Pts',(-8.11748925481006,34.6037331378548,8.18522154028186));
#11282=CARTESIAN_POINT('Ctrl Pts',(-11.0446554057036,34.8419853614399,3.30258541734742));
#11283=CARTESIAN_POINT('Ctrl Pts',(-11.2783455590783,35.080237585025,-2.38545696112353));
#11284=CARTESIAN_POINT('Ctrl Pts',(-8.76156936239957,35.3184898086102,-7.49175451923664));
#11285=CARTESIAN_POINT('Ctrl Pts',(-4.10809664364021,35.5567420321952,-10.771027130304));
#11286=CARTESIAN_POINT('Ctrl Pts',(1.5472235081241,35.7949942557803,-11.4235538623753));
#11287=CARTESIAN_POINT('Ctrl Pts',(6.82522004459241,36.0332464793655,-9.2902020916712));
#11288=CARTESIAN_POINT('Ctrl Pts',(10.4387403400005,36.2714987029505,-4.89123536487858));
#11289=CARTESIAN_POINT('Ctrl Pts',(11.5065500437207,36.5097509265356,0.70056394083236));
#11290=CARTESIAN_POINT('Ctrl Pts',(9.76824078653887,36.7480031501207,6.12151575819658));
#11291=CARTESIAN_POINT('Ctrl Pts',(5.64773670980524,36.9862553737058,10.0496046291158));
#11292=CARTESIAN_POINT('Ctrl Pts',(0.149910741251658,37.2245075972909,11.5268821578289));
#11293=CARTESIAN_POINT('Ctrl Pts',(-5.38447373686177,37.4627598208761,10.1930819743391));
#11294=CARTESIAN_POINT('Ctrl Pts',(-9.60573974179206,37.7010120444611,6.37348100123998));
#11295=CARTESIAN_POINT('Ctrl Pts',(-11.4844384140878,37.9392642680463,0.999568504329265));
#11296=CARTESIAN_POINT('Ctrl Pts',(-10.5624141240384,38.1775164916313,-4.61810709638991));
#11297=CARTESIAN_POINT('Ctrl Pts',(-7.06451158493042,38.4157687152165,-9.10956451224892));
#11298=CARTESIAN_POINT('Ctrl Pts',(-1.84379075576973,38.6540209388016,-11.379446812989));
#11299=CARTESIAN_POINT('Ctrl Pts',(3.82660670829195,38.8922731623866,-10.8742321871762));
#11300=CARTESIAN_POINT('Ctrl Pts',(8.56374640160554,39.1305253859717,-7.71705245621345));
#11301=CARTESIAN_POINT('Ctrl Pts',(11.2125487848899,39.3687776095568,-2.67800538147839));
#11302=CARTESIAN_POINT('Ctrl Pts',(11.1266980751514,39.607029833142,3.01433436518149));
#11303=CARTESIAN_POINT('Ctrl Pts',(8.32783221717754,39.845282056727,7.97115252965823));
#11304=CARTESIAN_POINT('Ctrl Pts',(3.49666957081488,40.0835548275914,10.9851498170082));
#11305=CARTESIAN_POINT('Ctrl Pts',(-0.291443741763231,40.2424101905938,
11.2065715437861));
#11306=CARTESIAN_POINT('Ctrl Pts',(-2.09786016577339,40.3218481457347,10.8575365576823));
#11307=CARTESIAN_POINT('Ctrl Pts',(-2.71489279974816,19.033158812699,10.1428239586147));
#11308=CARTESIAN_POINT('Ctrl Pts',(-4.40196321373591,19.1125762205607,9.69125195674494));
#11309=CARTESIAN_POINT('Ctrl Pts',(-7.54469310451393,19.2714110362841,7.93037237162453));
#11310=CARTESIAN_POINT('Ctrl Pts',(-10.4197874732365,19.5096632598692,3.35207403955784));
#11311=CARTESIAN_POINT('Ctrl Pts',(-10.7533286627092,19.7479154834543,-2.04257042003514));
#11312=CARTESIAN_POINT('Ctrl Pts',(-8.46466966430815,19.9861677070394,-6.9396362376572));
#11313=CARTESIAN_POINT('Ctrl Pts',(-4.11160527360535,20.2244199306245,-10.1440525089817));
#11314=CARTESIAN_POINT('Ctrl Pts',(1.24410532515808,20.4626721542096,-10.8747587183546));
#11315=CARTESIAN_POINT('Ctrl Pts',(6.29644249876465,20.7009243777947,-8.95335484490964));
#11316=CARTESIAN_POINT('Ctrl Pts',(9.81324307592822,20.9391766013798,-4.84851683553984));
#11317=CARTESIAN_POINT('Ctrl Pts',(10.936880978813,21.177428824965,0.438752574772446));
#11318=CARTESIAN_POINT('Ctrl Pts',(9.39332248927878,21.41568104855,5.6190144824336));
#11319=CARTESIAN_POINT('Ctrl Pts',(5.55900267879502,21.6539332721351,9.42896337199362));
#11320=CARTESIAN_POINT('Ctrl Pts',(0.369000022518657,21.8921854957201,10.9394553500859));
#11321=CARTESIAN_POINT('Ctrl Pts',(-4.9109907675498,22.1304377193053,9.78212764297827));
#11322=CARTESIAN_POINT('Ctrl Pts',(-8.99333139197382,22.3686899428904,6.23921789037432));
#11323=CARTESIAN_POINT('Ctrl Pts',(-10.8824552492826,22.6069421664755,1.17474135199233));
#11324=CARTESIAN_POINT('Ctrl Pts',(-10.1176591483038,22.8451943900607,-4.17622117568216));
#11325=CARTESIAN_POINT('Ctrl Pts',(-6.88545493402124,23.0834466136456,-8.50872257647364));
#11326=CARTESIAN_POINT('Ctrl Pts',(-1.9740849362557,23.3216988372308,-10.7661895974971));
#11327=CARTESIAN_POINT('Ctrl Pts',(3.41870800044444,23.5599510608158,-10.398090462909));
#11328=CARTESIAN_POINT('Ctrl Pts',(7.97777569734612,23.798203284401,-7.49419406141432));
#11329=CARTESIAN_POINT('Ctrl Pts',(10.5912917637341,24.0364555079861,-2.76267777288981));
#11330=CARTESIAN_POINT('Ctrl Pts',(10.6218942755493,24.2747077315713,2.64257671518715));
#11331=CARTESIAN_POINT('Ctrl Pts',(8.06212015544694,24.5129599551563,7.4033822204027));
#11332=CARTESIAN_POINT('Ctrl Pts',(3.53622519869919,24.7512121787414,10.3587142562468));
#11333=CARTESIAN_POINT('Ctrl Pts',(-1.85205408259982,24.9894644023265,10.7878517497922));
#11334=CARTESIAN_POINT('Ctrl Pts',(-6.78867027138654,25.2277166259116,8.5861403229883));
#11335=CARTESIAN_POINT('Ctrl Pts',(-10.0697236782791,25.4659688494967,4.29051450794865));
#11336=CARTESIAN_POINT('Ctrl Pts',(-10.8950590904933,25.7042210730819,-1.05144525036245));
#11337=CARTESIAN_POINT('Ctrl Pts',(-9.06340077411911,25.942473296667,-6.13698754336968));
#11338=CARTESIAN_POINT('Ctrl Pts',(-5.02143787688763,26.180725520252,-9.72589385858134));
#11339=CARTESIAN_POINT('Ctrl Pts',(0.245110296711381,26.4189777438371,-10.9429324516899));
#11340=CARTESIAN_POINT('Ctrl Pts',(5.45188306975753,26.6572299674222,-9.49130237077641));
#11341=CARTESIAN_POINT('Ctrl Pts',(9.32909727822967,26.8954821910073,-5.72501473125955));
#11342=CARTESIAN_POINT('Ctrl Pts',(10.9312111172857,27.1337344145924,-0.562559516087658));
#11343=CARTESIAN_POINT('Ctrl Pts',(9.86751478099552,27.3719866381776,4.73708789728954));
#11344=CARTESIAN_POINT('Ctrl Pts',(6.3974134245917,27.6102388617626,8.8814948727489));
#11345=CARTESIAN_POINT('Ctrl Pts',(1.367165656213,27.8484910853477,10.8599589211139));
#11346=CARTESIAN_POINT('Ctrl Pts',(-3.99649476686722,28.0867433089328,10.1899891696809));
#11347=CARTESIAN_POINT('Ctrl Pts',(-8.38552426379272,28.3249955325179,7.03497210521514));
#11348=CARTESIAN_POINT('Ctrl Pts',(-10.7295638992853,28.563247756103,2.16432627645773));
#11349=CARTESIAN_POINT('Ctrl Pts',(-10.4569693564742,28.8014999796882,-3.23413691385691));
#11350=CARTESIAN_POINT('Ctrl Pts',(-7.63421865853288,29.0397522032733,-7.84388648397718));
#11351=CARTESIAN_POINT('Ctrl Pts',(-2.94970007756592,29.2780044268583,-10.5407361769574));
#11352=CARTESIAN_POINT('Ctrl Pts',(2.45416610328047,29.5162566504434,-10.6670013798312));
#11353=CARTESIAN_POINT('Ctrl Pts',(7.25953126718375,29.7545088740285,-8.19188961599171));
#11354=CARTESIAN_POINT('Ctrl Pts',(10.2945041010277,29.9927610976136,-3.71900995074453));
#11355=CARTESIAN_POINT('Ctrl Pts',(10.8189414152284,30.2310133211988,1.66083001949865));
#11356=CARTESIAN_POINT('Ctrl Pts',(8.70494792777857,30.4692655447839,6.63564098444718));
#11357=CARTESIAN_POINT('Ctrl Pts',(4.46806627059647,30.7075177683689,9.9922086398038));
#11358=CARTESIAN_POINT('Ctrl Pts',(-0.858449133521731,30.945769991954,10.911962004377));
#11359=CARTESIAN_POINT('Ctrl Pts',(-5.97561331291237,31.1840222155391,9.17059950245109));
#11360=CARTESIAN_POINT('Ctrl Pts',(-9.63549608015401,31.4222744391242,5.19278971162398));
#11361=CARTESIAN_POINT('Ctrl Pts',(-10.9455565615224,31.6605266627094,-0.0513931739272948));
#11362=CARTESIAN_POINT('Ctrl Pts',(-9.58630842342816,31.8987788862945,-5.28304273224449));
#11363=CARTESIAN_POINT('Ctrl Pts',(-5.88923346404332,32.1370311098796,-9.2263090619057));
#11364=CARTESIAN_POINT('Ctrl Pts',(-0.755942670475671,32.3752833334646,
-10.919542132286));
#11365=CARTESIAN_POINT('Ctrl Pts',(4.56170094926121,32.6135355570497,-9.94981075947233));
#11366=CARTESIAN_POINT('Ctrl Pts',(8.76687599832148,32.8517877806348,-6.55360472792545));
#11367=CARTESIAN_POINT('Ctrl Pts',(10.8340603900244,33.0900400042199,-1.55916168663833));
#11368=CARTESIAN_POINT('Ctrl Pts',(10.2591268939567,33.3282922278051,3.81551635739438));
#11369=CARTESIAN_POINT('Ctrl Pts',(7.18228536859824,33.5665444513902,8.25969894026603));
#11370=CARTESIAN_POINT('Ctrl Pts',(2.35388958157973,33.8047966749752,10.6895768642816));
#11371=CARTESIAN_POINT('Ctrl Pts',(-3.04855264287536,34.0430488985603,10.5125723057673));
#11372=CARTESIAN_POINT('Ctrl Pts',(-7.70753995009214,34.2813011221453,7.77185162083141));
#11373=CARTESIAN_POINT('Ctrl Pts',(-10.4868784056621,34.5195533457305,3.13579830459444));
#11374=CARTESIAN_POINT('Ctrl Pts',(-10.7087667428733,34.7578055693157,-2.26498665411725));
#11375=CARTESIAN_POINT('Ctrl Pts',(-8.31909273500825,34.9960577929008,-7.11340605952559));
#11376=CARTESIAN_POINT('Ctrl Pts',(-3.90062961659408,35.2343100164858,-10.2270689007874));
#11377=CARTESIAN_POINT('Ctrl Pts',(1.46908565274932,35.4725622400709,-10.846641738899));
#11378=CARTESIAN_POINT('Ctrl Pts',(6.48053289761904,35.710814463656,-8.82102846314895));
#11379=CARTESIAN_POINT('Ctrl Pts',(9.91156325233417,35.9490666872411,-4.64421827941024));
#11380=CARTESIAN_POINT('Ctrl Pts',(10.9254464485013,36.1873189108261,0.665184072570199));
#11381=CARTESIAN_POINT('Ctrl Pts',(9.27492525595335,36.4255711344113,5.81236707316377));
#11382=CARTESIAN_POINT('Ctrl Pts',(5.36251480624159,36.6638233579963,9.54207966652283));
#11383=CARTESIAN_POINT('Ctrl Pts',(0.142339951538634,36.9020755815815,10.9447517505275));
#11384=CARTESIAN_POINT('Ctrl Pts',(-5.11254713549418,37.1403278051666,9.67831112129031));
#11385=CARTESIAN_POINT('Ctrl Pts',(-9.12063083621321,37.3785800287517,6.05160757177495));
#11386=CARTESIAN_POINT('Ctrl Pts',(-10.9044515000132,37.6168322523368,0.949088312670873));
#11387=CARTESIAN_POINT('Ctrl Pts',(-10.0289912650274,37.855084475922,-4.38488353010602));
#11388=CARTESIAN_POINT('Ctrl Pts',(-6.707739740644,38.093336699507,-8.64951343970004));
#11389=CARTESIAN_POINT('Ctrl Pts',(-1.75067566628252,38.3315889230921,-10.8047621829729));
#11390=CARTESIAN_POINT('Ctrl Pts',(3.63335548118823,38.5698411466772,-10.3250618976272));
#11391=CARTESIAN_POINT('Ctrl Pts',(8.13126022602624,38.8080933702623,-7.32732600390901));
#11392=CARTESIAN_POINT('Ctrl Pts',(10.6462928362593,39.0463455938474,-2.54276079910738));
#11393=CARTESIAN_POINT('Ctrl Pts',(10.5647777576085,39.2845978174326,2.86210450217782));
#11394=CARTESIAN_POINT('Ctrl Pts',(7.90726017574041,39.5228500410177,7.56859351975284));
#11395=CARTESIAN_POINT('Ctrl Pts',(3.32008082343409,39.7611228118819,10.430377967198));
#11396=CARTESIAN_POINT('Ctrl Pts',(-0.276725254858005,39.9199781748845,
10.6406174576843));
#11397=CARTESIAN_POINT('Ctrl Pts',(-1.99191406724981,39.9994161300253,10.309209430531));
#11398=CARTESIAN_POINT('Ctrl Pts',(-1.99079507083261,40.,10.3105642903746));
#11399=CARTESIAN_POINT('Ctrl Pts',(-1.74787308387841,40.,10.3776190639041));
#11400=CARTESIAN_POINT('Ctrl Pts',(-1.50291730396296,40.,10.4356201925428));
#11401=CARTESIAN_POINT('Ctrl Pts',(-1.25645144932171,40.,10.4847082098123));
#11402=CARTESIAN_POINT('Ctrl Pts',(-1.00610937738997,40.,10.5345682440478));
#11403=CARTESIAN_POINT('Ctrl Pts',(-0.754208867844965,40.,10.5752327777935));
#11404=CARTESIAN_POINT('Ctrl Pts',(-0.501269410076261,40.,10.6068040927733));
#11405=CARTESIAN_POINT('Ctrl Pts',(-0.244349094599502,40.,10.638872289156));
#11406=CARTESIAN_POINT('Ctrl Pts',(0.0136436862107205,40.,10.6615589815521));
#11407=CARTESIAN_POINT('Ctrl Pts',(0.272186552083508,40.,10.6749225223864));
#11408=CARTESIAN_POINT('Ctrl Pts',(0.531566233231362,40.,10.6883293164547));
#11409=CARTESIAN_POINT('Ctrl Pts',(0.79150020091699,40.,10.6923526126103));
#11410=CARTESIAN_POINT('Ctrl Pts',(1.05147389557568,40.,10.6870004795277));
#11411=CARTESIAN_POINT('Ctrl Pts',(1.31028375616657,40.,10.6816723065417));
#11412=CARTESIAN_POINT('Ctrl Pts',(1.56913363753882,40.,10.667052504031));
#11413=CARTESIAN_POINT('Ctrl Pts',(1.82751900740169,40.,10.6430977087009));
#11414=CARTESIAN_POINT('Ctrl Pts',(1.90159763837717,40.,10.6362299110222));
#11415=CARTESIAN_POINT('Ctrl Pts',(1.97563807441582,40.,10.62859448903));
#11416=CARTESIAN_POINT('Ctrl Pts',(2.04962835769163,40.,10.6201896290691));
#11417=CARTESIAN_POINT('Ctrl Pts',(2.08954125923063,40.,10.6156557587659));
#11418=CARTESIAN_POINT('Ctrl Pts',(2.12944528573599,40.,10.6108972103674));
#11419=CARTESIAN_POINT('Ctrl Pts',(2.1693057513364,40.,10.6059179310049));
#11420=CARTESIAN_POINT('Ctrl Pts',(2.43279869411477,40.,10.5730029875293));
#11421=CARTESIAN_POINT('Ctrl Pts',(2.69461388759011,40.,10.5304238386819));
#11422=CARTESIAN_POINT('Ctrl Pts',(2.95420990430317,40.,10.4782725649796));
#11423=CARTESIAN_POINT('Ctrl Pts',(3.07376860221186,40.,10.4542539438271));
#11424=CARTESIAN_POINT('Ctrl Pts',(3.19285681334819,40.,10.4282042572862));
#11425=CARTESIAN_POINT('Ctrl Pts',(3.31142253876288,40.,10.4001289044428));
#11426=CARTESIAN_POINT('Ctrl Pts',(3.56622266861186,40.,10.3397944062138));
#11427=CARTESIAN_POINT('Ctrl Pts',(3.81860986323782,40.,10.2701083948083));
#11428=CARTESIAN_POINT('Ctrl Pts',(4.06816673278697,40.,10.1914106777718));
#11429=CARTESIAN_POINT('Ctrl Pts',(4.32019405300233,40.,10.1119339045312));
#11430=CARTESIAN_POINT('Ctrl Pts',(4.56933530459187,40.,10.0232659756233));
#11431=CARTESIAN_POINT('Ctrl Pts',(4.81515658717821,40.,9.92570343342688));
#11432=CARTESIAN_POINT('Ctrl Pts',(5.0619503348636,40.,9.82775493535928));
#11433=CARTESIAN_POINT('Ctrl Pts',(5.30539839347577,40.,9.72084110650416));
#11434=CARTESIAN_POINT('Ctrl Pts',(5.54504886067588,40.,9.60521113795994));
#11435=CARTESIAN_POINT('Ctrl Pts',(5.66474353075312,40.,9.54745914983473));
#11436=CARTESIAN_POINT('Ctrl Pts',(5.7834906148258,40.,9.48753209970937));
#11437=CARTESIAN_POINT('Ctrl Pts',(5.90123189477887,40.,9.42545655578914));
#11438=CARTESIAN_POINT('Ctrl Pts',(5.95755288857904,40.,9.39576300798952));
#11439=CARTESIAN_POINT('Ctrl Pts',(6.0136437182583,40.,9.36557781144656));
#11440=CARTESIAN_POINT('Ctrl Pts',(6.06949788210085,40.,9.33490364295837));
#11441=CARTESIAN_POINT('Ctrl Pts',(6.11005050514561,40.,9.31263282362574));
#11442=CARTESIAN_POINT('Ctrl Pts',(6.15048573176791,40.,9.29010000366931));
#11443=CARTESIAN_POINT('Ctrl Pts',(6.19076456917044,40.,9.26732701566816));
#11444=CARTESIAN_POINT('Ctrl Pts',(6.42582634078894,40.,9.13442698056777));
#11445=CARTESIAN_POINT('Ctrl Pts',(6.65571575867433,40.,8.99327172535973));
#11446=CARTESIAN_POINT('Ctrl Pts',(6.8800037608189,40.,8.8442223141287));
#11447=CARTESIAN_POINT('Ctrl Pts',(7.10949099987972,40.,8.69171777737241));
#11448=CARTESIAN_POINT('Ctrl Pts',(7.33311477943246,40.,8.53094877669126));
#11449=CARTESIAN_POINT('Ctrl Pts',(7.55040528259981,40.,8.36224719022096));
#11450=CARTESIAN_POINT('Ctrl Pts',(7.76769578576717,40.,8.19354560375065));
#11451=CARTESIAN_POINT('Ctrl Pts',(7.97865366192367,40.,8.01691114350707));
#11452=CARTESIAN_POINT('Ctrl Pts',(8.18278913651048,40.,7.83262450231714));
#11453=CARTESIAN_POINT('Ctrl Pts',(8.3828805419461,40.,7.65198871075106));
#11454=CARTESIAN_POINT('Ctrl Pts',(8.57641773083029,40.,7.46400053667558));
#11455=CARTESIAN_POINT('Ctrl Pts',(8.76315973735538,40.,7.26911327772968));
#11456=CARTESIAN_POINT('Ctrl Pts',(8.95087399741526,40.,7.07321135780887));
#11457=CARTESIAN_POINT('Ctrl Pts',(9.13172256221306,40.,6.87033788468238));
#11458=CARTESIAN_POINT('Ctrl Pts',(9.305425145709,40.,6.66091475544659));
#11459=CARTESIAN_POINT('Ctrl Pts',(9.35096602906598,40.,6.60600875399955));
#11460=CARTESIAN_POINT('Ctrl Pts',(9.39601551120144,40.,6.5506523646528));
#11461=CARTESIAN_POINT('Ctrl Pts',(9.44056808201162,40.,6.49485281517297));
#11462=CARTESIAN_POINT('Ctrl Pts',(9.45871046836229,40.,6.47213051281313));
#11463=CARTESIAN_POINT('Ctrl Pts',(9.4767704796353,40.,6.44933463079931));
#11464=CARTESIAN_POINT('Ctrl Pts',(9.49473878095482,40.,6.42647721576431));
#11465=CARTESIAN_POINT('Ctrl Pts',(9.66342503031443,40.,6.21189201131206));
#11466=CARTESIAN_POINT('Ctrl Pts',(9.82423055529979,40.,5.99163828046606));
#11467=CARTESIAN_POINT('Ctrl Pts',(9.97696748002078,40.,5.76623949569044));
#11468=CARTESIAN_POINT('Ctrl Pts',(10.132296481448,40.,5.53701550007802));
#11469=CARTESIAN_POINT('Ctrl Pts',(10.2792811505019,40.,5.30246996680171));
#11470=CARTESIAN_POINT('Ctrl Pts',(10.417694044559,40.,5.06310861315508));
#11471=CARTESIAN_POINT('Ctrl Pts',(10.5565955437288,40.,4.82290230079295));
#11472=CARTESIAN_POINT('Ctrl Pts',(10.6868650563927,40.,4.57784561876773));
#11473=CARTESIAN_POINT('Ctrl Pts',(10.8082364605648,40.,4.32841151267132));
#11474=CARTESIAN_POINT('Ctrl Pts',(10.9290278820725,40.,4.08016934678893));
#11475=CARTESIAN_POINT('Ctrl Pts',(11.0410063966906,40.,3.82759096156524));
#11476=CARTESIAN_POINT('Ctrl Pts',(11.1438680898851,40.,3.5711125486244));
#11477=CARTESIAN_POINT('Ctrl Pts',(11.210257734195,40.,3.40557462989577));
#11478=CARTESIAN_POINT('Ctrl Pts',(11.2728486825664,40.,3.23841146991623));
#11479=CARTESIAN_POINT('Ctrl Pts',(11.3315488558307,40.,3.06973522608137));
#11480=CARTESIAN_POINT('Ctrl Pts',(11.3969138737467,40.,2.88190740399589));
#11481=CARTESIAN_POINT('Ctrl Pts',(11.4574546537082,40.,2.69220336876743));
#11482=CARTESIAN_POINT('Ctrl Pts',(11.5131538719282,40.,2.50080739873));
#11483=CARTESIAN_POINT('Ctrl Pts',(11.5219564527078,40.,2.47055960457811));
#11484=CARTESIAN_POINT('Ctrl Pts',(11.5306367798565,40.,2.44027394775997));
#11485=CARTESIAN_POINT('Ctrl Pts',(11.5391927173603,40.,2.40995901899243));
#11486=CARTESIAN_POINT('Ctrl Pts',(11.6149930718682,40.,2.14138735791638));
#11487=CARTESIAN_POINT('Ctrl Pts',(11.6810877877354,40.,1.87033611873908));
#11488=CARTESIAN_POINT('Ctrl Pts',(11.7375427831218,40.,1.59736118879834));
#11489=CARTESIAN_POINT('Ctrl Pts',(11.7945063360496,40.,1.32192724777677));
#11490=CARTESIAN_POINT('Ctrl Pts',(11.84165587897,40.,1.04453424120747));
#11491=CARTESIAN_POINT('Ctrl Pts',(11.8790117311798,40.,0.765728997851488));
#11492=CARTESIAN_POINT('Ctrl Pts',(11.9165716381981,40.,0.485400792305021));
#11493=CARTESIAN_POINT('Ctrl Pts',(11.9442307186072,40.,0.203644272153142));
#11494=CARTESIAN_POINT('Ctrl Pts',(11.9619595697314,40.,-0.079000249593141));
#11495=CARTESIAN_POINT('Ctrl Pts',(11.9657577577725,40.,-0.139553357906196));
#11496=CARTESIAN_POINT('Ctrl Pts',(11.9690999836776,40.,-0.200147260578903));
#11497=CARTESIAN_POINT('Ctrl Pts',(11.9719856511623,40.,-0.260776694674976));
#11498=CARTESIAN_POINT('Ctrl Pts',(11.9737712450156,40.,-0.298292986980646));
#11499=CARTESIAN_POINT('Ctrl Pts',(11.9753819638708,40.,-0.335822485014976));
#11500=CARTESIAN_POINT('Ctrl Pts',(11.9768172604587,40.,-0.37335023804946));
#11501=CARTESIAN_POINT('Ctrl Pts',(11.9877545329118,40.,-0.659319885686097));
#11502=CARTESIAN_POINT('Ctrl Pts',(11.9885197420998,40.,-0.945390292321608));
#11503=CARTESIAN_POINT('Ctrl Pts',(11.9791433269757,40.,-1.23099730766982));
#11504=CARTESIAN_POINT('Ctrl Pts',(11.9697517430833,40.,-1.51706636598248));
#11505=CARTESIAN_POINT('Ctrl Pts',(11.9501858036841,40.,-1.80267116625394));
#11506=CARTESIAN_POINT('Ctrl Pts',(11.920425517138,40.,-2.08725729224288));
#11507=CARTESIAN_POINT('Ctrl Pts',(11.894682539692,40.,-2.33342744290519));
#11508=CARTESIAN_POINT('Ctrl Pts',(11.8613109472795,40.,-2.57883581888343));
#11509=CARTESIAN_POINT('Ctrl Pts',(11.8202663870092,40.,-2.82312554759088));
#11510=CARTESIAN_POINT('Ctrl Pts',(11.8016841988292,40.,-2.93372333885433));
#11511=CARTESIAN_POINT('Ctrl Pts',(11.7815289081037,40.,-3.04409183784577));
#11512=CARTESIAN_POINT('Ctrl Pts',(11.7598151666302,40.,-3.1542027559576));
#11513=CARTESIAN_POINT('Ctrl Pts',(-3.14788895504392,20.,11.7604951161383));
#11514=CARTESIAN_POINT('Ctrl Pts',(-3.41583726409301,20.,11.6689078365353));
#11515=CARTESIAN_POINT('Ctrl Pts',(-3.6800281171579,20.,11.5679423474188));
#11516=CARTESIAN_POINT('Ctrl Pts',(-3.9400576560663,20.,11.4579525320777));
#11517=CARTESIAN_POINT('Ctrl Pts',(-4.20217416504438,20.,11.3470799499035));
#11518=CARTESIAN_POINT('Ctrl Pts',(-4.46006282882018,20.,11.2270372658007));
#11519=CARTESIAN_POINT('Ctrl Pts',(-4.71328870839101,20.,11.0981380892181));
#11520=CARTESIAN_POINT('Ctrl Pts',(-4.96683786887351,20.,10.9690743534546));
#11521=CARTESIAN_POINT('Ctrl Pts',(-5.21571284554744,20.,10.83113111242));
#11522=CARTESIAN_POINT('Ctrl Pts',(-5.45944793424098,20.,10.6845799111558));
#11523=CARTESIAN_POINT('Ctrl Pts',(-5.70414316212735,20.,10.5374514046179));
#11524=CARTESIAN_POINT('Ctrl Pts',(-5.94365846472394,20.,10.3816466219635));
#11525=CARTESIAN_POINT('Ctrl Pts',(-6.17748537895062,20.,10.217402357069));
#11526=CARTESIAN_POINT('Ctrl Pts',(-6.35285556462064,20.,10.0942191583982));
#11527=CARTESIAN_POINT('Ctrl Pts',(-6.52502531488677,20.,9.96628793618934));
#11528=CARTESIAN_POINT('Ctrl Pts',(-6.69376370917604,20.,9.83369652447978));
#11529=CARTESIAN_POINT('Ctrl Pts',(-6.820317504893,20.,9.73425296569761));
#11530=CARTESIAN_POINT('Ctrl Pts',(-6.94494088210404,20.,9.63218783287827));
#11531=CARTESIAN_POINT('Ctrl Pts',(-7.06753052972854,20.,9.52753487809413));
#11532=CARTESIAN_POINT('Ctrl Pts',(-7.10083026097056,20.,9.49910739391806));
#11533=CARTESIAN_POINT('Ctrl Pts',(-7.13398139822032,20.,9.47048763974647));
#11534=CARTESIAN_POINT('Ctrl Pts',(-7.16697685356759,20.,9.44168058839424));
#11535=CARTESIAN_POINT('Ctrl Pts',(-7.19428556748663,20.,9.41783841025336));
#11536=CARTESIAN_POINT('Ctrl Pts',(-7.22148095759086,20.,9.39387375887951));
#11537=CARTESIAN_POINT('Ctrl Pts',(-7.24855699528293,20.,9.36979178935576));
#11538=CARTESIAN_POINT('Ctrl Pts',(-7.45693217325836,20.,9.18445873794766));
#11539=CARTESIAN_POINT('Ctrl Pts',(-7.65835188432274,20.,8.99208370611105));
#11540=CARTESIAN_POINT('Ctrl Pts',(-7.85239628045986,20.,8.79294161458531));
#11541=CARTESIAN_POINT('Ctrl Pts',(-7.93912888420864,20.,8.70393047869144));
#11542=CARTESIAN_POINT('Ctrl Pts',(-8.02438754640145,20.,8.61356687435558));
#11543=CARTESIAN_POINT('Ctrl Pts',(-8.1081323460688,20.,8.52187300942612));
#11544=CARTESIAN_POINT('Ctrl Pts',(-8.29599191369493,20.,8.31618179172615));
#11545=CARTESIAN_POINT('Ctrl Pts',(-8.47623651864031,20.,8.10379842051365));
#11546=CARTESIAN_POINT('Ctrl Pts',(-8.64862143631702,20.,7.88521040928684));
#11547=CARTESIAN_POINT('Ctrl Pts',(-8.82101815485311,20.,7.66660743430092));
#11548=CARTESIAN_POINT('Ctrl Pts',(-8.98555437557762,20.,7.44179836758922));
#11549=CARTESIAN_POINT('Ctrl Pts',(-9.14193907463545,20.,7.21124696764572));
#11550=CARTESIAN_POINT('Ctrl Pts',(-9.29725248533917,20.,6.9822749231716));
#11551=CARTESIAN_POINT('Ctrl Pts',(-9.44452587936642,20.,6.74763835396367));
#11552=CARTESIAN_POINT('Ctrl Pts',(-9.58342512130665,20.,6.50777699622786));
#11553=CARTESIAN_POINT('Ctrl Pts',(-9.65196330298591,20.,6.38942025730912));
#11554=CARTESIAN_POINT('Ctrl Pts',(-9.71846176138575,20.,6.26979121209968));
#11555=CARTESIAN_POINT('Ctrl Pts',(-9.7828756676878,20.,6.14894204377767));
#11556=CARTESIAN_POINT('Ctrl Pts',(-9.8132088705112,20.,6.0920328677286));
#11557=CARTESIAN_POINT('Ctrl Pts',(-9.84307976363647,20.,6.03485311738496));
#11558=CARTESIAN_POINT('Ctrl Pts',(-9.87248341765159,20.,5.97740823126373));
#11559=CARTESIAN_POINT('Ctrl Pts',(-9.88901621089197,20.,5.94510869378205));
#11560=CARTESIAN_POINT('Ctrl Pts',(-9.90540128472552,20.,5.91272533420826));
#11561=CARTESIAN_POINT('Ctrl Pts',(-9.92163774038952,20.,5.88025911929686));
#11562=CARTESIAN_POINT('Ctrl Pts',(-9.93566445772471,20.,5.85221146967865));
#11563=CARTESIAN_POINT('Ctrl Pts',(-9.94957694938171,20.,5.82410855112396));
#11564=CARTESIAN_POINT('Ctrl Pts',(-9.96337153280697,20.,5.79595784393599));
#11565=CARTESIAN_POINT('Ctrl Pts',(-10.0085819479117,20.,5.70369661949572));
#11566=CARTESIAN_POINT('Ctrl Pts',(-10.0525370783396,20.,5.61089988168351));
#11567=CARTESIAN_POINT('Ctrl Pts',(-10.0952260574459,20.,5.51759230643859));
#11568=CARTESIAN_POINT('Ctrl Pts',(-10.2089718891463,20.,5.26897198399479));
#11569=CARTESIAN_POINT('Ctrl Pts',(-10.3137316524454,20.,5.01672675586682));
#11570=CARTESIAN_POINT('Ctrl Pts',(-10.409265014146,20.,4.76131291339675));
#11571=CARTESIAN_POINT('Ctrl Pts',(-10.5040506875237,20.,4.50789805792076));
#11572=CARTESIAN_POINT('Ctrl Pts',(-10.5897539804176,20.,4.25136340325132));
#11573=CARTESIAN_POINT('Ctrl Pts',(-10.6660911547673,20.,3.99214066991294));
#11574=CARTESIAN_POINT('Ctrl Pts',(-10.7164100476478,20.,3.82126977952232));
#11575=CARTESIAN_POINT('Ctrl Pts',(-10.7626583544202,20.,3.64923065117632));
#11576=CARTESIAN_POINT('Ctrl Pts',(-10.8047424783443,20.,3.47614542570932));
#11577=CARTESIAN_POINT('Ctrl Pts',(-10.8705314538897,20.,3.20556596239269));
#11578=CARTESIAN_POINT('Ctrl Pts',(-10.9261465394823,20.,2.93242944986049));
#11579=CARTESIAN_POINT('Ctrl Pts',(-10.971539533839,20.,2.65731524077356));
#11580=CARTESIAN_POINT('Ctrl Pts',(-11.0169325281957,20.,2.38220103168662));
#11581=CARTESIAN_POINT('Ctrl Pts',(-11.0521033806315,20.,2.10510839212968));
#11582=CARTESIAN_POINT('Ctrl Pts',(-11.0769480123086,20.,1.82662914162098));
#11583=CARTESIAN_POINT('Ctrl Pts',(-11.0805510773543,20.,1.78624299838922));
#11584=CARTESIAN_POINT('Ctrl Pts',(-11.0839368669433,20.,1.74582772459025));
#11585=CARTESIAN_POINT('Ctrl Pts',(-11.0871049669885,20.,1.70538516141017));
#11586=CARTESIAN_POINT('Ctrl Pts',(-11.0904162776532,20.,1.6631144348383));
#11587=CARTESIAN_POINT('Ctrl Pts',(-11.093490147485,20.,1.62080741465348));
#11588=CARTESIAN_POINT('Ctrl Pts',(-11.0963238911948,20.,1.57850150671815));
#11589=CARTESIAN_POINT('Ctrl Pts',(-11.1141911417013,20.,1.31175534601927));
#11590=CARTESIAN_POINT('Ctrl Pts',(-11.1225356031101,20.,1.04484600136694));
#11591=CARTESIAN_POINT('Ctrl Pts',(-11.1214040387022,20.,0.778285111146802));
#11592=CARTESIAN_POINT('Ctrl Pts',(-11.1202704089922,20.,0.511237700885669));
#11593=CARTESIAN_POINT('Ctrl Pts',(-11.1096260686206,20.,0.244539372120431));
#11594=CARTESIAN_POINT('Ctrl Pts',(-11.0894661186789,20.,-0.0212930842774587));
#11595=CARTESIAN_POINT('Ctrl Pts',(-11.0694226014249,20.,-0.285590239869608));
#11596=CARTESIAN_POINT('Ctrl Pts',(-11.0399729544881,20.,-0.549032106527681));
#11597=CARTESIAN_POINT('Ctrl Pts',(-11.0010625248055,20.,-0.811099100292543));
#11598=CARTESIAN_POINT('Ctrl Pts',(-10.9627843225331,20.,-1.06890795714815));
#11599=CARTESIAN_POINT('Ctrl Pts',(-10.9153500990796,20.,-1.32538677858601));
#11600=CARTESIAN_POINT('Ctrl Pts',(-10.8586617973662,20.,-1.58002123097109));
#11601=CARTESIAN_POINT('Ctrl Pts',(-10.824283554091,20.,-1.73444259985593));
#11602=CARTESIAN_POINT('Ctrl Pts',(-10.786501025353,20.,-1.88818524282884));
#11603=CARTESIAN_POINT('Ctrl Pts',(-10.7452842897659,20.,-2.04112961510651));
#11604=CARTESIAN_POINT('Ctrl Pts',(-10.6983394263361,20.,-2.21532955031828));
#11605=CARTESIAN_POINT('Ctrl Pts',(-10.6469394936606,20.,-2.38849410088829));
#11606=CARTESIAN_POINT('Ctrl Pts',(-10.5911391151801,20.,-2.5604596881072));
#11607=CARTESIAN_POINT('Ctrl Pts',(-10.5808112700642,20.,-2.59228803763508));
#11608=CARTESIAN_POINT('Ctrl Pts',(-10.5703323195386,20.,-2.6240761705273));
#11609=CARTESIAN_POINT('Ctrl Pts',(-10.5597080024052,20.,-2.65580723494851));
#11610=CARTESIAN_POINT('Ctrl Pts',(-10.4761217376019,20.,-2.90544974089902));
#11611=CARTESIAN_POINT('Ctrl Pts',(-10.3834680471007,20.,-3.15179168198811));
#11612=CARTESIAN_POINT('Ctrl Pts',(-10.282020382983,20.,-3.39437485165473));
#11613=CARTESIAN_POINT('Ctrl Pts',(-10.1805768302556,20.,-3.63694819010331));
#11614=CARTESIAN_POINT('Ctrl Pts',(-10.0703396373221,20.,-3.87576361222901));
#11615=CARTESIAN_POINT('Ctrl Pts',(-9.95153837324811,20.,-4.1103350806491));
#11616=CARTESIAN_POINT('Ctrl Pts',(-9.83294619673873,20.,-4.34449370853715));
#11617=CARTESIAN_POINT('Ctrl Pts',(-9.70581969057772,20.,-4.5744238410096));
#11618=CARTESIAN_POINT('Ctrl Pts',(-9.57034919813197,20.,-4.79960611610117));
#11619=CARTESIAN_POINT('Ctrl Pts',(-9.54674783630744,20.,-4.83883686115094));
#11620=CARTESIAN_POINT('Ctrl Pts',(-9.52289211440892,20.,-4.8779250440819));
#11621=CARTESIAN_POINT('Ctrl Pts',(-9.49878620932176,20.,-4.91686250731363));
#11622=CARTESIAN_POINT('Ctrl Pts',(-9.4714725605423,20.,-4.96098133177716));
#11623=CARTESIAN_POINT('Ctrl Pts',(-9.44384412923328,20.,-5.00489629459305));
#11624=CARTESIAN_POINT('Ctrl Pts',(-9.41590688328757,20.,-5.0485974151017));
#11625=CARTESIAN_POINT('Ctrl Pts',(-9.27645734340157,20.,-5.26673277315658));
#11626=CARTESIAN_POINT('Ctrl Pts',(-9.12928197466736,20.,-5.47959889217826));
#11627=CARTESIAN_POINT('Ctrl Pts',(-8.97460595807497,20.,-5.68672989826698));
#11628=CARTESIAN_POINT('Ctrl Pts',(-8.82197249701016,20.,-5.89112566077535));
#11629=CARTESIAN_POINT('Ctrl Pts',(-8.66203475265525,20.,-6.08993719137158));
#11630=CARTESIAN_POINT('Ctrl Pts',(-8.49497511955485,20.,-6.28267973360122));
#11631=CARTESIAN_POINT('Ctrl Pts',(-8.37973300106364,20.,-6.41563859671912));
#11632=CARTESIAN_POINT('Ctrl Pts',(-8.2611011573261,20.,-6.54570870489164));
#11633=CARTESIAN_POINT('Ctrl Pts',(-8.13913138220323,20.,-6.6727188759329));
#11634=CARTESIAN_POINT('Ctrl Pts',(-8.07193084909504,20.,-6.74269646829574));
#11635=CARTESIAN_POINT('Ctrl Pts',(-8.0037169417772,20.,-6.81174500263592));
#11636=CARTESIAN_POINT('Ctrl Pts',(-7.93451184210526,20.,-6.87984615149801));
#11637=CARTESIAN_POINT('Origin',(0.,40.,-2.22044604925031E-15));
#11638=CARTESIAN_POINT('',(9.46171656752341,40.,16.3881738217667));
#11639=CARTESIAN_POINT('',(-9.46171656752339,40.,16.3881738217667));
#11640=CARTESIAN_POINT('',(9.46171656752341,40.,16.3881738217667));
#11641=CARTESIAN_POINT('',(18.9234331350468,40.,-1.22124532708767E-14));
#11642=CARTESIAN_POINT('',(18.9234331350468,40.,-1.22124532708767E-14));
#11643=CARTESIAN_POINT('',(9.46171656752339,40.,-16.3881738217667));
#11644=CARTESIAN_POINT('',(9.46171656752339,40.,-16.3881738217667));
#11645=CARTESIAN_POINT('',(-9.4617165675234,40.,-16.3881738217667));
#11646=CARTESIAN_POINT('',(-9.4617165675234,40.,-16.3881738217667));
#11647=CARTESIAN_POINT('',(-18.9234331350468,40.,4.44089209850063E-15));
#11648=CARTESIAN_POINT('',(-18.9234331350468,40.,4.44089209850063E-15));
#11649=CARTESIAN_POINT('',(-9.46171656752339,40.,16.3881738217667));
#11650=CARTESIAN_POINT('Origin',(18.9234331350468,20.,-1.22124532708767E-14));
#11651=CARTESIAN_POINT('',(18.9234331350468,20.,-1.22124532708767E-14));
#11652=CARTESIAN_POINT('',(9.46171656752341,20.,16.3881738217667));
#11653=CARTESIAN_POINT('',(18.9234331350468,20.,-1.22124532708767E-14));
#11654=CARTESIAN_POINT('',(18.9234331350468,20.,-1.22124532708767E-14));
#11655=CARTESIAN_POINT('',(9.46171656752341,20.,16.3881738217667));
#11656=CARTESIAN_POINT('Origin',(9.46171656752339,20.,-16.3881738217667));
#11657=CARTESIAN_POINT('',(9.46171656752339,20.,-16.3881738217667));
#11658=CARTESIAN_POINT('',(9.46171656752339,20.,-16.3881738217667));
#11659=CARTESIAN_POINT('',(9.46171656752339,20.,-16.3881738217667));
#11660=CARTESIAN_POINT('Origin',(-9.4617165675234,20.,-16.3881738217667));
#11661=CARTESIAN_POINT('',(-9.4617165675234,20.,-16.3881738217667));
#11662=CARTESIAN_POINT('',(-9.4617165675234,20.,-16.3881738217667));
#11663=CARTESIAN_POINT('',(-9.4617165675234,20.,-16.3881738217667));
#11664=CARTESIAN_POINT('Origin',(-18.9234331350468,20.,4.44089209850063E-15));
#11665=CARTESIAN_POINT('',(-18.9234331350468,20.,4.44089209850063E-15));
#11666=CARTESIAN_POINT('',(-18.9234331350468,20.,4.44089209850063E-15));
#11667=CARTESIAN_POINT('',(-18.9234331350468,20.,4.44089209850063E-15));
#11668=CARTESIAN_POINT('Origin',(-9.46171656752339,20.,16.3881738217667));
#11669=CARTESIAN_POINT('',(-9.46171656752339,20.,16.3881738217667));
#11670=CARTESIAN_POINT('',(-9.46171656752339,20.,16.3881738217667));
#11671=CARTESIAN_POINT('',(-9.46171656752339,20.,16.3881738217667));
#11672=CARTESIAN_POINT('Origin',(9.46171656752341,20.,16.3881738217667));
#11673=CARTESIAN_POINT('',(9.46171656752341,20.,16.3881738217667));
#11674=CARTESIAN_POINT('Origin',(0.,20.,-2.22044604925031E-15));
#11675=CARTESIAN_POINT('',(0.,0.,0.));
#11676=CARTESIAN_POINT('Origin',(0.,0.,4.68922655072688));
#11677=CARTESIAN_POINT('',(-1.47525540501185,-2.86526422036142,7.65376407014636));
#11678=CARTESIAN_POINT('',(-1.47525540501185,-2.86526422036142,7.40717138384282));
#11679=CARTESIAN_POINT('',(-1.47525540501186,-2.86526422036142,4.68922655072688));
#11680=CARTESIAN_POINT('',(1.87152456426716,2.62364505370765,7.00006724526264));
#11681=CARTESIAN_POINT('Ctrl Pts',(1.87152456426716,2.62364505370765,7.00006724526264));
#11682=CARTESIAN_POINT('Ctrl Pts',(1.79127682369291,2.68088816953973,7.00618730725958));
#11683=CARTESIAN_POINT('Ctrl Pts',(1.70825160021717,2.73455212168423,7.01230736925651));
#11684=CARTESIAN_POINT('Ctrl Pts',(1.62280488302109,2.78435304409174,7.01842743125345));
#11685=CARTESIAN_POINT('Ctrl Pts',(1.53747062668585,2.83408842091963,7.02453943831904));
#11686=CARTESIAN_POINT('Ctrl Pts',(1.44972158771444,2.87997064926674,7.03065144538463));
#11687=CARTESIAN_POINT('Ctrl Pts',(1.35994463582073,2.92175771582834,7.03676345245022));
#11688=CARTESIAN_POINT('Ctrl Pts',(1.26815769042948,2.96448034246742,7.04301229969806));
#11689=CARTESIAN_POINT('Ctrl Pts',(1.17425130695441,3.00292194634153,7.0492611469459));
#11690=CARTESIAN_POINT('Ctrl Pts',(1.07866802208888,3.03687221670963,7.05550999419374));
#11691=CARTESIAN_POINT('Ctrl Pts',(0.98533379127609,3.07002364454715,7.06161180741521));
#11692=CARTESIAN_POINT('Ctrl Pts',(0.890401144946329,3.09889261286461,7.06771362063667));
#11693=CARTESIAN_POINT('Ctrl Pts',(0.794303269988383,3.12333153504167,7.07381543385814));
#11694=CARTESIAN_POINT('Ctrl Pts',(0.698234643998841,3.14776301883091,7.07991538989242));
#11695=CARTESIAN_POINT('Ctrl Pts',(0.601001922285462,3.16776702607249,7.0860153459267));
#11696=CARTESIAN_POINT('Ctrl Pts',(0.503052557517713,3.18324609272907,7.09211530196098));
#11697=CARTESIAN_POINT('Ctrl Pts',(0.405105726564905,3.19872475896355,7.09821510019781));
#11698=CARTESIAN_POINT('Ctrl Pts',(0.30644272650644,3.20967864914956,7.10431489843464));
#11699=CARTESIAN_POINT('Ctrl Pts',(0.207519177167271,3.21606177701981,7.11041469667147));
#11700=CARTESIAN_POINT('Ctrl Pts',(0.104374329965198,3.22271728779804,7.11677478748205));
#11701=CARTESIAN_POINT('Ctrl Pts',(0.000946722460567373,3.22440320262582,
7.12313487829262));
#11702=CARTESIAN_POINT('Ctrl Pts',(-0.102245417469026,3.22112766544677,
7.1294949691032));
#11703=CARTESIAN_POINT('Ctrl Pts',(-0.201349360971802,3.21798189628495,
7.13560309013639));
#11704=CARTESIAN_POINT('Ctrl Pts',(-0.30023569264504,3.21026042906621,7.14171121116958));
#11705=CARTESIAN_POINT('Ctrl Pts',(-0.398450710501723,3.1980235449103,7.14781933220276));
#11706=CARTESIAN_POINT('Ctrl Pts',(-0.496732126942532,3.18577838796883,
7.15393158265116));
#11707=CARTESIAN_POINT('Ctrl Pts',(-0.594340891938124,3.16901181580139,
7.16004383309956));
#11708=CARTESIAN_POINT('Ctrl Pts',(-0.690834245690382,3.14783506675324,
7.16615608354795));
#11709=CARTESIAN_POINT('Ctrl Pts',(-0.787468407724652,3.12662741545602,
7.17227725332034));
#11710=CARTESIAN_POINT('Ctrl Pts',(-0.882983487642857,3.10099686775126,
7.17839842309272));
#11711=CARTESIAN_POINT('Ctrl Pts',(-0.976953019268458,3.07110409472591,
7.1845195928651));
#11712=CARTESIAN_POINT('Ctrl Pts',(-0.988293698477211,3.06749649613862,
7.18525832404286));
#11713=CARTESIAN_POINT('Ctrl Pts',(-0.99961189323101,3.0638268757802,7.18599705522062));
#11714=CARTESIAN_POINT('Ctrl Pts',(-1.01090687624163,3.06009556224432,7.18673578639837));
#11715=CARTESIAN_POINT('Ctrl Pts',(-1.10543852769614,3.02886689812778,7.19291848522568));
#11716=CARTESIAN_POINT('Ctrl Pts',(-1.19868177442532,2.99320091442327,7.19910118405298));
#11717=CARTESIAN_POINT('Ctrl Pts',(-1.29019080625755,2.95322285748104,7.20528388288029));
#11718=CARTESIAN_POINT('Ctrl Pts',(-1.3815790573384,2.9132975666938,7.21145842129987));
#11719=CARTESIAN_POINT('Ctrl Pts',(-1.47123725036822,2.86907168796002,7.21763295971945));
#11720=CARTESIAN_POINT('Ctrl Pts',(-1.55873551592881,2.82071997083761,7.22380749813904));
#11721=CARTESIAN_POINT('Ctrl Pts',(-1.64614388885164,2.77241792856721,7.22997569305522));
#11722=CARTESIAN_POINT('Ctrl Pts',(-1.73139636969943,2.71999868399673,7.23614388797139));
#11723=CARTESIAN_POINT('Ctrl Pts',(-1.81408470890849,2.66368433403893,7.24231208288757));
#11724=CARTESIAN_POINT('Ctrl Pts',(-1.89671587603632,2.60740892075128,7.24847601301207));
#11725=CARTESIAN_POINT('Ctrl Pts',(-1.97678606976541,2.54724399940528,7.25463994313658));
#11726=CARTESIAN_POINT('Ctrl Pts',(-2.05391399381773,2.48345623446432,7.26080387326108));
#11727=CARTESIAN_POINT('Ctrl Pts',(-2.13101448396032,2.41969115842374,7.26696561091502));
#11728=CARTESIAN_POINT('Ctrl Pts',(-2.20517445103947,2.35230607499375,7.27312734856897));
#11729=CARTESIAN_POINT('Ctrl Pts',(-2.2760445269573,2.28160883453052,7.27928908622291));
#11730=CARTESIAN_POINT('Ctrl Pts',(-2.34690816624739,2.21091801499761,7.28545026424981));
#11731=CARTESIAN_POINT('Ctrl Pts',(-2.41448220220194,2.13691594216141,7.29161144227671));
#11732=CARTESIAN_POINT('Ctrl Pts',(-2.47845380927167,2.05994763957892,7.2977726203036));
#11733=CARTESIAN_POINT('Ctrl Pts',(-2.54243655018751,1.98296594115918,7.30393487064384));
#11734=CARTESIAN_POINT('Ctrl Pts',(-2.60281534004262,1.90301732011431,7.31009712098408));
#11735=CARTESIAN_POINT('Ctrl Pts',(-2.65931799386684,1.82047943410412,7.31625937132433));
#11736=CARTESIAN_POINT('Ctrl Pts',(-2.71588198103346,1.73785195363984,7.32242831075587));
#11737=CARTESIAN_POINT('Ctrl Pts',(-2.76856118534086,1.65262995338251,7.32859725018741));
#11738=CARTESIAN_POINT('Ctrl Pts',(-2.81712715630606,1.56521952061139,7.33476618961895));
#11739=CARTESIAN_POINT('Ctrl Pts',(-2.86572077106075,1.47775933375208,7.34093864041574));
#11740=CARTESIAN_POINT('Ctrl Pts',(-2.9101962972974,1.38810862107274,7.34711109121254));
#11741=CARTESIAN_POINT('Ctrl Pts',(-2.9503725327185,1.296695600625,7.35328354200934));
#11742=CARTESIAN_POINT('Ctrl Pts',(-2.99061595500699,1.20512970984437,7.35946631501847));
#11743=CARTESIAN_POINT('Ctrl Pts',(-3.02654556955357,1.11179602839463,7.36564908802761));
#11744=CARTESIAN_POINT('Ctrl Pts',(-3.05802929386376,1.01714030515514,7.37183186103675));
#11745=CARTESIAN_POINT('Ctrl Pts',(-3.081515842817,0.946528065775037,7.37644414894511));
#11746=CARTESIAN_POINT('Ctrl Pts',(-3.10252928054058,0.875180462760919,
7.38105643685346));
#11747=CARTESIAN_POINT('Ctrl Pts',(-3.1210333525377,0.803285985715719,7.38566872476182));
#11748=CARTESIAN_POINT('Ctrl Pts',(-3.14576188247488,0.707207418349198,
7.39183250858402));
#11749=CARTESIAN_POINT('Ctrl Pts',(-3.16609437828951,0.609812275758225,
7.39799629240622));
#11750=CARTESIAN_POINT('Ctrl Pts',(-3.18189322309051,0.51153990983176,7.40416007622841));
#11751=CARTESIAN_POINT('Ctrl Pts',(-3.19767035311234,0.413402614712841,
7.41031538821572));
#11752=CARTESIAN_POINT('Ctrl Pts',(-3.20892614793691,0.314390918801613,
7.41647070020303));
#11753=CARTESIAN_POINT('Ctrl Pts',(-3.21557314781084,0.214957887917286,
7.42262601219034));
#11754=CARTESIAN_POINT('Ctrl Pts',(-3.22221299064851,0.115631919741172,
7.42877469655738));
#11755=CARTESIAN_POINT('Ctrl Pts',(-3.2242538746182,0.0158859507229964,
7.43492338092442));
#11756=CARTESIAN_POINT('Ctrl Pts',(-3.22165980543998,-0.0838192132654753,
7.44107206529145));
#11757=CARTESIAN_POINT('Ctrl Pts',(-3.21906768223833,-0.183449582057625,
7.44721613713858));
#11758=CARTESIAN_POINT('Ctrl Pts',(-3.21184752969372,-0.283038772450925,
7.4533602089857));
#11759=CARTESIAN_POINT('Ctrl Pts',(-3.20001540502417,-0.382124286205456,
7.45950428083282));
#11760=CARTESIAN_POINT('Ctrl Pts',(-3.18818790171217,-0.481171099422168,
7.46564595294586));
#11761=CARTESIAN_POINT('Ctrl Pts',(-3.17175205680164,-0.579714194694247,
7.47178762505889));
#11762=CARTESIAN_POINT('Ctrl Pts',(-3.15077585500389,-0.677295411194052,
7.47792929717193));
#11763=CARTESIAN_POINT('Ctrl Pts',(-3.1298021927133,-0.774864813915528,
7.48407022573661));
#11764=CARTESIAN_POINT('Ctrl Pts',(-3.10428935783583,-0.871472143348168,
7.49021115430129));
#11765=CARTESIAN_POINT('Ctrl Pts',(-3.07435640514299,-0.966669672978465,
7.49635208286598));
#11766=CARTESIAN_POINT('Ctrl Pts',(-3.04441900906306,-1.06188133417401,
7.50249392301873));
#11767=CARTESIAN_POINT('Ctrl Pts',(-3.010060322785,-1.15568236421211,7.50863576317149));
#11768=CARTESIAN_POINT('Ctrl Pts',(-2.97144888083816,-1.24764141926504,
7.51477760332424));
#11769=CARTESIAN_POINT('Ctrl Pts',(-2.93279616806333,-1.33969876710763,
7.52092600834005));
#11770=CARTESIAN_POINT('Ctrl Pts',(-2.8898817913854,-1.42990980580736,7.52707441335585));
#11771=CARTESIAN_POINT('Ctrl Pts',(-2.84292190183757,-1.51786449413386,
7.53322281837165));
#11772=CARTESIAN_POINT('Ctrl Pts',(-2.79593596524847,-1.60586796791149,
7.53937463369699));
#11773=CARTESIAN_POINT('Ctrl Pts',(-2.74490027030643,-1.69161222466882,
7.54552644902233));
#11774=CARTESIAN_POINT('Ctrl Pts',(-2.69007518096602,-1.77471493013685,
7.55167826434767));
#11775=CARTESIAN_POINT('Ctrl Pts',(-2.63515766627508,-1.85795773198731,
7.55784045053961));
#11776=CARTESIAN_POINT('Ctrl Pts',(-2.57643825363058,-1.93854973511658,
7.56400263673155));
#11777=CARTESIAN_POINT('Ctrl Pts',(-2.51421866168475,-2.01614039286359,
7.57016482292349));
#11778=CARTESIAN_POINT('Ctrl Pts',(-2.46562907143422,-2.07673381929555,
7.57497710299074));
#11779=CARTESIAN_POINT('Ctrl Pts',(-2.4149057024178,-2.13549746859355,7.579789383058));
#11780=CARTESIAN_POINT('Ctrl Pts',(-2.36220738045403,-2.19228051449364,
7.58460166312525));
#11781=CARTESIAN_POINT('Ctrl Pts',(-2.29461677109524,-2.26511017074482,
7.59077386994381));
#11782=CARTESIAN_POINT('Ctrl Pts',(-2.22353619037049,-2.33493893300441,
7.59694607676236));
#11783=CARTESIAN_POINT('Ctrl Pts',(-2.14926265549304,-2.40141366703094,
7.60311828358091));
#11784=CARTESIAN_POINT('Ctrl Pts',(-2.07507717426126,-2.46780959313907,
7.60928317305132));
#11785=CARTESIAN_POINT('Ctrl Pts',(-1.9977065768573,-2.53085910109103,7.61544806252174));
#11786=CARTESIAN_POINT('Ctrl Pts',(-1.91748654889088,-2.59024379109816,
7.62161295199215));
#11787=CARTESIAN_POINT('Ctrl Pts',(-1.83735475836048,-2.64956316134764,
7.62777106043725));
#11788=CARTESIAN_POINT('Ctrl Pts',(-1.75438011671107,-2.70522547284929,
7.63392916888235));
#11789=CARTESIAN_POINT('Ctrl Pts',(-1.66893246721288,-2.75695157418166,
7.64008727732745));
#11790=CARTESIAN_POINT('Ctrl Pts',(-1.60567441703572,-2.79524510633577,
7.64464620826709));
#11791=CARTESIAN_POINT('Ctrl Pts',(-1.54106175878119,-2.831382116787,7.64920513920673));
#11792=CARTESIAN_POINT('Ctrl Pts',(-1.47525540501185,-2.86526422036142,
7.65376407014636));
#11793=CARTESIAN_POINT('',(-1.87158653173903,2.62360084935058,7.));
#11794=CARTESIAN_POINT('Origin',(0.,0.,7.));
#11795=CARTESIAN_POINT('Ctrl Pts',(-1.87158653173896,2.62360084935063,7.));
#11796=CARTESIAN_POINT('Ctrl Pts',(-1.95488455526994,2.56417890679422,7.00631636296639));
#11797=CARTESIAN_POINT('Ctrl Pts',(-2.0354058791132,2.50074665614785,7.01263272593278));
#11798=CARTESIAN_POINT('Ctrl Pts',(-2.11275911458763,2.43359127345306,7.01894908889917));
#11799=CARTESIAN_POINT('Ctrl Pts',(-2.19006764871673,2.3664746989081,7.02526180172836));
#11800=CARTESIAN_POINT('Ctrl Pts',(-2.26421143417526,2.29563954104779,7.03157451455755));
#11801=CARTESIAN_POINT('Ctrl Pts',(-2.33483186844915,2.2214134483644,7.03788722738675));
#11802=CARTESIAN_POINT('Ctrl Pts',(-2.40542791175611,2.14721299197442,7.04419775992391));
#11803=CARTESIAN_POINT('Ctrl Pts',(-2.47250274843121,2.06962422637506,7.05050829246107));
#11804=CARTESIAN_POINT('Ctrl Pts',(-2.53573481925193,1.98901143509367,7.05681882499824));
#11805=CARTESIAN_POINT('Ctrl Pts',(-2.59897761335262,1.9083849730038,7.06313042771397));
#11806=CARTESIAN_POINT('Ctrl Pts',(-2.65837608332418,1.82473377464521,7.0694420304297));
#11807=CARTESIAN_POINT('Ctrl Pts',(-2.71364928332791,1.73845481091512,7.07575363314544));
#11808=CARTESIAN_POINT('Ctrl Pts',(-2.7689307737664,1.65216290619155,7.08206618253932));
#11809=CARTESIAN_POINT('Ctrl Pts',(-2.82008554331845,1.5632427926457,7.0883787319332));
#11810=CARTESIAN_POINT('Ctrl Pts',(-2.86687682085001,1.47211917200102,7.09469128132708));
#11811=CARTESIAN_POINT('Ctrl Pts',(-2.9136850090638,1.38096261866729,7.10100611211875));
#11812=CARTESIAN_POINT('Ctrl Pts',(-2.95612638052977,1.28760133341672,7.10732094291041));
#11813=CARTESIAN_POINT('Ctrl Pts',(-2.99401111992302,1.19248269433031,7.11363577370208));
#11814=CARTESIAN_POINT('Ctrl Pts',(-3.03191756464926,1.09730955884861,7.11995422245462));
#11815=CARTESIAN_POINT('Ctrl Pts',(-3.06526203005559,1.00037744137021,7.12627267120716));
#11816=CARTESIAN_POINT('Ctrl Pts',(-3.09390384883166,0.902151060900918,
7.13259111995971));
#11817=CARTESIAN_POINT('Ctrl Pts',(-3.12258819884177,0.803778820658934,
7.13891895119682));
#11818=CARTESIAN_POINT('Ctrl Pts',(-3.14655584252349,0.704108868842967,
7.14524678243393));
#11819=CARTESIAN_POINT('Ctrl Pts',(-3.16571666474431,0.603618721595178,
7.15157461367104));
#11820=CARTESIAN_POINT('Ctrl Pts',(-3.18489319973714,0.503046167718055,
7.15790763402626));
#11821=CARTESIAN_POINT('Ctrl Pts',(-3.19925499963053,0.401652478673659,
7.16424065438148));
#11822=CARTESIAN_POINT('Ctrl Pts',(-3.20876377075636,0.299921032909348,
7.17057367473671));
#11823=CARTESIAN_POINT('Ctrl Pts',(-3.21828938395578,0.198009398930137,
7.1769179122296));
#11824=CARTESIAN_POINT('Ctrl Pts',(-3.22294477780767,0.0957592177962029,
7.1832621497225));
#11825=CARTESIAN_POINT('Ctrl Pts',(-3.22274375398103,-0.00634497251973922,
7.18960638721539));
#11826=CARTESIAN_POINT('Ctrl Pts',(-3.22264524679225,-0.056378826311069,
7.19271523759807));
#11827=CARTESIAN_POINT('Ctrl Pts',(-3.22138137649325,-0.106377683652681,
7.19582408798075));
#11828=CARTESIAN_POINT('Ctrl Pts',(-3.21895829870692,-0.156285103851417,
7.19893293836343));
#11829=CARTESIAN_POINT('Ctrl Pts',(-3.2141962974436,-0.254366642701122,
7.20504266770573));
#11830=CARTESIAN_POINT('Ctrl Pts',(-3.20493703544895,-0.352439736616328,
7.21115239704804));
#11831=CARTESIAN_POINT('Ctrl Pts',(-3.19117079167538,-0.450051709093428,
7.21726212639034));
#11832=CARTESIAN_POINT('Ctrl Pts',(-3.17742529840946,-0.547516546446787,
7.22336264624983));
#11833=CARTESIAN_POINT('Ctrl Pts',(-3.15918637904269,-0.644521208194034,
7.22946316610932));
#11834=CARTESIAN_POINT('Ctrl Pts',(-3.13649628481895,-0.740613676498684,
7.2355636859688));
#11835=CARTESIAN_POINT('Ctrl Pts',(-3.11383333468033,-0.836591189699454,
7.24165690779644));
#11836=CARTESIAN_POINT('Ctrl Pts',(-3.08672989080458,-0.931658248347009,
7.24775012962408));
#11837=CARTESIAN_POINT('Ctrl Pts',(-3.05527977719574,-1.0253697116449,7.25384335145172));
#11838=CARTESIAN_POINT('Ctrl Pts',(-3.02385762985271,-1.11899784425202,
7.25993115502672));
#11839=CARTESIAN_POINT('Ctrl Pts',(-2.98809663559724,-1.21127235777711,
7.26601895860171));
#11840=CARTESIAN_POINT('Ctrl Pts',(-2.94814103357299,-1.30176111812543,
7.27210676217671));
#11841=CARTESIAN_POINT('Ctrl Pts',(-2.90820437617437,-1.39220697395969,
7.27819167926886));
#11842=CARTESIAN_POINT('Ctrl Pts',(-2.86407723941635,-1.48086835208181,
7.28427659636101));
#11843=CARTESIAN_POINT('Ctrl Pts',(-2.81595244431603,-1.56733193480212,
7.29036151345317));
#11844=CARTESIAN_POINT('Ctrl Pts',(-2.76783693766769,-1.65377882939245,
7.29644525610998));
#11845=CARTESIAN_POINT('Ctrl Pts',(-2.71572552160548,-1.73802838303165,
7.30252899876679));
#11846=CARTESIAN_POINT('Ctrl Pts',(-2.65985700406729,-1.81969180918478,
7.3086127414236));
#11847=CARTESIAN_POINT('Ctrl Pts',(-2.60398356273015,-1.90136243249132,
7.31469702025225));
#11848=CARTESIAN_POINT('Ctrl Pts',(-2.5443526141527,-1.98044610937609,7.32078129908089));
#11849=CARTESIAN_POINT('Ctrl Pts',(-2.48124567103609,-2.05658393518589,
7.32686557790954));
#11850=CARTESIAN_POINT('Ctrl Pts',(-2.41807320159362,-2.1328008177799,7.33295617427502));
#11851=CARTESIAN_POINT('Ctrl Pts',(-2.35141781427544,-2.2060653980937,7.33904677064049));
#11852=CARTESIAN_POINT('Ctrl Pts',(-2.28160046354572,-2.27605291837601,
7.34513736700596));
#11853=CARTESIAN_POINT('Ctrl Pts',(-2.21174675054973,-2.34607688955228,
7.35123113547528));
#11854=CARTESIAN_POINT('Ctrl Pts',(-2.13872812446055,-2.41282010374611,
7.35732490394461));
#11855=CARTESIAN_POINT('Ctrl Pts',(-2.06289978202659,-2.47599718332123,
7.36341867241393));
#11856=CARTESIAN_POINT('Ctrl Pts',(-1.9869397203935,-2.53928400595624,7.36952302619049));
#11857=CARTESIAN_POINT('Ctrl Pts',(-1.90816054833947,-2.59899205243666,
7.37562737996706));
#11858=CARTESIAN_POINT('Ctrl Pts',(-1.82694775631032,-2.65487842625848,
7.38173173374362));
#11859=CARTESIAN_POINT('Ctrl Pts',(-1.75539779668978,-2.70411534682703,
7.38710978140471));
#11860=CARTESIAN_POINT('Ctrl Pts',(-1.68195947092443,-2.75038647700699,
7.39248782906579));
#11861=CARTESIAN_POINT('Ctrl Pts',(-1.6069110018128,-2.79355590507027,7.39786587672688));
#11862=CARTESIAN_POINT('Ctrl Pts',(-1.56362614533898,-2.81845424769998,
7.40096771243219));
#11863=CARTESIAN_POINT('Ctrl Pts',(-1.51972485578459,-2.84236797325646,
7.4040695481375));
#11864=CARTESIAN_POINT('Ctrl Pts',(-1.47525540501185,-2.86526422036142,
7.40717138384282));
#11865=CARTESIAN_POINT('Origin',(0.,0.,4.68922655072688));
#11866=CARTESIAN_POINT('',(-1.47525556020637,-2.8652641404555,8.90579936292296));
#11867=CARTESIAN_POINT('',(-1.47525540497551,-2.86526422038013,8.65558740743848));
#11868=CARTESIAN_POINT('',(-1.47525540501186,-2.86526422036142,4.68922655072688));
#11869=CARTESIAN_POINT('',(3.22274949386856,-0.00180617550826221,8.06077344923593));
#11870=CARTESIAN_POINT('Ctrl Pts',(-1.47525556020637,-2.8652641404555,8.90579936292296));
#11871=CARTESIAN_POINT('Ctrl Pts',(-1.56191584290783,-2.82064484616451,
8.9001782983926));
#11872=CARTESIAN_POINT('Ctrl Pts',(-1.64653192564077,-2.77210432391562,
8.89445384481769));
#11873=CARTESIAN_POINT('Ctrl Pts',(-1.74732582984747,-2.70803429645877,
8.88727024250858));
#11874=CARTESIAN_POINT('Ctrl Pts',(-1.76568991081099,-2.69609651330088,
8.88594609824383));
#11875=CARTESIAN_POINT('Ctrl Pts',(-1.79483672095497,-2.67672378086745,
8.88381910504022));
#11876=CARTESIAN_POINT('Ctrl Pts',(-1.80569848880261,-2.66940855126029,
8.88302075531027));
#11877=CARTESIAN_POINT('Ctrl Pts',(-1.82484375429939,-2.65634419792067,
8.88160326897679));
#11878=CARTESIAN_POINT('Ctrl Pts',(-1.83314546940875,-2.65062198544963,
8.88098516116634));
#11879=CARTESIAN_POINT('Ctrl Pts',(-1.85032771157253,-2.63865926721531,
8.87969856997363));
#11880=CARTESIAN_POINT('Ctrl Pts',(-1.85920382696431,-2.63241267544839,
8.87902985821276));
#11881=CARTESIAN_POINT('Ctrl Pts',(-1.88205101427809,-2.61616070584337,
8.8772979262051));
#11882=CARTESIAN_POINT('Ctrl Pts',(-1.89597378050373,-2.60608830708994,
8.87623212468758));
#11883=CARTESIAN_POINT('Ctrl Pts',(-1.95505444363666,-2.56262248890407,
8.87166432267757));
#11884=CARTESIAN_POINT('Ctrl Pts',(-1.99941353186853,-2.52816470714099,
8.86812089055773));
#11885=CARTESIAN_POINT('Ctrl Pts',(-2.11406016631624,-2.43420311009594,
8.85865041136447));
#11886=CARTESIAN_POINT('Ctrl Pts',(-2.18273299514682,-2.37281885265166,
8.85265147681694));
#11887=CARTESIAN_POINT('Ctrl Pts',(-2.42137386943083,-2.14037036060827,
8.83061161306671));
#11888=CARTESIAN_POINT('Ctrl Pts',(-2.57463129709393,-1.95332937520388,
8.81403486023412));
#11889=CARTESIAN_POINT('Ctrl Pts',(-2.75636266549661,-1.67251703985024,
8.7917698958822));
#11890=CARTESIAN_POINT('Ctrl Pts',(-2.8036990385628,-1.59189310158585,8.78565022208224));
#11891=CARTESIAN_POINT('Ctrl Pts',(-2.85401455155441,-1.49696822750696,
8.77884472223392));
#11892=CARTESIAN_POINT('Ctrl Pts',(-2.86048042076661,-1.48457560053888,
8.77796386642576));
#11893=CARTESIAN_POINT('Ctrl Pts',(-2.87010281165793,-1.46583683795933,
8.77664381755683));
#11894=CARTESIAN_POINT('Ctrl Pts',(-2.87331926374573,-1.45952190660949,
8.77620098354383));
#11895=CARTESIAN_POINT('Ctrl Pts',(-2.87903262519064,-1.44821265074036,
8.77541159855454));
#11896=CARTESIAN_POINT('Ctrl Pts',(-2.88153740232486,-1.44322241504034,
8.77506455854859));
#11897=CARTESIAN_POINT('Ctrl Pts',(-2.88692943479051,-1.43240993911197,
8.77431538984498));
#11898=CARTESIAN_POINT('Ctrl Pts',(-2.88981204413429,-1.42658548515855,
8.77391355269614));
#11899=CARTESIAN_POINT('Ctrl Pts',(-2.89780797274013,-1.41030563167213,
8.77279507804597));
#11900=CARTESIAN_POINT('Ctrl Pts',(-2.9028823626142,-1.39983106840124,8.77208083164053));
#11901=CARTESIAN_POINT('Ctrl Pts',(-2.93194065425306,-1.33901134734256,
8.76796342033422));
#11902=CARTESIAN_POINT('Ctrl Pts',(-2.95467294484771,-1.28807455059822,
8.76463287007666));
#11903=CARTESIAN_POINT('Ctrl Pts',(-3.07368517942321,-1.00164584814562,
8.74641373676251));
#11904=CARTESIAN_POINT('Ctrl Pts',(-3.14314712502643,-0.755968689147023,
8.73260956516305));
#11905=CARTESIAN_POINT('Ctrl Pts',(-3.20868236742669,-0.342622672841557,
8.70897172935884));
#11906=CARTESIAN_POINT('Ctrl Pts',(-3.22195949021845,-0.178883766546193,
8.69951858710015));
#11907=CARTESIAN_POINT('Ctrl Pts',(-3.22281676813793,0.00705201471682277,
8.68833510825207));
#11908=CARTESIAN_POINT('Ctrl Pts',(-3.22269433460698,0.0289627566378994,
8.68701050324264));
#11909=CARTESIAN_POINT('Ctrl Pts',(-3.22214176634534,0.0639649697824238,
8.68488298994749));
#11910=CARTESIAN_POINT('Ctrl Pts',(-3.22185522579968,0.077058262542411,
8.68408458647804));
#11911=CARTESIAN_POINT('Ctrl Pts',(-3.22120688608411,0.100226709786385,
8.68266713820439));
#11912=CARTESIAN_POINT('Ctrl Pts',(-3.22087760048591,0.110302653321238,
8.68204912320675));
#11913=CARTESIAN_POINT('Ctrl Pts',(-3.22009577069156,0.131219339565238,
8.6807628592837));
#11914=CARTESIAN_POINT('Ctrl Pts',(-3.21963574586003,0.142059659550053,
8.68009438268703));
#11915=CARTESIAN_POINT('Ctrl Pts',(-3.21830622391815,0.170051591003138,
8.67836335015214));
#11916=CARTESIAN_POINT('Ctrl Pts',(-3.21735436256677,0.187198776119536,
8.67729821653906));
#11917=CARTESIAN_POINT('Ctrl Pts',(-3.21270939306384,0.260310524804873,
8.67273594273521));
#11918=CARTESIAN_POINT('Ctrl Pts',(-3.2076929140099,0.316178343891641,8.66919748290491));
#11919=CARTESIAN_POINT('Ctrl Pts',(-3.19061669986576,0.463172367564257,
8.65974328643643));
#11920=CARTESIAN_POINT('Ctrl Pts',(-3.17611271358921,0.553957650238664,
8.65375594827045));
#11921=CARTESIAN_POINT('Ctrl Pts',(-3.10920634554157,0.882025980317213,
8.6316064529134));
#11922=CARTESIAN_POINT('Ctrl Pts',(-3.03390974688837,1.11378210204861,8.61489679298693));
#11923=CARTESIAN_POINT('Ctrl Pts',(-2.89521884214251,1.41854780620448,8.59262025619512));
#11924=CARTESIAN_POINT('Ctrl Pts',(-2.85357089629121,1.50056874902238,8.58660221977168));
#11925=CARTESIAN_POINT('Ctrl Pts',(-2.8016373262799,1.59284017043318,8.57989545603576));
#11926=CARTESIAN_POINT('Ctrl Pts',(-2.79472775553292,1.60493249250087,8.57901783707648));
#11927=CARTESIAN_POINT('Ctrl Pts',(-2.7841899060956,1.62310017847586,8.57770171879629));
#11928=CARTESIAN_POINT('Ctrl Pts',(-2.78061975809547,1.62920882201503,8.57725960889085));
#11929=CARTESIAN_POINT('Ctrl Pts',(-2.7741968489609,1.64011602286669,8.57647102342865));
#11930=CARTESIAN_POINT('Ctrl Pts',(-2.77135172105746,1.64491895393319,8.57612406289979));
#11931=CARTESIAN_POINT('Ctrl Pts',(-2.76516336600325,1.65530403772327,8.57537448757764));
#11932=CARTESIAN_POINT('Ctrl Pts',(-2.76181571951796,1.66088344900567,8.57497216742491));
#11933=CARTESIAN_POINT('Ctrl Pts',(-2.75241477797755,1.67644466924457,8.5738510626584));
#11934=CARTESIAN_POINT('Ctrl Pts',(-2.74632403864026,1.68640390285786,8.5731346869855));
#11935=CARTESIAN_POINT('Ctrl Pts',(-2.71052735340222,1.74422834313809,8.56898062799087));
#11936=CARTESIAN_POINT('Ctrl Pts',(-2.67962257809606,1.79134440601588,8.56561707103738));
#11937=CARTESIAN_POINT('Ctrl Pts',(-2.50268463307353,2.04626120634536,8.5473967484244));
#11938=CARTESIAN_POINT('Ctrl Pts',(-2.33370664075608,2.23706410608582,8.53361490966403));
#11939=CARTESIAN_POINT('Ctrl Pts',(-2.02173041204856,2.51506888703168,8.5100121280717));
#11940=CARTESIAN_POINT('Ctrl Pts',(-1.89128091654333,2.6145767194305,8.500570419313));
#11941=CARTESIAN_POINT('Ctrl Pts',(-1.73542694140845,2.71567537702212,8.4893971628286));
#11942=CARTESIAN_POINT('Ctrl Pts',(-1.71688965944886,2.7274327275099,8.4880701397851));
#11943=CARTESIAN_POINT('Ctrl Pts',(-1.68709247569136,2.74590757242795,8.48593940595385));
#11944=CARTESIAN_POINT('Ctrl Pts',(-1.67590897860193,2.75274744670181,8.48514022015577));
#11945=CARTESIAN_POINT('Ctrl Pts',(-1.65604900630699,2.76472800709805,8.48372177974039));
#11946=CARTESIAN_POINT('Ctrl Pts',(-1.64738949897839,2.76989658642821,8.48310355871688));
#11947=CARTESIAN_POINT('Ctrl Pts',(-1.6293656110088,2.78054004333162,8.48181726080737));
#11948=CARTESIAN_POINT('Ctrl Pts',(-1.61999757476011,2.78600844939026,8.48114895817598));
#11949=CARTESIAN_POINT('Ctrl Pts',(-1.595742730712,2.80000303766307,8.47941922239956));
#11950=CARTESIAN_POINT('Ctrl Pts',(-1.58081527599739,2.80845774730057,8.47835522021374));
#11951=CARTESIAN_POINT('Ctrl Pts',(-1.51695785188169,2.84395532250318,8.47380537636145));
#11952=CARTESIAN_POINT('Ctrl Pts',(-1.46739859746591,2.8698403658216,8.47027850670192));
#11953=CARTESIAN_POINT('Ctrl Pts',(-1.33502721792961,2.93465325805991,8.46086327890989));
#11954=CARTESIAN_POINT('Ctrl Pts',(-1.25119176427262,2.97136401321875,8.45490407314585));
#11955=CARTESIAN_POINT('Ctrl Pts',(-0.936264577472805,3.09357516656347,
8.43256166640414));
#11956=CARTESIAN_POINT('Ctrl Pts',(-0.6971794875072,3.15606145360958,8.41560900263179));
#11957=CARTESIAN_POINT('Ctrl Pts',(-0.364938512903642,3.2032650890367,8.39330593887493));
#11958=CARTESIAN_POINT('Ctrl Pts',(-0.276059656320446,3.21214594500282,
8.38746816700556));
#11959=CARTESIAN_POINT('Ctrl Pts',(-0.173104642769638,3.21812737713856,
8.38093662225614));
#11960=CARTESIAN_POINT('Ctrl Pts',(-0.15928533661647,3.21884097627461,8.38006471914973));
#11961=CARTESIAN_POINT('Ctrl Pts',(-0.138411284595818,3.21978410562802,
8.37875539607126));
#11962=CARTESIAN_POINT('Ctrl Pts',(-0.131359887447836,3.22007949479204,
8.3783144214118));
#11963=CARTESIAN_POINT('Ctrl Pts',(-0.118728067577128,3.22056709057461,
8.37752690212941));
#11964=CARTESIAN_POINT('Ctrl Pts',(-0.113148088982313,3.22076795972613,
8.37717988007813));
#11965=CARTESIAN_POINT('Ctrl Pts',(-0.101044665211502,3.22117216750185,
8.3764290261362));
#11966=CARTESIAN_POINT('Ctrl Pts',(-0.0945211362517755,3.22137019195878,
8.37602549523407));
#11967=CARTESIAN_POINT('Ctrl Pts',(-0.0762496291795751,3.22186928037541,
8.37489841368772));
#11968=CARTESIAN_POINT('Ctrl Pts',(-0.0645003978578495,3.22212590914076,
8.37417730976002));
#11969=CARTESIAN_POINT('Ctrl Pts',(0.00478784292492184,3.2232601676578,
8.3699449147229));
#11970=CARTESIAN_POINT('Ctrl Pts',(0.0623445902081485,3.22266087779381,
8.36651097389545));
#11971=CARTESIAN_POINT('Ctrl Pts',(0.373118292862246,3.2110947857646,8.34826455816404));
#11972=CARTESIAN_POINT('Ctrl Pts',(0.624405016901019,3.17182785454008,8.33450906399677));
#11973=CARTESIAN_POINT('Ctrl Pts',(1.02520605030147,3.0596642465497,8.31099204798635));
#11974=CARTESIAN_POINT('Ctrl Pts',(1.17833211311284,3.00401663105659,8.30161245074197));
#11975=CARTESIAN_POINT('Ctrl Pts',(1.34658173339306,2.9280226026677,8.29050848005503));
#11976=CARTESIAN_POINT('Ctrl Pts',(1.36647949825128,2.91878955577153,8.28918239150363));
#11977=CARTESIAN_POINT('Ctrl Pts',(1.39811371285924,2.90371613764046,8.28705272567481));
#11978=CARTESIAN_POINT('Ctrl Pts',(1.40991169001187,2.89800593175453,8.28625366187736));
#11979=CARTESIAN_POINT('Ctrl Pts',(1.4307272707706,2.88777402099146,8.28483517354185));
#11980=CARTESIAN_POINT('Ctrl Pts',(1.43975914542981,2.88328162327544,8.28421678052989));
#11981=CARTESIAN_POINT('Ctrl Pts',(1.44894556310741,2.87865842996574,8.28358479724617));
#11982=CARTESIAN_POINT('Ctrl Pts',(1.44912141895466,2.87856990785151,8.28357269804586));
#11983=CARTESIAN_POINT('Ctrl Pts',(1.44949010197805,2.87838427826791,8.28354732962392));
#11984=CARTESIAN_POINT('Ctrl Pts',(1.44968292750618,2.87828716753724,8.28353406028741));
#11985=CARTESIAN_POINT('Ctrl Pts',(1.45004265414901,2.87810595680168,8.28350930307968));
#11986=CARTESIAN_POINT('Ctrl Pts',(1.45020955742023,2.87802186179936,8.2834978153999));
#11987=CARTESIAN_POINT('Ctrl Pts',(1.45052089772116,2.87786495755752,8.28347638445922));
#11988=CARTESIAN_POINT('Ctrl Pts',(1.45066533754033,2.87779215148027,8.28346644126128));
#11989=CARTESIAN_POINT('Ctrl Pts',(1.45093475823428,2.8776563223289,8.28344789299351));
#11990=CARTESIAN_POINT('Ctrl Pts',(1.45105974175618,2.87759330134494,8.28343928793259));
#11991=CARTESIAN_POINT('Ctrl Pts',(1.45129286049334,2.87747573582274,8.28342323674557));
#11992=CARTESIAN_POINT('Ctrl Pts',(1.45140099837991,2.87742119250351,8.28341579057875));
#11993=CARTESIAN_POINT('Ctrl Pts',(1.45160268999296,2.87731944766031,8.28340190168581));
#11994=CARTESIAN_POINT('Ctrl Pts',(1.45169624646475,2.87727224667359,8.2833954588779));
#11995=CARTESIAN_POINT('Ctrl Pts',(1.45189715079337,2.87717087439633,8.28338162282568));
#11996=CARTESIAN_POINT('Ctrl Pts',(1.45200450021031,2.87711670050562,8.28337422937272));
#11997=CARTESIAN_POINT('Ctrl Pts',(1.4522157160377,2.87701009559024,8.28335968152221));
#11998=CARTESIAN_POINT('Ctrl Pts',(1.45231957730882,2.87695766764132,8.28335252750566));
#11999=CARTESIAN_POINT('Ctrl Pts',(1.4525239278985,2.87685449997981,8.28333845095853));
#12000=CARTESIAN_POINT('Ctrl Pts',(1.45262441808936,2.87680376027666,8.28333152839296));
#12001=CARTESIAN_POINT('Ctrl Pts',(1.45282214130987,2.8767039124812,8.28331790691457));
#12002=CARTESIAN_POINT('Ctrl Pts',(1.45291937533058,2.87665480430889,8.28331120795692));
#12003=CARTESIAN_POINT('Ctrl Pts',(1.45311069710945,2.87655816481374,8.28329802612367));
#12004=CARTESIAN_POINT('Ctrl Pts',(1.45320478592302,2.87651063335084,8.28329154319727));
#12005=CARTESIAN_POINT('Ctrl Pts',(1.45338992424005,2.87641709441151,8.28327878612238));
#12006=CARTESIAN_POINT('Ctrl Pts',(1.45348097490983,2.87637108671325,8.28327251191403));
#12007=CARTESIAN_POINT('Ctrl Pts',(1.45366014024989,2.8762805441915,8.28326016521712));
#12008=CARTESIAN_POINT('Ctrl Pts',(1.45374825613992,2.87623600909513,8.28325409266368));
#12009=CARTESIAN_POINT('Ctrl Pts',(1.45392165144414,2.87614836249648,8.28324214247482));
#12010=CARTESIAN_POINT('Ctrl Pts',(1.45400693222277,2.87610525062572,8.28323626476329));
#12011=CARTESIAN_POINT('Ctrl Pts',(1.45417475348336,2.87602040281084,8.28322469768269));
#12012=CARTESIAN_POINT('Ctrl Pts',(1.45425729537493,2.8759786664544,8.28321900823322));
#12013=CARTESIAN_POINT('Ctrl Pts',(1.45441973144542,2.87589652374621,8.28320781134494));
#12014=CARTESIAN_POINT('Ctrl Pts',(1.45449962719732,2.8758561168799,8.28320230381336));
#12015=CARTESIAN_POINT('Ctrl Pts',(1.45465686045572,2.87577658873875,8.28319146464015));
#12016=CARTESIAN_POINT('Ctrl Pts',(1.45473419958992,2.87573746690334,8.28318613290095));
#12017=CARTESIAN_POINT('Ctrl Pts',(1.45488639914185,2.87566046937528,8.28317563987343));
#12018=CARTESIAN_POINT('Ctrl Pts',(1.45496126132407,2.87562259303767,8.28317047847757));
#12019=CARTESIAN_POINT('Ctrl Pts',(1.45510862278797,2.87554802863505,8.28316031819173));
#12020=CARTESIAN_POINT('Ctrl Pts',(1.45518110393332,2.87551134997834,8.28315532056545));
#12021=CARTESIAN_POINT('Ctrl Pts',(1.45532375933505,2.87543915327744,8.28314548399554));
#12022=CARTESIAN_POINT('Ctrl Pts',(1.45539393367991,2.87540363540385,8.28314064505787));
#12023=CARTESIAN_POINT('Ctrl Pts',(1.45553205290674,2.87533372172008,8.28313112056191));
#12024=CARTESIAN_POINT('Ctrl Pts',(1.4555999978773,2.87529932606662,8.28312643500879));
#12025=CARTESIAN_POINT('Ctrl Pts',(1.45573373307805,2.87523161959461,8.28311721216244));
#12026=CARTESIAN_POINT('Ctrl Pts',(1.45579952336763,2.87519830893463,8.28311267487567));
#12027=CARTESIAN_POINT('Ctrl Pts',(1.46613360586299,2.86996555454922,8.28239995060537));
#12028=CARTESIAN_POINT('Ctrl Pts',(1.47637386319367,2.86471119750456,8.28168983009041));
#12029=CARTESIAN_POINT('Ctrl Pts',(1.50475679532078,2.84995508509782,8.27971069068866));
#12030=CARTESIAN_POINT('Ctrl Pts',(1.52283712778484,2.84033520048992,8.27843749813012));
#12031=CARTESIAN_POINT('Ctrl Pts',(1.56296807023564,2.81848967122392,8.27558316607803));
#12032=CARTESIAN_POINT('Ctrl Pts',(1.58496918684809,2.80617637255745,8.2739989539887));
#12033=CARTESIAN_POINT('Ctrl Pts',(1.65276816168936,2.76717984313757,8.26905574579382));
#12034=CARTESIAN_POINT('Ctrl Pts',(1.69805201947264,2.73962510128927,8.26566605775303));
#12035=CARTESIAN_POINT('Ctrl Pts',(1.87539698758895,2.62562619239151,8.25203372394604));
#12036=CARTESIAN_POINT('Ctrl Pts',(2.0016968561666,2.53065724137172,8.24150173867995));
#12037=CARTESIAN_POINT('Ctrl Pts',(2.2905503527454,2.27826241015908,8.21559746268043));
#12038=CARTESIAN_POINT('Ctrl Pts',(2.44450735163029,2.11222615715828,8.20014330439292));
#12039=CARTESIAN_POINT('Ctrl Pts',(2.59410994337361,1.91240093692607,8.18417037034958));
#12040=CARTESIAN_POINT('Ctrl Pts',(2.6081595136398,1.89319512243291,8.18265991212846));
#12041=CARTESIAN_POINT('Ctrl Pts',(2.62719646252656,1.86655734461766,8.1806007276607));
#12042=CARTESIAN_POINT('Ctrl Pts',(2.63236712616528,1.85925815610738,8.18004012148366));
#12043=CARTESIAN_POINT('Ctrl Pts',(2.64056224724243,1.84758676151705,8.1791496302794));
#12044=CARTESIAN_POINT('Ctrl Pts',(2.64360634652024,1.84322850143718,8.17881841561658));
#12045=CARTESIAN_POINT('Ctrl Pts',(2.64989274381402,1.83418061082435,8.1781335415127));
#12046=CARTESIAN_POINT('Ctrl Pts',(2.65313338408978,1.82948990526959,8.17778000417152));
#12047=CARTESIAN_POINT('Ctrl Pts',(2.66087015350301,1.81822743106244,8.17693474076742));
#12048=CARTESIAN_POINT('Ctrl Pts',(2.66535444449386,1.81164749696855,8.17644381968037));
#12049=CARTESIAN_POINT('Ctrl Pts',(2.68061139660243,1.78908124735452,8.17476986499453));
#12050=CARTESIAN_POINT('Ctrl Pts',(2.69126523638913,1.77301456241518,8.17359459837548));
#12051=CARTESIAN_POINT('Ctrl Pts',(2.75108891190173,1.68101477443178,8.16695267436686));
#12052=CARTESIAN_POINT('Ctrl Pts',(2.79719305364331,1.60312662590675,8.16166675577809));
#12053=CARTESIAN_POINT('Ctrl Pts',(2.97390819186197,1.27368846713814,8.1402346970622));
#12054=CARTESIAN_POINT('Ctrl Pts',(3.07433847305442,1.00740787792131,8.12494432390821));
#12055=CARTESIAN_POINT('Ctrl Pts',(3.15317723981285,0.669093012184489,8.1048473039023));
#12056=CARTESIAN_POINT('Ctrl Pts',(3.16583972636272,0.606358172287019,8.10109998830986));
#12057=CARTESIAN_POINT('Ctrl Pts',(3.18349483106141,0.503128612881159,8.09487342480401));
#12058=CARTESIAN_POINT('Ctrl Pts',(3.18960114412124,0.462841284842914,8.09242860422071));
#12059=CARTESIAN_POINT('Ctrl Pts',(3.19700041338162,0.406881489302844,8.08900793060503));
#12060=CARTESIAN_POINT('Ctrl Pts',(3.19894514461284,0.391298016377325,8.08805271324975));
#12061=CARTESIAN_POINT('Ctrl Pts',(3.20188023352817,0.366292606015592,8.08651549693148));
#12062=CARTESIAN_POINT('Ctrl Pts',(3.20294309376386,0.356879304743489,8.08593579894911));
#12063=CARTESIAN_POINT('Ctrl Pts',(3.20499467234622,0.337961570921506,8.0847687015072));
#12064=CARTESIAN_POINT('Ctrl Pts',(3.20598265222462,0.328457156536636,8.08418128493849));
#12065=CARTESIAN_POINT('Ctrl Pts',(3.20789892967487,0.309189584762989,8.08298826345403));
#12066=CARTESIAN_POINT('Ctrl Pts',(3.20882496015555,0.299426308128521,8.08238259331582));
#12067=CARTESIAN_POINT('Ctrl Pts',(3.21085396987018,0.276942889645245,8.0809851358859));
#12068=CARTESIAN_POINT('Ctrl Pts',(3.21192594388193,0.264220179771188,8.08019237794668));
#12069=CARTESIAN_POINT('Ctrl Pts',(3.21541309354019,0.21967021619048,8.07740935626988));
#12070=CARTESIAN_POINT('Ctrl Pts',(3.21743095265524,0.187814569564738,8.07540666130566));
#12071=CARTESIAN_POINT('Ctrl Pts',(3.22152329183475,0.103336231139147,8.07006066720517));
#12072=CARTESIAN_POINT('Ctrl Pts',(3.22278156527427,0.0506859090623757,
8.06669274223213));
#12073=CARTESIAN_POINT('Ctrl Pts',(3.22274939864108,-0.00196877082894968,
8.06328801173323));
#12074=CARTESIAN_POINT('Ctrl Pts',(-1.47525540501185,-2.86526422036142,
7.65376407014636));
#12075=CARTESIAN_POINT('Ctrl Pts',(-1.38644963466766,-2.9109881685284,7.65991635409541));
#12076=CARTESIAN_POINT('Ctrl Pts',(-1.29546923767711,-2.95260373781076,
7.66606863804446));
#12077=CARTESIAN_POINT('Ctrl Pts',(-1.20273214142544,-2.98990852008589,
7.6722209219935));
#12078=CARTESIAN_POINT('Ctrl Pts',(-1.11001191723956,-3.02720651533871,
7.67837208663061));
#12079=CARTESIAN_POINT('Ctrl Pts',(-1.01553603176287,-3.06019512043509,
7.68452325126771));
#12080=CARTESIAN_POINT('Ctrl Pts',(-0.919742622604065,-3.08871997284723,
7.69067441590482));
#12081=CARTESIAN_POINT('Ctrl Pts',(-0.823941047833115,-3.11724725677197,
7.69682610487888));
#12082=CARTESIAN_POINT('Ctrl Pts',(-0.726822142574996,-3.14130990861831,
7.70297779385294));
#12083=CARTESIAN_POINT('Ctrl Pts',(-0.628838468977979,-3.16080365452102,
7.709129482827));
#12084=CARTESIAN_POINT('Ctrl Pts',(-0.530078506583397,-3.18045184224053,
7.71532990938214));
#12085=CARTESIAN_POINT('Ctrl Pts',(-0.430440450089063,-3.19545831082972,
7.72153033593728));
#12086=CARTESIAN_POINT('Ctrl Pts',(-0.330395857705662,-3.20576919626335,
7.72773076249242));
#12087=CARTESIAN_POINT('Ctrl Pts',(-0.230986158321603,-3.21601464778573,
7.73389184051988));
#12088=CARTESIAN_POINT('Ctrl Pts',(-0.131175508218247,-3.22162397899351,
7.74005291854734));
#12089=CARTESIAN_POINT('Ctrl Pts',(-0.0314279910081243,-3.2225967547742,
7.7462139965748));
#12090=CARTESIAN_POINT('Ctrl Pts',(0.0692751019773634,-3.22357884969382,
7.75243409739379));
#12091=CARTESIAN_POINT('Ctrl Pts',(0.169913393363746,-3.21983510293097,
7.75865419821277));
#12092=CARTESIAN_POINT('Ctrl Pts',(0.270014601907335,-3.21141863936436,
7.76487429903175));
#12093=CARTESIAN_POINT('Ctrl Pts',(0.370115810450923,-3.20300217579775,
7.77109439985074));
#12094=CARTESIAN_POINT('Ctrl Pts',(0.469679499641924,-3.18991311630918,
7.77731450066972));
#12095=CARTESIAN_POINT('Ctrl Pts',(0.568245329918624,-3.17225705256142,
7.7835346014887));
#12096=CARTESIAN_POINT('Ctrl Pts',(0.666067788263,-3.15473414877578,7.78970779103679));
#12097=CARTESIAN_POINT('Ctrl Pts',(0.763250526326483,-3.13265146741895,
7.79588098058488));
#12098=CARTESIAN_POINT('Ctrl Pts',(0.859335649326477,-3.10606822273701,
7.80205417013297));
#12099=CARTESIAN_POINT('Ctrl Pts',(0.95529095626567,-3.07952089341845,7.80821901937691));
#12100=CARTESIAN_POINT('Ctrl Pts',(1.0501511808306,-3.04848520131768,7.81438386862085));
#12101=CARTESIAN_POINT('Ctrl Pts',(1.14346700560903,-3.01307165025718,7.82054871786479));
#12102=CARTESIAN_POINT('Ctrl Pts',(1.23668430195901,-2.97769549094176,7.82670705789222));
#12103=CARTESIAN_POINT('Ctrl Pts',(1.32836003673228,-2.93795081575181,7.83286539791965));
#12104=CARTESIAN_POINT('Ctrl Pts',(1.41805942227855,-2.89399810597502,7.83902373794708));
#12105=CARTESIAN_POINT('Ctrl Pts',(1.50769365270407,-2.8500773222153,7.84517760472883));
#12106=CARTESIAN_POINT('Ctrl Pts',(1.59535399928417,-2.80195477138832,7.85133147151059));
#12107=CARTESIAN_POINT('Ctrl Pts',(1.68062591525096,-2.74983892173467,7.85748533829234));
#12108=CARTESIAN_POINT('Ctrl Pts',(1.76586572460008,-2.69774269476265,7.86363688801759));
#12109=CARTESIAN_POINT('Ctrl Pts',(1.84871852014072,-2.64165638274115,7.86978843774284));
#12110=CARTESIAN_POINT('Ctrl Pts',(1.92879541135377,-2.58183381022881,7.87593998746809));
#12111=CARTESIAN_POINT('Ctrl Pts',(2.00886355338595,-2.52201777391562,7.88209086507657));
#12112=CARTESIAN_POINT('Ctrl Pts',(2.08615604621886,-2.4584665486047,7.88824174268504));
#12113=CARTESIAN_POINT('Ctrl Pts',(2.16031481799547,-2.39147599813362,7.89439262029352));
#12114=CARTESIAN_POINT('Ctrl Pts',(2.23448530675665,-2.32447486324713,7.90054446973226));
#12115=CARTESIAN_POINT('Ctrl Pts',(2.30552076874257,-2.25403361492285,7.90669631917099));
#12116=CARTESIAN_POINT('Ctrl Pts',(2.37309867492827,-2.18048623970748,7.91284816860973));
#12117=CARTESIAN_POINT('Ctrl Pts',(2.44074905272957,-2.10685999112351,7.91900661538912));
#12118=CARTESIAN_POINT('Ctrl Pts',(2.50493417597123,-2.0301212842115,7.9251650621685));
#12119=CARTESIAN_POINT('Ctrl Pts',(2.56537073886303,-1.95063849410529,7.93132350894789));
#12120=CARTESIAN_POINT('Ctrl Pts',(2.62584110262679,-1.87111125098119,7.93748540001433));
#12121=CARTESIAN_POINT('Ctrl Pts',(2.6825584844241,-1.78883722581535,7.94364729108077));
#12122=CARTESIAN_POINT('Ctrl Pts',(2.73528318951348,-1.70421343606515,7.94980918214721));
#12123=CARTESIAN_POINT('Ctrl Pts',(2.78809621421564,-1.61944789226758,7.95598139505105));
#12124=CARTESIAN_POINT('Ctrl Pts',(2.83690299037388,-1.53232510057701,7.96215360795489));
#12125=CARTESIAN_POINT('Ctrl Pts',(2.88150994870523,-1.44326642655221,7.96832582085873));
#12126=CARTESIAN_POINT('Ctrl Pts',(2.91557763667492,-1.37524961412725,7.97303972718986));
#12127=CARTESIAN_POINT('Ctrl Pts',(2.94719659092646,-1.30610413706821,7.97775363352099));
#12128=CARTESIAN_POINT('Ctrl Pts',(2.97629999177014,-1.23602423984689,7.98246753985212));
#12129=CARTESIAN_POINT('Ctrl Pts',(3.0188297503367,-1.13361417700918,7.98935612648999));
#12130=CARTESIAN_POINT('Ctrl Pts',(3.05611340035765,-1.0289026103966,7.99624471312786));
#12131=CARTESIAN_POINT('Ctrl Pts',(3.08792381878256,-0.922412083558831,
8.00313329976573));
#12132=CARTESIAN_POINT('Ctrl Pts',(3.11963641267084,-0.816249040198438,
8.01000070237556));
#12133=CARTESIAN_POINT('Ctrl Pts',(3.14590924755755,-0.708318181077056,
8.01686810498539));
#12134=CARTESIAN_POINT('Ctrl Pts',(3.16656354493143,-0.599160144211315,
8.02373550759522));
#12135=CARTESIAN_POINT('Ctrl Pts',(3.18710346491378,-0.490606592276461,
8.03056488056004));
#12136=CARTESIAN_POINT('Ctrl Pts',(3.2020867924657,-0.380839652699022,8.03739425352486));
#12137=CARTESIAN_POINT('Ctrl Pts',(3.21138534471515,-0.270410299820069,
8.04422362648968));
#12138=CARTESIAN_POINT('Ctrl Pts',(3.21889649751144,-0.181208054092015,
8.04974023407176));
#12139=CARTESIAN_POINT('Ctrl Pts',(3.22269918389552,-0.0915739967349043,
8.05525684165385));
#12140=CARTESIAN_POINT('Ctrl Pts',(3.22274949386856,-0.00180617550826221,
8.06077344923593));
#12141=CARTESIAN_POINT('',(3.22274940930447,-0.00195123747957988,7.81422655072689));
#12142=CARTESIAN_POINT('Ctrl Pts',(-1.47525540501185,-2.86526422036142,
7.40717138384282));
#12143=CARTESIAN_POINT('Ctrl Pts',(-1.38671147020266,-2.91085335572981,
7.41334750551078));
#12144=CARTESIAN_POINT('Ctrl Pts',(-1.29591331447514,-2.9524058816945,7.41952362717875));
#12145=CARTESIAN_POINT('Ctrl Pts',(-1.20326442470719,-2.98969434670738,
7.42569974884672));
#12146=CARTESIAN_POINT('Ctrl Pts',(-1.11072730614301,-3.02693782708383,
7.43186841966929));
#12147=CARTESIAN_POINT('Ctrl Pts',(-1.01634429106289,-3.05992731241399,
7.43803709049186));
#12148=CARTESIAN_POINT('Ctrl Pts',(-0.920542606245815,-3.08848164517553,
7.44420576131444));
#12149=CARTESIAN_POINT('Ctrl Pts',(-0.821799889057217,-3.11791257230135,
7.45056380522177));
#12150=CARTESIAN_POINT('Ctrl Pts',(-0.721550396993546,-3.14263139571463,
7.4569218491291));
#12151=CARTESIAN_POINT('Ctrl Pts',(-0.620283454517043,-3.16249363612837,
7.46327989303642));
#12152=CARTESIAN_POINT('Ctrl Pts',(-0.522177050373216,-3.18173597659583,
7.46943950257812));
#12153=CARTESIAN_POINT('Ctrl Pts',(-0.423116222109622,-3.19642030312448,
7.47559911211981));
#12154=CARTESIAN_POINT('Ctrl Pts',(-0.323559181618689,-3.20646643807326,
7.48175872166151));
#12155=CARTESIAN_POINT('Ctrl Pts',(-0.224026376014791,-3.21651012752001,
7.48791683178698));
#12156=CARTESIAN_POINT('Ctrl Pts',(-0.123998028914641,-3.22191782599267,
7.49407494191246));
#12157=CARTESIAN_POINT('Ctrl Pts',(-0.0239386781153377,-3.22266109018465,
7.50023305203793));
#12158=CARTESIAN_POINT('Ctrl Pts',(0.0761228768800743,-3.22340437074991,
7.50639129781972));
#12159=CARTESIAN_POINT('Ctrl Pts',(0.176215003847994,-3.21948301033851,
7.5125495436015));
#12160=CARTESIAN_POINT('Ctrl Pts',(0.275872946911921,-3.21092069034134,
7.51870778938328));
#12161=CARTESIAN_POINT('Ctrl Pts',(0.375559539726755,-3.20235590884108,
7.52486780554285));
#12162=CARTESIAN_POINT('Ctrl Pts',(0.474811269307638,-3.1891475539048,7.53102782170241));
#12163=CARTESIAN_POINT('Ctrl Pts',(0.573169271697264,-3.17137108337735,
7.53718783786197));
#12164=CARTESIAN_POINT('Ctrl Pts',(0.671637472571346,-3.15357469642151,
7.54335475558956));
#12165=CARTESIAN_POINT('Ctrl Pts',(0.769209521553051,-3.13120005760236,
7.54952167331716));
#12166=CARTESIAN_POINT('Ctrl Pts',(0.865437712260869,-3.10437354851131,
7.55568859104475));
#12167=CARTESIAN_POINT('Ctrl Pts',(0.961730663784091,-3.07752898539065,
7.56185965905946));
#12168=CARTESIAN_POINT('Ctrl Pts',(1.05667754608014,-3.04622672280497,7.56803072707418));
#12169=CARTESIAN_POINT('Ctrl Pts',(1.14984864136705,-3.01064206847084,7.57420179508889));
#12170=CARTESIAN_POINT('Ctrl Pts',(1.24315849563187,-2.97500441819145,7.58038205362657));
#12171=CARTESIAN_POINT('Ctrl Pts',(1.33468689024469,-2.93507182280368,7.58656231216424));
#12172=CARTESIAN_POINT('Ctrl Pts',(1.42402700472962,-2.89106635210968,7.59274257070192));
#12173=CARTESIAN_POINT('Ctrl Pts',(1.44357232179737,-2.88143908800342,7.59409465216472));
#12174=CARTESIAN_POINT('Ctrl Pts',(1.4630130093848,-2.87161705432507,7.59544673362752));
#12175=CARTESIAN_POINT('Ctrl Pts',(1.48234499273142,-2.861602852428,7.59679881509032));
#12176=CARTESIAN_POINT('Ctrl Pts',(1.57074490588527,-2.81581062500192,7.6029815166655));
#12177=CARTESIAN_POINT('Ctrl Pts',(1.65717056177596,-2.76584082135359,7.60916421824068));
#12178=CARTESIAN_POINT('Ctrl Pts',(1.74120158228424,-2.71188764744243,7.61534691981586));
#12179=CARTESIAN_POINT('Ctrl Pts',(1.82512169312725,-2.65800568447722,7.62152146105503));
#12180=CARTESIAN_POINT('Ctrl Pts',(1.90665309024184,-2.60015103407787,7.6276960022942));
#12181=CARTESIAN_POINT('Ctrl Pts',(1.98539896798611,-2.53856425965933,7.63387054353338));
#12182=CARTESIAN_POINT('Ctrl Pts',(2.06406394588774,-2.47704075662084,7.64003874133682));
#12183=CARTESIAN_POINT('Ctrl Pts',(2.13994875533962,-2.41179301830379,7.64620693914026));
#12184=CARTESIAN_POINT('Ctrl Pts',(2.21268542963185,-2.34310493832328,7.65237513694371));
#12185=CARTESIAN_POINT('Ctrl Pts',(2.28537181367839,-2.27446434938426,7.65853907004594));
#12186=CARTESIAN_POINT('Ctrl Pts',(2.35491407642516,-2.20238844422196,7.66470300314817));
#12187=CARTESIAN_POINT('Ctrl Pts',(2.42097791650659,-2.1272008580027,7.6708669362504));
#12188=CARTESIAN_POINT('Ctrl Pts',(2.48701825869888,-2.05204001484838,7.67702867693668));
#12189=CARTESIAN_POINT('Ctrl Pts',(2.54958235152694,-1.97377001471056,7.68319041762297));
#12190=CARTESIAN_POINT('Ctrl Pts',(2.60837393614563,-1.89275010810624,7.68935215830925));
#12191=CARTESIAN_POINT('Ctrl Pts',(2.6671601816317,-1.81173755929009,7.69551333941969));
#12192=CARTESIAN_POINT('Ctrl Pts',(2.72217434603628,-1.72797595076776,7.70167452053012));
#12193=CARTESIAN_POINT('Ctrl Pts',(2.7731621343777,-1.64185545616956,7.70783570164056));
#12194=CARTESIAN_POINT('Ctrl Pts',(2.82415879720679,-1.55571997219266,7.7139979551122));
#12195=CARTESIAN_POINT('Ctrl Pts',(2.87112747127984,-1.46722515879271,7.72016020858384));
#12196=CARTESIAN_POINT('Ctrl Pts',(2.91385915369973,-1.37678698239789,7.72632246205547));
#12197=CARTESIAN_POINT('Ctrl Pts',(2.95663722150481,-1.28625063505799,7.73249140467401));
#12198=CARTESIAN_POINT('Ctrl Pts',(2.99516892824132,-1.19376710416503,7.73866034729254));
#12199=CARTESIAN_POINT('Ctrl Pts',(3.02929295278728,-1.09977350790666,7.74482928991108));
#12200=CARTESIAN_POINT('Ctrl Pts',(3.06343640094297,-1.00572640990121,7.75100174393061));
#12201=CARTESIAN_POINT('Ctrl Pts',(3.09316704163156,-0.910167947767144,
7.75717419795014));
#12202=CARTESIAN_POINT('Ctrl Pts',(3.11837370832897,-0.81354961600545,7.76334665196967));
#12203=CARTESIAN_POINT('Ctrl Pts',(3.14362252831195,-0.716769708729668,
7.76952942822737));
#12204=CARTESIAN_POINT('Ctrl Pts',(3.16433217268322,-0.618926814870015,
7.77571220448507));
#12205=CARTESIAN_POINT('Ctrl Pts',(3.18044274974578,-0.520481967112708,
7.78189498074276));
#12206=CARTESIAN_POINT('Ctrl Pts',(3.19246099655305,-0.447043599718565,
7.78650723831309));
#12207=CARTESIAN_POINT('Ctrl Pts',(3.20192096831247,-0.373270435471746,
7.79111949588342));
#12208=CARTESIAN_POINT('Ctrl Pts',(3.20881669037223,-0.299354321980865,
7.79573175345375));
#12209=CARTESIAN_POINT('Ctrl Pts',(3.21803379498261,-0.200555016479001,
7.80189668587813));
#12210=CARTESIAN_POINT('Ctrl Pts',(3.22268924659059,-0.101318614663308,
7.80806161830251));
#12211=CARTESIAN_POINT('Ctrl Pts',(3.22274940930447,-0.00195123747957988,
7.81422655072689));
#12212=CARTESIAN_POINT('Ctrl Pts',(3.22274932270398,-0.00208938053611371,
7.81661100490856));
#12213=CARTESIAN_POINT('Ctrl Pts',(3.22291239419932,0.249439023247388,7.8311833694689));
#12214=CARTESIAN_POINT('Ctrl Pts',(3.19362926120235,0.500148083184054,7.84481689517584));
#12215=CARTESIAN_POINT('Ctrl Pts',(3.11304789178756,0.839323643325621,7.86460739709412));
#12216=CARTESIAN_POINT('Ctrl Pts',(3.08637114396103,0.932653367675951,7.87019217685673));
#12217=CARTESIAN_POINT('Ctrl Pts',(3.03702325784947,1.07981222902295,7.87933101176798));
#12218=CARTESIAN_POINT('Ctrl Pts',(3.01702917710218,1.13447742086749,7.88280133181157));
#12219=CARTESIAN_POINT('Ctrl Pts',(2.98917878097904,1.20466916884041,7.88736914577782));
#12220=CARTESIAN_POINT('Ctrl Pts',(2.98266097621755,1.22071744217555,7.88842119815647));
#12221=CARTESIAN_POINT('Ctrl Pts',(2.97185811066363,1.2467133712967,7.89013824177165));
#12222=CARTESIAN_POINT('Ctrl Pts',(2.96765165744539,1.25669347718225,7.89080053785394));
#12223=CARTESIAN_POINT('Ctrl Pts',(2.95947034396081,1.27583406340428,7.89207680293235));
#12224=CARTESIAN_POINT('Ctrl Pts',(2.95550305182177,1.28499765804987,7.89269050555653));
#12225=CARTESIAN_POINT('Ctrl Pts',(2.94632807113943,1.30592262726926,7.89409812244582));
#12226=CARTESIAN_POINT('Ctrl Pts',(2.94109245362894,1.31767150027749,7.89489299590258));
#12227=CARTESIAN_POINT('Ctrl Pts',(2.92700875580443,1.34877356737663,7.89700942593846));
#12228=CARTESIAN_POINT('Ctrl Pts',(2.91803920197356,1.36807074854517,7.89833518695753));
#12229=CARTESIAN_POINT('Ctrl Pts',(2.84799321808213,1.51494500003797,7.90852440611709));
#12230=CARTESIAN_POINT('Ctrl Pts',(2.77877707849778,1.63844803163552,7.91767522228456));
#12231=CARTESIAN_POINT('Ctrl Pts',(2.58696198290358,1.93339715144885,7.94099802439458));
#12232=CARTESIAN_POINT('Ctrl Pts',(2.45524212287087,2.09813537452023,7.95541066578146));
#12233=CARTESIAN_POINT('Ctrl Pts',(2.25008038076588,2.30873267972408,7.97515359571141));
#12234=CARTESIAN_POINT('Ctrl Pts',(2.18942374043026,2.3663334451214,7.98070997231011));
#12235=CARTESIAN_POINT('Ctrl Pts',(2.1049415164223,2.44052637500369,7.98801075027205));
#12236=CARTESIAN_POINT('Ctrl Pts',(2.08303683116699,2.45924896257552,7.98986627708023));
#12237=CARTESIAN_POINT('Ctrl Pts',(2.05034708217619,2.48643966698099,7.99257708070185));
#12238=CARTESIAN_POINT('Ctrl Pts',(2.03975497069508,2.49513627876588,7.99344659340964));
#12239=CARTESIAN_POINT('Ctrl Pts',(2.02059230835463,2.51066613007455,7.99500333965673));
#12240=CARTESIAN_POINT('Ctrl Pts',(2.01204182646676,2.51752366226652,7.99569219562318));
#12241=CARTESIAN_POINT('Ctrl Pts',(1.99850021089175,2.52827105065238,7.9967738590614));
#12242=CARTESIAN_POINT('Ctrl Pts',(1.9935324166196,2.53218998182143,7.99716871555721));
#12243=CARTESIAN_POINT('Ctrl Pts',(1.98853853016755,2.53610569118877,7.99756366077424));
#12244=CARTESIAN_POINT('Ctrl Pts',(1.98852399843804,2.53611708532492,7.99756481001003));
#12245=CARTESIAN_POINT('Ctrl Pts',(1.9884948810692,2.53613991546308,7.99756711271136));
#12246=CARTESIAN_POINT('Ctrl Pts',(1.98848029540349,2.53615135148429,7.99756826617885));
#12247=CARTESIAN_POINT('Ctrl Pts',(1.98845019244889,2.53617495355482,7.99757064675373));
#12248=CARTESIAN_POINT('Ctrl Pts',(1.98843467506125,2.5361871196548,7.9975718738667));
#12249=CARTESIAN_POINT('Ctrl Pts',(1.98840338093371,2.53621165473099,7.99757434856349));
#12250=CARTESIAN_POINT('Ctrl Pts',(1.98838760423611,2.5362240236663,7.99757559614334));
#12251=CARTESIAN_POINT('Ctrl Pts',(1.98835578614724,2.53624896857747,7.99757811219431));
#12252=CARTESIAN_POINT('Ctrl Pts',(1.98833974475694,2.53626154454453,7.9975793806647));
#12253=CARTESIAN_POINT('Ctrl Pts',(1.98830739182855,2.53628690777079,7.99758193892604));
#12254=CARTESIAN_POINT('Ctrl Pts',(1.98829108029912,2.53629969501487,7.99758322871561));
#12255=CARTESIAN_POINT('Ctrl Pts',(1.98388901657916,2.53975057588469,7.99793130414242));
#12256=CARTESIAN_POINT('Ctrl Pts',(1.97949436027855,2.54317728359509,7.99827725613142));
#12257=CARTESIAN_POINT('Ctrl Pts',(1.96945807277163,2.55096124526612,7.99906387158608));
#12258=CARTESIAN_POINT('Ctrl Pts',(1.9638107963393,2.55531124009185,7.99950401834394));
#12259=CARTESIAN_POINT('Ctrl Pts',(1.94650630314225,2.56854932982754,8.00084535181694));
#12260=CARTESIAN_POINT('Ctrl Pts',(1.93480264630484,2.57737680339038,8.00174236965873));
#12261=CARTESIAN_POINT('Ctrl Pts',(1.77243199238497,2.69811542548282,8.01405368247367));
#12262=CARTESIAN_POINT('Ctrl Pts',(1.61230561832042,2.79675418420261,8.02462904823332));
#12263=CARTESIAN_POINT('Ctrl Pts',(1.31562301647539,2.94551054961165,8.04320218946657));
#12264=CARTESIAN_POINT('Ctrl Pts',(1.18257688858008,3.00140080208691,8.05120669365991));
#12265=CARTESIAN_POINT('Ctrl Pts',(0.957753331581384,3.07856762020385,8.06472954336099));
#12266=CARTESIAN_POINT('Ctrl Pts',(0.867991302652524,3.10506990587199,8.07012583530546));
#12267=CARTESIAN_POINT('Ctrl Pts',(0.722040652644978,3.14133829389882,8.07899083353608));
#12268=CARTESIAN_POINT('Ctrl Pts',(0.666522630973167,3.15358462152701,8.08238317238944));
#12269=CARTESIAN_POINT('Ctrl Pts',(0.593743553348956,3.16763078918094,8.08686829675858));
#12270=CARTESIAN_POINT('Ctrl Pts',(0.576749066642107,3.17076910540319,8.08791827103549));
#12271=CARTESIAN_POINT('Ctrl Pts',(0.54900534341609,3.1756620255081,8.08963702309177));
#12272=CARTESIAN_POINT('Ctrl Pts',(0.538270859982677,3.17749911786822,8.09030316726141));
#12273=CARTESIAN_POINT('Ctrl Pts',(0.517563639668784,3.18093499629054,8.09159044815188));
#12274=CARTESIAN_POINT('Ctrl Pts',(0.507592280179287,3.18254138152798,8.09221133503163));
#12275=CARTESIAN_POINT('Ctrl Pts',(0.484676630399889,3.18612265613375,8.09364061253893));
#12276=CARTESIAN_POINT('Ctrl Pts',(0.471727591307244,3.18806557138825,8.09445000717394));
#12277=CARTESIAN_POINT('Ctrl Pts',(0.437139984646929,3.19303986949242,8.09661676367176));
#12278=CARTESIAN_POINT('Ctrl Pts',(0.415482116672585,3.19593015368049,8.09797855773902));
#12279=CARTESIAN_POINT('Ctrl Pts',(0.234857759553856,3.21816779616052,8.10937943104561));
#12280=CARTESIAN_POINT('Ctrl Pts',(0.074705678239877,3.22585918932508,8.11978646975565));
#12281=CARTESIAN_POINT('Ctrl Pts',(-0.34142491355845,3.21483667004354,8.14751307528701));
#12282=CARTESIAN_POINT('Ctrl Pts',(-0.595778106288571,3.17754439942478,
8.16518974121458));
#12283=CARTESIAN_POINT('Ctrl Pts',(-0.89716771663642,3.09586081282522,8.18560963661507));
#12284=CARTESIAN_POINT('Ctrl Pts',(-0.950920069685817,3.07977531747029,
8.18922600764724));
#12285=CARTESIAN_POINT('Ctrl Pts',(-1.01533753221225,3.05865067224684,8.193506664754));
#12286=CARTESIAN_POINT('Ctrl Pts',(-1.02642663418538,3.05494723581705,8.19424162145674));
#12287=CARTESIAN_POINT('Ctrl Pts',(-1.04367455731185,3.04908241536222,8.19538147901506));
#12288=CARTESIAN_POINT('Ctrl Pts',(-1.04984724772803,3.04696257205005,8.19578875234949));
#12289=CARTESIAN_POINT('Ctrl Pts',(-1.06130146130086,3.04298999284143,8.19654321773187));
#12290=CARTESIAN_POINT('Ctrl Pts',(-1.06658456098769,3.04114226294447,8.19689069032292));
#12291=CARTESIAN_POINT('Ctrl Pts',(-1.07855473741985,3.03692074154765,8.19767682421497));
#12292=CARTESIAN_POINT('Ctrl Pts',(-1.08523878582975,3.03453862919129,8.19811498571747));
#12293=CARTESIAN_POINT('Ctrl Pts',(-1.10508609886458,3.0273913278311,8.1994137870648));
#12294=CARTESIAN_POINT('Ctrl Pts',(-1.11822644224297,3.02256235304654,8.20027072990811));
#12295=CARTESIAN_POINT('Ctrl Pts',(-1.21961463491292,2.98455128077434,8.20686285523089));
#12296=CARTESIAN_POINT('Ctrl Pts',(-1.30640852586918,2.94759335573578,8.21238969921858));
#12297=CARTESIAN_POINT('Ctrl Pts',(-1.60792321106036,2.80326428826997,8.23158968182284));
#12298=CARTESIAN_POINT('Ctrl Pts',(-1.81213767813902,2.67579461295379,8.24464748064823));
#12299=CARTESIAN_POINT('Ctrl Pts',(-2.07244815745649,2.46972468172623,8.26355017385069));
#12300=CARTESIAN_POINT('Ctrl Pts',(-2.14209781674233,2.40956352509111,8.26886059430073));
#12301=CARTESIAN_POINT('Ctrl Pts',(-2.24994121681319,2.30803644520514,8.27759481609647));
#12302=CARTESIAN_POINT('Ctrl Pts',(-2.28979308661072,2.26850496038625,8.28094505097589));
#12303=CARTESIAN_POINT('Ctrl Pts',(-2.34046849690914,2.21554055983848,8.28538093340298));
#12304=CARTESIAN_POINT('Ctrl Pts',(-2.35224659711994,2.20303170333044,8.28642486364947));
#12305=CARTESIAN_POINT('Ctrl Pts',(-2.37130114201489,2.18246792996896,8.28813532541151));
#12306=CARTESIAN_POINT('Ctrl Pts',(-2.37863800623781,2.17446926908372,8.28879925831892));
#12307=CARTESIAN_POINT('Ctrl Pts',(-2.39271324055299,2.1589679488566,8.29008338226154));
#12308=CARTESIAN_POINT('Ctrl Pts',(-2.39945708545186,2.15147041511032,8.29070333008597));
#12309=CARTESIAN_POINT('Ctrl Pts',(-2.41487995631976,2.13416118244532,8.2921320279114));
#12310=CARTESIAN_POINT('Ctrl Pts',(-2.42353452674198,2.12432802213781,8.29294179066548));
#12311=CARTESIAN_POINT('Ctrl Pts',(-2.44650636077899,2.09790476416592,8.29511296263071));
#12312=CARTESIAN_POINT('Ctrl Pts',(-2.46071456813859,2.08122116765404,8.29647885314647));
#12313=CARTESIAN_POINT('Ctrl Pts',(-2.57967483338234,1.93861417360511,8.30811418962841));
#12314=CARTESIAN_POINT('Ctrl Pts',(-2.6748402046713,1.80503805129905,8.31877045707719));
#12315=CARTESIAN_POINT('Ctrl Pts',(-2.88965063120983,1.44899217831922,8.34650564291163));
#12316=CARTESIAN_POINT('Ctrl Pts',(-2.99409050299239,1.21863699019569,8.36390197583305));
#12317=CARTESIAN_POINT('Ctrl Pts',(-3.08840438705934,0.922662848981157,
8.38424998917271));
#12318=CARTESIAN_POINT('Ctrl Pts',(-3.10466462765573,0.866375763504488,
8.38803103874007));
#12319=CARTESIAN_POINT('Ctrl Pts',(-3.12234782082464,0.798248676855255,
8.39247665849845));
#12320=CARTESIAN_POINT('Ctrl Pts',(-3.12525034542224,0.786808205928582,
8.39321881308502));
#12321=CARTESIAN_POINT('Ctrl Pts',(-3.129661747258,0.769010786393292,8.39436625942861));
#12322=CARTESIAN_POINT('Ctrl Pts',(-3.13121422022984,0.762664900640009,
8.39477399910329));
#12323=CARTESIAN_POINT('Ctrl Pts',(-3.13405570503181,0.750895118596302,
8.39552759582176));
#12324=CARTESIAN_POINT('Ctrl Pts',(-3.13534992942518,0.745472643521718,
8.39587374292877));
#12325=CARTESIAN_POINT('Ctrl Pts',(-3.1382438918827,0.733206809843047,8.3966544013219));
#12326=CARTESIAN_POINT('Ctrl Pts',(-3.13983531561365,0.72636157936522,8.39708842969506));
#12327=CARTESIAN_POINT('Ctrl Pts',(-3.14446866258261,0.706132265454387,
8.39836640889907));
#12328=CARTESIAN_POINT('Ctrl Pts',(-3.14744753597062,0.69273369354334,8.39920681870286));
#12329=CARTESIAN_POINT('Ctrl Pts',(-3.16859455172315,0.594664040890788,
8.40531676340006));
#12330=CARTESIAN_POINT('Ctrl Pts',(-3.18343069731096,0.509302113536559,
8.41041033933932));
#12331=CARTESIAN_POINT('Ctrl Pts',(-3.22766651600784,0.175546192818822,
8.42981776288062));
#12332=CARTESIAN_POINT('Ctrl Pts',(-3.23156117410327,-0.0753367921670371,
8.44338678472963));
#12333=CARTESIAN_POINT('Ctrl Pts',(-3.19725577395872,-0.414666429627105,
8.46281082990313));
#12334=CARTESIAN_POINT('Ctrl Pts',(-3.18427846140868,-0.504739071184974,
8.46806346755697));
#12335=CARTESIAN_POINT('Ctrl Pts',(-3.15724770205412,-0.648847428059623,
8.47671086724397));
#12336=CARTESIAN_POINT('Ctrl Pts',(-3.14557044659996,-0.703279488168077,
8.48003377933204));
#12337=CARTESIAN_POINT('Ctrl Pts',(-3.12846802410272,-0.774014392802717,
8.48443758235242));
#12338=CARTESIAN_POINT('Ctrl Pts',(-3.12431363039132,-0.790616708308909,
8.48547741725762));
#12339=CARTESIAN_POINT('Ctrl Pts',(-3.11731510549376,-0.817668240630555,
8.48718218056504));
#12340=CARTESIAN_POINT('Ctrl Pts',(-3.11455015952333,-0.828137740933525,
8.48784453210263));
#12341=CARTESIAN_POINT('Ctrl Pts',(-3.10911164481082,-0.848318213444777,
8.48912630314015));
#12342=CARTESIAN_POINT('Ctrl Pts',(-3.10644520768443,-0.858030989612591,
8.4897454836416));
#12343=CARTESIAN_POINT('Ctrl Pts',(-3.10020612835715,-0.880347165803772,
8.49117341926795));
#12344=CARTESIAN_POINT('Ctrl Pts',(-3.09660210155425,-0.892941536237934,
8.4919831923793));
#12345=CARTESIAN_POINT('Ctrl Pts',(-3.08675391408626,-0.926579546320306,
8.4941566184354));
#12346=CARTESIAN_POINT('Ctrl Pts',(-3.08037146114403,-0.947581661184512,
8.49552478190982));
#12347=CARTESIAN_POINT('Ctrl Pts',(-3.02362112304629,-1.12768986855556,
8.50735610465119));
#12348=CARTESIAN_POINT('Ctrl Pts',(-2.96118734985755,-1.28270149302478,
8.51822202388104));
#12349=CARTESIAN_POINT('Ctrl Pts',(-2.77168984861823,-1.6647023517483,8.54668743406963));
#12350=CARTESIAN_POINT('Ctrl Pts',(-2.62866977294471,-1.88244272121886,
8.56462354286451));
#12351=CARTESIAN_POINT('Ctrl Pts',(-2.4295901264145,-2.1179209401305,8.58470851864057));
#12352=CARTESIAN_POINT('Ctrl Pts',(-2.39725137917777,-2.15445671347857,
8.58784403981477));
#12353=CARTESIAN_POINT('Ctrl Pts',(-2.35650402086181,-2.19843832546854,
8.59162766756298));
#12354=CARTESIAN_POINT('Ctrl Pts',(-2.34887183217735,-2.20659089907569,
8.59232940588338));
#12355=CARTESIAN_POINT('Ctrl Pts',(-2.33680595919136,-2.21934591824998,
8.59342768532506));
#12356=CARTESIAN_POINT('Ctrl Pts',(-2.33240078661435,-2.22397503764171,
8.59382635875229));
#12357=CARTESIAN_POINT('Ctrl Pts',(-2.32411356840756,-2.23263184940374,
8.59457200576773));
#12358=CARTESIAN_POINT('Ctrl Pts',(-2.32023485212496,-2.23666248801878,
8.59491921444437));
#12359=CARTESIAN_POINT('Ctrl Pts',(-2.31131681927921,-2.24588166135363,
8.59571348561187));
#12360=CARTESIAN_POINT('Ctrl Pts',(-2.30627052284075,-2.25106333846185,
8.59615999462763));
#12361=CARTESIAN_POINT('Ctrl Pts',(-2.29298303880059,-2.26461571331645,
8.59732818088585));
#12362=CARTESIAN_POINT('Ctrl Pts',(-2.28471336820862,-2.27295850822992,
8.59804768331967));
#12363=CARTESIAN_POINT('Ctrl Pts',(-2.22814774798873,-2.32940367215067,
8.60291977523013));
#12364=CARTESIAN_POINT('Ctrl Pts',(-2.17837798877688,-2.3760123525556,8.60696345033467));
#12365=CARTESIAN_POINT('Ctrl Pts',(-2.1056051498441,-2.43995247055496,8.61260527242614));
#12366=CARTESIAN_POINT('Ctrl Pts',(-2.08379434720952,-2.4586057639987,8.61426335794122));
#12367=CARTESIAN_POINT('Ctrl Pts',(-1.88099374527501,-2.62740966316,8.62941227749103));
#12368=CARTESIAN_POINT('Ctrl Pts',(-1.68433187323717,-2.75761579212618,
8.6422176227668));
#12369=CARTESIAN_POINT('Ctrl Pts',(-1.47525540497551,-2.86526422038013,
8.65558740743848));
#12370=CARTESIAN_POINT('Origin',(0.,0.,4.68922655072688));
#12371=CARTESIAN_POINT('',(-1.47525540501219,-2.86526422036124,10.1510771966379));
#12372=CARTESIAN_POINT('',(-1.47525538675478,-2.86526422976154,9.90456889022841));
#12373=CARTESIAN_POINT('',(-1.47525540501186,-2.86526422036142,4.68922655072688));
#12374=CARTESIAN_POINT('Ctrl Pts',(-1.47525540501219,-2.86526422036124,
10.1510771966379));
#12375=CARTESIAN_POINT('Ctrl Pts',(-1.49798330242841,-2.85356217443139,
10.1495893801617));
#12376=CARTESIAN_POINT('Ctrl Pts',(-1.52057167187558,-2.8415898554236,10.1481119797034));
#12377=CARTESIAN_POINT('Ctrl Pts',(-1.75495113035089,-2.7137685504471,10.1327715715633));
#12378=CARTESIAN_POINT('Ctrl Pts',(-1.95323586278964,-2.5747379397887,10.119643525819));
#12379=CARTESIAN_POINT('Ctrl Pts',(-2.20310559319854,-2.35391451488999,
10.1006602024223));
#12380=CARTESIAN_POINT('Ctrl Pts',(-2.26942121423015,-2.29004655308268,
10.0953483063834));
#12381=CARTESIAN_POINT('Ctrl Pts',(-2.37164549888876,-2.18278892774195,
10.0866115088114));
#12382=CARTESIAN_POINT('Ctrl Pts',(-2.40931060051194,-2.14114262205184,
10.0832603040736));
#12383=CARTESIAN_POINT('Ctrl Pts',(-2.45705509425807,-2.08549587202644,
10.0788234103592));
#12384=CARTESIAN_POINT('Ctrl Pts',(-2.46813845933246,-2.07236707565026,
10.0777794983055));
#12385=CARTESIAN_POINT('Ctrl Pts',(-2.4860504739894,-2.05080188878633,10.0760691452295));
#12386=CARTESIAN_POINT('Ctrl Pts',(-2.49294251506406,-2.04241840921544,
10.0754053048263));
#12387=CARTESIAN_POINT('Ctrl Pts',(-2.50615532190427,-2.02617983340296,
10.074121416626));
#12388=CARTESIAN_POINT('Ctrl Pts',(-2.51248183782853,-2.01832956320141,
10.073501612386));
#12389=CARTESIAN_POINT('Ctrl Pts',(-2.52694066273657,-2.00021497316811,
10.0720733272728));
#12390=CARTESIAN_POINT('Ctrl Pts',(-2.5350474126451,-1.98993056647264,10.0712638341013));
#12391=CARTESIAN_POINT('Ctrl Pts',(-2.55654599720707,-1.96231239164215,
10.0690935583276));
#12392=CARTESIAN_POINT('Ctrl Pts',(-2.56982398582325,-1.94489125707648,
10.067728297218));
#12393=CARTESIAN_POINT('Ctrl Pts',(-2.68079255262662,-1.79617655180575,
10.0561031313478));
#12394=CARTESIAN_POINT('Ctrl Pts',(-2.7685143128291,-1.65777344139973,10.0454570177789));
#12395=CARTESIAN_POINT('Ctrl Pts',(-2.96450120822199,-1.28928133952013,
10.0176214483249));
#12396=CARTESIAN_POINT('Ctrl Pts',(-3.0567784004247,-1.05195754527471,10.0001055939133));
#12397=CARTESIAN_POINT('Ctrl Pts',(-3.13445565251752,-0.75134779497655,
9.97978918864016));
#12398=CARTESIAN_POINT('Ctrl Pts',(-3.14719656026249,-0.696053513058442,
9.97613019505615));
#12399=CARTESIAN_POINT('Ctrl Pts',(-3.16079652554137,-0.62898309348485,
9.97180841804277));
#12400=CARTESIAN_POINT('Ctrl Pts',(-3.16305885504856,-0.617505544239278,
9.97107293311871));
#12401=CARTESIAN_POINT('Ctrl Pts',(-3.16648324617846,-0.599619731555221,
9.96993343130642));
#12402=CARTESIAN_POINT('Ctrl Pts',(-3.16768843725006,-0.593219973612614,
9.96952702166769));
#12403=CARTESIAN_POINT('Ctrl Pts',(-3.16989072655983,-0.581327367698841,
9.9687742969665));
#12404=CARTESIAN_POINT('Ctrl Pts',(-3.17089294200678,-0.575835634378956,
9.96842770178606));
#12405=CARTESIAN_POINT('Ctrl Pts',(-3.17313199315836,-0.563383432580207,
9.96764404954695));
#12406=CARTESIAN_POINT('Ctrl Pts',(-3.17436019633908,-0.556421498738663,
9.96720748816599));
#12407=CARTESIAN_POINT('Ctrl Pts',(-3.17793470792605,-0.535762690840379,
9.96591654893985));
#12408=CARTESIAN_POINT('Ctrl Pts',(-3.18021538176781,-0.522054413292213,
9.9650658119158));
#12409=CARTESIAN_POINT('Ctrl Pts',(-3.19676145970589,-0.418467762870959,
9.95867858624681));
#12410=CARTESIAN_POINT('Ctrl Pts',(-3.20730426088762,-0.328027099196606,
9.95333638335265));
#12411=CARTESIAN_POINT('Ctrl Pts',(-3.23197408711659,0.00616865497466972,
9.93406079204967));
#12412=CARTESIAN_POINT('Ctrl Pts',(-3.22223238796559,0.25085153834473,9.92079543740196));
#12413=CARTESIAN_POINT('Ctrl Pts',(-3.17094490334434,0.582792774803053,
9.90167217074299));
#12414=CARTESIAN_POINT('Ctrl Pts',(-3.15306591000912,0.672839092153315,
9.89637495399306));
#12415=CARTESIAN_POINT('Ctrl Pts',(-3.11812266495177,0.816436108454772,
9.88766010022414));
#12416=CARTESIAN_POINT('Ctrl Pts',(-3.10345808221088,0.870519517592819,
9.88431567664817));
#12417=CARTESIAN_POINT('Ctrl Pts',(-3.08246840334816,0.940638544687956,
9.8798865154964));
#12418=CARTESIAN_POINT('Ctrl Pts',(-3.07741361852219,0.957046358428913,
9.87884337039329));
#12419=CARTESIAN_POINT('Ctrl Pts',(-3.06895087267763,0.983755978737971,
9.87713395989083));
#12420=CARTESIAN_POINT('Ctrl Pts',(-3.06562151871285,0.99408248353102,9.87647028961194));
#12421=CARTESIAN_POINT('Ctrl Pts',(-3.05909760074557,1.01397293037028,9.87518650978715));
#12422=CARTESIAN_POINT('Ctrl Pts',(-3.05591016870599,1.02353909135034,9.87456664261014));
#12423=CARTESIAN_POINT('Ctrl Pts',(-3.04847799372856,1.04550042615752,9.87313789604433));
#12424=CARTESIAN_POINT('Ctrl Pts',(-3.04420247311019,1.05788492469834,9.87232800219654));
#12425=CARTESIAN_POINT('Ctrl Pts',(-3.03257012165674,1.09092473599328,9.8701559479281));
#12426=CARTESIAN_POINT('Ctrl Pts',(-3.02507791253301,1.11153133428337,9.86878929741879));
#12427=CARTESIAN_POINT('Ctrl Pts',(-2.95950138301336,1.28631813786793,9.85709312066563));
#12428=CARTESIAN_POINT('Ctrl Pts',(-2.88989202018284,1.43588717610679,9.84637190550986));
#12429=CARTESIAN_POINT('Ctrl Pts',(-2.68360201039837,1.80278617387882,9.81829147750748));
#12430=CARTESIAN_POINT('Ctrl Pts',(-2.53186237251953,2.01032991578635,9.8006002660016));
#12431=CARTESIAN_POINT('Ctrl Pts',(-2.32066532674737,2.23684888889761,9.7803718934559));
#12432=CARTESIAN_POINT('Ctrl Pts',(-2.28320564784507,2.27507214719117,9.77692557209138));
#12433=CARTESIAN_POINT('Ctrl Pts',(-2.23655897998637,2.32035637326267,9.77282108197791));
#12434=CARTESIAN_POINT('Ctrl Pts',(-2.22826602203411,2.32832135118031,9.77209831424605));
#12435=CARTESIAN_POINT('Ctrl Pts',(-2.21524132570283,2.34069760383624,9.7709741995424));
#12436=CARTESIAN_POINT('Ctrl Pts',(-2.21053873152024,2.3451392116252,9.77057056103418));
#12437=CARTESIAN_POINT('Ctrl Pts',(-2.20174917953522,2.35339102839649,9.76982031748659));
#12438=CARTESIAN_POINT('Ctrl Pts',(-2.19766572851964,2.35720472773749,9.76947344889975));
#12439=CARTESIAN_POINT('Ctrl Pts',(-2.18834841325355,2.36586128694528,9.768685778058));
#12440=CARTESIAN_POINT('Ctrl Pts',(-2.18310839275273,2.37069739837347,9.76824549273941));
#12441=CARTESIAN_POINT('Ctrl Pts',(-2.16703974483438,2.38542899350795,9.76690340960159));
#12442=CARTESIAN_POINT('Ctrl Pts',(-2.15615939265464,2.39526813345481,9.7660057886217));
#12443=CARTESIAN_POINT('Ctrl Pts',(-2.0062073826821,2.52902050638279,9.75378009747099));
#12444=CARTESIAN_POINT('Ctrl Pts',(-1.85669279309748,2.64074338310637,9.7432785203068));
#12445=CARTESIAN_POINT('Ctrl Pts',(-1.57744951807622,2.81389496316148,9.72488799190989));
#12446=CARTESIAN_POINT('Ctrl Pts',(-1.45172804239822,2.88077007724106,9.71698961155022));
#12447=CARTESIAN_POINT('Ctrl Pts',(-1.23501970008563,2.97824460780462,9.70348309559244));
#12448=CARTESIAN_POINT('Ctrl Pts',(-1.14634737152156,3.01348638555492,9.69798655318822));
#12449=CARTESIAN_POINT('Ctrl Pts',(-1.00183698375023,3.06361828910557,9.68897431149231));
#12450=CARTESIAN_POINT('Ctrl Pts',(-0.946932956252721,3.08103095048887,
9.68553854747924));
#12451=CARTESIAN_POINT('Ctrl Pts',(-0.874932642321345,3.10175934835942,
9.68100534546626));
#12452=CARTESIAN_POINT('Ctrl Pts',(-0.85823276882279,3.10642152322956,9.67995202291908));
#12453=CARTESIAN_POINT('Ctrl Pts',(-0.830986645732835,3.11379146578005,
9.67823012256292));
#12454=CARTESIAN_POINT('Ctrl Pts',(-0.820462719058099,3.11658098238875,
9.67756421344988));
#12455=CARTESIAN_POINT('Ctrl Pts',(-0.800177928237605,3.12184789111245,
9.67627902135131));
#12456=CARTESIAN_POINT('Ctrl Pts',(-0.790419176992457,3.12433296769904,
9.67565999646816));
#12457=CARTESIAN_POINT('Ctrl Pts',(-0.768019186020709,3.12992548604776,
9.67423734605707));
#12458=CARTESIAN_POINT('Ctrl Pts',(-0.755370508290407,3.13300213940569,
9.67343273435095));
#12459=CARTESIAN_POINT('Ctrl Pts',(-0.721648157117469,3.14098865030842,
9.67128401858587));
#12460=CARTESIAN_POINT('Ctrl Pts',(-0.700543369886417,3.14576297804875,
9.66993557479394));
#12461=CARTESIAN_POINT('Ctrl Pts',(-0.531255537784271,3.18227124631683,
9.65908807285468));
#12462=CARTESIAN_POINT('Ctrl Pts',(-0.381071663922611,3.203725234389,9.64925995083529));
#12463=CARTESIAN_POINT('Ctrl Pts',(-0.00567248030310788,3.2305796653726,
9.62424507274492));
#12464=CARTESIAN_POINT('Ctrl Pts',(0.21965468893966,3.22310717750737,9.60880529587015));
#12465=CARTESIAN_POINT('Ctrl Pts',(0.528483400541867,3.1803116765297,9.58804768226647));
#12466=CARTESIAN_POINT('Ctrl Pts',(0.614095951465856,3.16489589395617,9.58234507767179));
#12467=CARTESIAN_POINT('Ctrl Pts',(0.717425223241102,3.14193815157551,9.57560578178687));
#12468=CARTESIAN_POINT('Ctrl Pts',(0.735827251549994,3.13767949212627,9.57441121379952));
#12469=CARTESIAN_POINT('Ctrl Pts',(0.761874204345368,3.13140985922785,9.57272942361945));
#12470=CARTESIAN_POINT('Ctrl Pts',(0.769550392055552,3.12953226648004,9.57223490938894));
#12471=CARTESIAN_POINT('Ctrl Pts',(0.782745762778267,3.12625319777419,9.57138685912824));
#12472=CARTESIAN_POINT('Ctrl Pts',(0.788268254516875,3.12486530056206,9.57103254646471));
#12473=CARTESIAN_POINT('Ctrl Pts',(0.798956579270361,3.12214900284774,9.57034802112019));
#12474=CARTESIAN_POINT('Ctrl Pts',(0.804122795027835,3.12082241453158,9.57001770216024));
#12475=CARTESIAN_POINT('Ctrl Pts',(0.818033471925459,3.11721357536209,9.56912969396428));
#12476=CARTESIAN_POINT('Ctrl Pts',(0.826771744301351,3.11490733779355,9.56857338400094));
#12477=CARTESIAN_POINT('Ctrl Pts',(0.859071640603072,3.10623713187091,9.56652225761763));
#12478=CARTESIAN_POINT('Ctrl Pts',(0.882571143337986,3.09964215073174,9.56504024065413));
#12479=CARTESIAN_POINT('Ctrl Pts',(1.07885081183562,3.04214429508616,9.55273041844396));
#12480=CARTESIAN_POINT('Ctrl Pts',(1.24718223920008,2.97709836740406,9.54261115321278));
#12481=CARTESIAN_POINT('Ctrl Pts',(1.5341898329561,2.8375501387894,9.52476288014499));
#12482=CARTESIAN_POINT('Ctrl Pts',(1.65510324437602,2.76876523350859,9.51703614433546));
#12483=CARTESIAN_POINT('Ctrl Pts',(1.84816236532744,2.64176095669568,9.50388135650029));
#12484=CARTESIAN_POINT('Ctrl Pts',(1.92291734367836,2.58785471581919,9.49856426891199));
#12485=CARTESIAN_POINT('Ctrl Pts',(2.03938008311484,2.49603753048567,9.48981971212175));
#12486=CARTESIAN_POINT('Ctrl Pts',(2.08258380002192,2.4601054070721,9.48646611008544));
#12487=CARTESIAN_POINT('Ctrl Pts',(2.13774599011124,2.41173278118607,9.482026478794));
#12488=CARTESIAN_POINT('Ctrl Pts',(2.15057655728285,2.40029860216433,9.48098229133988));
#12489=CARTESIAN_POINT('Ctrl Pts',(2.17135997399603,2.3814766916414,9.47927159667604));
#12490=CARTESIAN_POINT('Ctrl Pts',(2.17936814535857,2.37415034316318,9.4786076920225));
#12491=CARTESIAN_POINT('Ctrl Pts',(2.19474329466983,2.35994090603032,9.47732375648716));
#12492=CARTESIAN_POINT('Ctrl Pts',(2.20211529227447,2.35306341718573,9.47670396957851));
#12493=CARTESIAN_POINT('Ctrl Pts',(2.21898668487585,2.33717502306297,9.47527583458854));
#12494=CARTESIAN_POINT('Ctrl Pts',(2.22846363137538,2.3281406382756,9.47446647495386));
#12495=CARTESIAN_POINT('Ctrl Pts',(2.25364176254992,2.30384370911539,9.47229680213002));
#12496=CARTESIAN_POINT('Ctrl Pts',(2.26924267586403,2.28847868020525,9.47093201442676));
#12497=CARTESIAN_POINT('Ctrl Pts',(2.39983737529585,2.157210061642,9.45933120051799));
#12498=CARTESIAN_POINT('Ctrl Pts',(2.50600903112001,2.03289913147211,9.44871083796801));
#12499=CARTESIAN_POINT('Ctrl Pts',(2.75154839361424,1.69679550900973,9.4209534828316));
#12500=CARTESIAN_POINT('Ctrl Pts',(2.87621582036658,1.47563918253337,9.40349158095591));
#12501=CARTESIAN_POINT('Ctrl Pts',(2.99599847901292,1.18888487028301,9.38314505362866));
#12502=CARTESIAN_POINT('Ctrl Pts',(3.01682746053736,1.13499214879745,9.3794177231507));
#12503=CARTESIAN_POINT('Ctrl Pts',(3.04014064956671,1.06948617394439,9.37502640799508));
#12504=CARTESIAN_POINT('Ctrl Pts',(3.04402288902337,1.05838580232535,9.37428702442598));
#12505=CARTESIAN_POINT('Ctrl Pts',(3.04996488561941,1.04109285919292,9.37314280810061));
#12506=CARTESIAN_POINT('Ctrl Pts',(3.05206669242826,1.0349149973481,9.37273555120382));
#12507=CARTESIAN_POINT('Ctrl Pts',(3.05593128977814,1.02344157805368,9.37198205876087));
#12508=CARTESIAN_POINT('Ctrl Pts',(3.05769907260211,1.01814787417535,9.37163553803965));
#12509=CARTESIAN_POINT('Ctrl Pts',(3.06166920903117,1.00615552323239,9.37085306867315));
#12510=CARTESIAN_POINT('Ctrl Pts',(3.06386332985656,0.999454241400612,9.37041760942009));
#12511=CARTESIAN_POINT('Ctrl Pts',(3.07029010964349,0.979605518807584,9.36913292678391));
#12512=CARTESIAN_POINT('Ctrl Pts',(3.07446032692231,0.966437811699707,9.36828729213164));
#12513=CARTESIAN_POINT('Ctrl Pts',(3.10475795287041,0.868590160540404,9.36204972150661));
#12514=CARTESIAN_POINT('Ctrl Pts',(3.12746986524456,0.782883215436703,9.35684192756291));
#12515=CARTESIAN_POINT('Ctrl Pts',(3.15375064262285,0.66412581295219,9.34983739866215));
#12516=CARTESIAN_POINT('Ctrl Pts',(3.16038482555225,0.631802233210747,9.34795208838726));
#12517=CARTESIAN_POINT('Ctrl Pts',(3.20376790413385,0.402610327376689,9.33469908676473));
#12518=CARTESIAN_POINT('Ctrl Pts',(3.22259253227262,0.202793807467092,9.32371333098121));
#12519=CARTESIAN_POINT('Ctrl Pts',(3.22286530194858,-0.146309910456225,
9.30391398381168));
#12520=CARTESIAN_POINT('Ctrl Pts',(3.21267240414683,-0.294949237190834,
9.29529762126277));
#12521=CARTESIAN_POINT('Ctrl Pts',(3.18928614388277,-0.463721191285525,
9.28504670735152));
#12522=CARTESIAN_POINT('Ctrl Pts',(3.18610889489276,-0.48507064016707,9.28374156663271));
#12523=CARTESIAN_POINT('Ctrl Pts',(3.18067454520792,-0.519226390681428,
9.28163937885324));
#12524=CARTESIAN_POINT('Ctrl Pts',(3.17855394234404,-0.532053977661528,
9.28084666557937));
#12525=CARTESIAN_POINT('Ctrl Pts',(3.17465366011762,-0.554791005188704,
9.2794357270943));
#12526=CARTESIAN_POINT('Ctrl Pts',(3.17290504781711,-0.56470565343308,9.27881849944492));
#12527=CARTESIAN_POINT('Ctrl Pts',(3.16916758408359,-0.585331591729099,
9.277530260138));
#12528=CARTESIAN_POINT('Ctrl Pts',(3.16717082125311,-0.596041301100955,
9.27685900277794));
#12529=CARTESIAN_POINT('Ctrl Pts',(3.1618495464183,-0.623800236435388,9.27511292105727));
#12530=CARTESIAN_POINT('Ctrl Pts',(3.15844146081401,-0.64083290234613,9.27403543436173));
#12531=CARTESIAN_POINT('Ctrl Pts',(3.14307892566315,-0.714509519888538,
9.26934759894313));
#12532=CARTESIAN_POINT('Ctrl Pts',(3.12973772570854,-0.770850215272871,
9.26569305806917));
#12533=CARTESIAN_POINT('Ctrl Pts',(3.0902376559278,-0.919663130509084,9.25584722265343));
#12534=CARTESIAN_POINT('Ctrl Pts',(3.0614497149314,-1.01137126634294,9.24957674504851));
#12535=CARTESIAN_POINT('Ctrl Pts',(2.98022535374917,-1.23466994676335,9.23382728287994));
#12536=CARTESIAN_POINT('Ctrl Pts',(2.92313126069588,-1.3643504593328,9.22424625302479));
#12537=CARTESIAN_POINT('Ctrl Pts',(2.77176098731157,-1.65469599580339,9.20208353823569));
#12538=CARTESIAN_POINT('Ctrl Pts',(2.67170607793641,-1.81181697256035,9.18953678143932));
#12539=CARTESIAN_POINT('Ctrl Pts',(2.54972666132089,-1.97109788310698,9.17682059420688));
#12540=CARTESIAN_POINT('Ctrl Pts',(2.54072464006728,-1.98268788134281,9.17589544650774));
#12541=CARTESIAN_POINT('Ctrl Pts',(2.52723056380333,-1.99981851675774,9.17452874573523));
#12542=CARTESIAN_POINT('Ctrl Pts',(2.5227989268441,-2.00540619317524,9.17408306943009));
#12543=CARTESIAN_POINT('Ctrl Pts',(2.51486221130881,-2.01534534008821,9.17329059302083));
#12544=CARTESIAN_POINT('Ctrl Pts',(2.51136433889133,-2.0197024386445,9.172943288152));
#12545=CARTESIAN_POINT('Ctrl Pts',(2.50379313025655,-2.02908337737495,9.17219575804493));
#12546=CARTESIAN_POINT('Ctrl Pts',(2.49971600939352,-2.03410404492456,9.17179581252982));
#12547=CARTESIAN_POINT('Ctrl Pts',(2.48835116928453,-2.04801321648941,9.1706880687874));
#12548=CARTESIAN_POINT('Ctrl Pts',(2.48103088544622,-2.05687516182828,9.16998258709342));
#12549=CARTESIAN_POINT('Ctrl Pts',(2.43940627810851,-2.10672042705616,9.1660149409455));
#12550=CARTESIAN_POINT('Ctrl Pts',(2.40413183363912,-2.14688724595349,9.16281934083323));
#12551=CARTESIAN_POINT('Ctrl Pts',(2.19407341603368,-2.37440551977974,9.14460141689181));
#12552=CARTESIAN_POINT('Ctrl Pts',(1.9984304037041,-2.54127222198343,9.13070291672181));
#12553=CARTESIAN_POINT('Ctrl Pts',(1.64786297988882,-2.77449501317888,9.10692510198949));
#12554=CARTESIAN_POINT('Ctrl Pts',(1.50387583268631,-2.85510453037785,9.09743162937913));
#12555=CARTESIAN_POINT('Ctrl Pts',(1.33447161178886,-2.93356163941016,9.08620296970295));
#12556=CARTESIAN_POINT('Ctrl Pts',(1.31448135868329,-2.94257320999233,9.08487737416152));
#12557=CARTESIAN_POINT('Ctrl Pts',(1.28240218132652,-2.95664233112758,9.08274851622357));
#12558=CARTESIAN_POINT('Ctrl Pts',(1.27037145130872,-2.96183145986221,9.08194976638928));
#12559=CARTESIAN_POINT('Ctrl Pts',(1.24902658658154,-2.97088401352726,9.08053184996504));
#12560=CARTESIAN_POINT('Ctrl Pts',(1.23972528149492,-2.9747773796658,9.07991371464923));
#12561=CARTESIAN_POINT('Ctrl Pts',(1.22037796719648,-2.98276933384184,9.078627346075));
#12562=CARTESIAN_POINT('Ctrl Pts',(1.21032923814628,-2.98686096301863,9.07795888584223));
#12563=CARTESIAN_POINT('Ctrl Pts',(1.18432710459764,-2.9972957172052,9.0762282075589));
#12564=CARTESIAN_POINT('Ctrl Pts',(1.16834348907939,-3.00356218184378,9.07516341484057));
#12565=CARTESIAN_POINT('Ctrl Pts',(1.09999073722591,-3.02973209939585,9.07060538648529));
#12566=CARTESIAN_POINT('Ctrl Pts',(1.04716008443043,-3.04839487894896,9.06707093559214));
#12567=CARTESIAN_POINT('Ctrl Pts',(0.90658853443234,-3.09396735397512,9.05763037682584));
#12568=CARTESIAN_POINT('Ctrl Pts',(0.818143193577447,-3.11852143886941,
9.05165293920046));
#12569=CARTESIAN_POINT('Ctrl Pts',(0.490857110636059,-3.19450050766365,
9.02942785652711));
#12570=CARTESIAN_POINT('Ctrl Pts',(0.247454931007985,-3.22250291739819,
9.01262439416313));
#12571=CARTESIAN_POINT('Ctrl Pts',(-0.0876520562247414,-3.22283972451628,
8.99033885097901));
#12572=CARTESIAN_POINT('Ctrl Pts',(-0.178515946018587,-3.21908591656147,
8.98439165540514));
#12573=CARTESIAN_POINT('Ctrl Pts',(-0.282951967910212,-3.2103346790872,
8.97775364388958));
#12574=CARTESIAN_POINT('Ctrl Pts',(-0.296788736266056,-3.20908507682182,
8.97687820494529));
#12575=CARTESIAN_POINT('Ctrl Pts',(-0.317653036887747,-3.20706471351594,
8.97556466914158));
#12576=CARTESIAN_POINT('Ctrl Pts',(-0.324686611909918,-3.20636026279526,
8.97512298320988));
#12577=CARTESIAN_POINT('Ctrl Pts',(-0.337270918242436,-3.20505804261154,
8.97433480502017));
#12578=CARTESIAN_POINT('Ctrl Pts',(-0.342822445514734,-3.20446898896062,
8.97398783047988));
#12579=CARTESIAN_POINT('Ctrl Pts',(-0.354847837520738,-3.20316140707925,
8.97323782077653));
#12580=CARTESIAN_POINT('Ctrl Pts',(-0.361321043459785,-3.2024376797873,
8.97283508248482));
#12581=CARTESIAN_POINT('Ctrl Pts',(-0.379417873678807,-3.20035882087031,
8.97171181922907));
#12582=CARTESIAN_POINT('Ctrl Pts',(-0.391036516503718,-3.1989599806402,
8.97099371736013));
#12583=CARTESIAN_POINT('Ctrl Pts',(-0.458988538091207,-3.19040306768619,
8.9668104601808));
#12584=CARTESIAN_POINT('Ctrl Pts',(-0.515136280018205,-3.18181987875896,
8.96342063625298));
#12585=CARTESIAN_POINT('Ctrl Pts',(-0.820749016689553,-3.12679845796169,
8.94519273797376));
#12586=CARTESIAN_POINT('Ctrl Pts',(-1.06430605591794,-3.052503420149,8.93142271107741));
#12587=CARTESIAN_POINT('Ctrl Pts',(-1.35706233084856,-2.92384247699667,
8.9133583200562));
#12588=CARTESIAN_POINT('Ctrl Pts',(-1.41662675287091,-2.8954507025908,8.90960221584586));
#12589=CARTESIAN_POINT('Ctrl Pts',(-1.47525556020637,-2.8652641404555,8.90579936292296));
#12590=CARTESIAN_POINT('Ctrl Pts',(-1.47525540497551,-2.86526422038013,
8.65558740743848));
#12591=CARTESIAN_POINT('Ctrl Pts',(-1.4716703386366,-2.86711008452629,8.65581666119134));
#12592=CARTESIAN_POINT('Ctrl Pts',(-1.46808162110067,-2.86894931632668,
8.65604606387195));
#12593=CARTESIAN_POINT('Ctrl Pts',(-1.38229776875123,-2.91271074979506,
8.66152776812017));
#12594=CARTESIAN_POINT('Ctrl Pts',(-1.29834902590854,-2.9510877474239,8.66685272648349));
#12595=CARTESIAN_POINT('Ctrl Pts',(-1.16075934891695,-3.00697844890102,
8.67560917369799));
#12596=CARTESIAN_POINT('Ctrl Pts',(-1.10810194889063,-3.02677900553692,
8.67896655367161));
#12597=CARTESIAN_POINT('Ctrl Pts',(-1.03870922200339,-3.05081896214508,
8.683410516769));
#12598=CARTESIAN_POINT('Ctrl Pts',(-1.02241823841246,-3.05631708361633,
8.68445516869137));
#12599=CARTESIAN_POINT('Ctrl Pts',(-0.995770867771936,-3.06507353801751,
8.6861664584646));
#12600=CARTESIAN_POINT('Ctrl Pts',(-0.985440497902606,-3.06841040851662,
8.68683049147229));
#12601=CARTESIAN_POINT('Ctrl Pts',(-0.965484058273281,-3.07474547626349,
8.68811455985541));
#12602=CARTESIAN_POINT('Ctrl Pts',(-0.955860378730679,-3.07775082540322,
8.68873435070027));
#12603=CARTESIAN_POINT('Ctrl Pts',(-0.933709097689958,-3.08455446537566,
8.69016233101586));
#12604=CARTESIAN_POINT('Ctrl Pts',(-0.921172202562161,-3.08832166298787,
8.69097153064602));
#12605=CARTESIAN_POINT('Ctrl Pts',(-0.88761396206841,-3.09818302358101,
8.69314041771855));
#12606=CARTESIAN_POINT('Ctrl Pts',(-0.866553189475032,-3.10413951440997,
8.6945045724049));
#12607=CARTESIAN_POINT('Ctrl Pts',(-0.688300452419962,-3.15259824695472,
8.70607743356053));
#12608=CARTESIAN_POINT('Ctrl Pts',(-0.528180312545542,-3.18333855606427,
8.71666816677794));
#12609=CARTESIAN_POINT('Ctrl Pts',(-0.114852080147411,-3.23064300032144,
8.74440659358943));
#12610=CARTESIAN_POINT('Ctrl Pts',(0.139242916007588,-3.22968286062258,
8.7618825022252));
#12611=CARTESIAN_POINT('Ctrl Pts',(0.44790830719467,-3.19199450129588,8.78224033719575));
#12612=CARTESIAN_POINT('Ctrl Pts',(0.505022415411805,-3.1834578824089,8.78596562762726));
#12613=CARTESIAN_POINT('Ctrl Pts',(0.573460161699617,-3.17134030070757,
8.79035506889609));
#12614=CARTESIAN_POINT('Ctrl Pts',(0.585028942337611,-3.16922656284242,
8.7910944822084));
#12615=CARTESIAN_POINT('Ctrl Pts',(0.603000158094171,-3.16584127394099,
8.79223881040948));
#12616=CARTESIAN_POINT('Ctrl Pts',(0.60941059694925,-3.16461354490051,8.79264614763672));
#12617=CARTESIAN_POINT('Ctrl Pts',(0.621295875164245,-3.16229981974072,
8.79339973455768));
#12618=CARTESIAN_POINT('Ctrl Pts',(0.626771575046279,-3.1612190857196,8.79374626978552));
#12619=CARTESIAN_POINT('Ctrl Pts',(0.639158763553322,-3.1587407866198,8.79452874988903));
#12620=CARTESIAN_POINT('Ctrl Pts',(0.646068471747284,-3.157334764343,8.79496420565854));
#12621=CARTESIAN_POINT('Ctrl Pts',(0.666501705666531,-3.1531070206157,8.79624905433342));
#12622=CARTESIAN_POINT('Ctrl Pts',(0.680011967978001,-3.15022096786465,
8.79709485737361));
#12623=CARTESIAN_POINT('Ctrl Pts',(0.780161081353696,-3.12815287457219,
8.80333975732255));
#12624=CARTESIAN_POINT('Ctrl Pts',(0.866001731128185,-3.10548479398337,
8.80855425541047));
#12625=CARTESIAN_POINT('Ctrl Pts',(1.1868328461683,-3.00642077449665,8.82789033869272));
#12626=CARTESIAN_POINT('Ctrl Pts',(1.41370747229911,-2.90664476623202,8.84130638490641));
#12627=CARTESIAN_POINT('Ctrl Pts',(1.70586383023312,-2.73578141405782,8.86057975248932));
#12628=CARTESIAN_POINT('Ctrl Pts',(1.78275697294445,-2.68630732155295,8.86585662164684));
#12629=CARTESIAN_POINT('Ctrl Pts',(1.90309176305783,-2.60143807419683,8.87454077949634));
#12630=CARTESIAN_POINT('Ctrl Pts',(1.94789647938893,-2.56806095112801,8.87787552514703));
#12631=CARTESIAN_POINT('Ctrl Pts',(2.00528932027912,-2.52294001700273,8.88229345042803));
#12632=CARTESIAN_POINT('Ctrl Pts',(2.01868440865049,-2.51223502642831,8.8833353019335));
#12633=CARTESIAN_POINT('Ctrl Pts',(2.0404093254302,-2.49458712376726,8.88504299161517));
#12634=CARTESIAN_POINT('Ctrl Pts',(2.04879077891802,-2.48770807633137,8.8857062434288));
#12635=CARTESIAN_POINT('Ctrl Pts',(2.06489764993535,-2.47435181247372,8.88698949385681));
#12636=CARTESIAN_POINT('Ctrl Pts',(2.07262771297458,-2.46788037723152,8.88760925177809));
#12637=CARTESIAN_POINT('Ctrl Pts',(2.09033681141244,-2.45291282786906,8.88903814732017));
#12638=CARTESIAN_POINT('Ctrl Pts',(2.10029458749696,-2.44439194153583,8.88984830148738));
#12639=CARTESIAN_POINT('Ctrl Pts',(2.12678817129933,-2.42143992745245,8.89202194047289));
#12640=CARTESIAN_POINT('Ctrl Pts',(2.14322877241587,-2.40690042138002,8.8933899271966));
#12641=CARTESIAN_POINT('Ctrl Pts',(2.2827557645539,-2.28094442635079,8.90516694677602));
#12642=CARTESIAN_POINT('Ctrl Pts',(2.39719183393805,-2.1603558549026,8.91597398164589));
#12643=CARTESIAN_POINT('Ctrl Pts',(2.66492841174709,-1.83063607487209,8.94431876069702));
#12644=CARTESIAN_POINT('Ctrl Pts',(2.8032466602291,-1.61086202739786,8.96219378389989));
#12645=CARTESIAN_POINT('Ctrl Pts',(2.93522607940133,-1.33157090491372,8.98233057654168));
#12646=CARTESIAN_POINT('Ctrl Pts',(2.95559521241621,-1.28572579333039,8.98555632963982));
#12647=CARTESIAN_POINT('Ctrl Pts',(2.97922195121041,-1.2290163445903,8.98943376617703));
#12648=CARTESIAN_POINT('Ctrl Pts',(2.98350227188833,-1.21858886108651,8.9901421264491));
#12649=CARTESIAN_POINT('Ctrl Pts',(2.99013349329532,-1.20218984925436,8.99124868803198));
#12650=CARTESIAN_POINT('Ctrl Pts',(2.99252136704051,-1.19623351018502,8.99164906915882));
#12651=CARTESIAN_POINT('Ctrl Pts',(2.99695663195689,-1.18507374238135,8.99239629464451));
#12652=CARTESIAN_POINT('Ctrl Pts',(2.99900824882141,-1.17987217646759,8.99274338379594));
#12653=CARTESIAN_POINT('Ctrl Pts',(3.00367049331907,-1.16796102746749,8.99353549271096));
#12654=CARTESIAN_POINT('Ctrl Pts',(3.00627217808673,-1.16124803024697,8.9939799709226));
#12655=CARTESIAN_POINT('Ctrl Pts',(3.01423580993555,-1.14049373062079,8.99534831122658));
#12656=CARTESIAN_POINT('Ctrl Pts',(3.01952213308221,-1.12642335541242,8.99626775216012));
#12657=CARTESIAN_POINT('Ctrl Pts',(3.07921875309348,-0.964090953341672,
9.00678673019368));
#12658=CARTESIAN_POINT('Ctrl Pts',(3.12276612550697,-0.812037597486608,
9.01579504065694));
#12659=CARTESIAN_POINT('Ctrl Pts',(3.19991700970102,-0.441767162907315,
9.0370583626955));
#12660=CARTESIAN_POINT('Ctrl Pts',(3.22262092942917,-0.2221226451123,9.04916950956993));
#12661=CARTESIAN_POINT('Ctrl Pts',(3.22280503408505,0.0933690777550868,
9.06741248524487));
#12662=CARTESIAN_POINT('Ctrl Pts',(3.2186379330999,0.188566570256866,9.07302010788799));
#12663=CARTESIAN_POINT('Ctrl Pts',(3.20856656757026,0.302638112184638,9.07992375128113));
#12664=CARTESIAN_POINT('Ctrl Pts',(3.20669875230241,0.321826556668248,9.08109126048284));
#12665=CARTESIAN_POINT('Ctrl Pts',(3.20334236530984,0.353369598652563,9.08302119681374));
#12666=CARTESIAN_POINT('Ctrl Pts',(3.20195418596328,0.36573455784507,9.08378045261212));
#12667=CARTESIAN_POINT('Ctrl Pts',(3.19932471440276,0.387992713683405,9.08515220645007));
#12668=CARTESIAN_POINT('Ctrl Pts',(3.19810904369534,0.397888822587316,9.08576388625864));
#12669=CARTESIAN_POINT('Ctrl Pts',(3.19541617396367,0.418999995317155,9.08707266108792));
#12670=CARTESIAN_POINT('Ctrl Pts',(3.19392581370026,0.430213217199748,9.08777016578625));
#12671=CARTESIAN_POINT('Ctrl Pts',(3.18973678696645,0.460508635314292,9.08966111865225));
#12672=CARTESIAN_POINT('Ctrl Pts',(3.18692596923275,0.479574617682628,9.09085810916952));
#12673=CARTESIAN_POINT('Ctrl Pts',(3.17172843103085,0.576619875930451,9.09698707409035));
#12674=CARTESIAN_POINT('Ctrl Pts',(3.15665091278065,0.654144462051568,9.10200395413512));
#12675=CARTESIAN_POINT('Ctrl Pts',(3.07883713311036,0.988243965040913,9.12416981602641));
#12676=CARTESIAN_POINT('Ctrl Pts',(2.9875461356485,1.23709004365705,9.14220635502869));
#12677=CARTESIAN_POINT('Ctrl Pts',(2.80552433449375,1.59161619042313,9.16903199702341));
#12678=CARTESIAN_POINT('Ctrl Pts',(2.73665244334882,1.70732273639555,9.17796761178809));
#12679=CARTESIAN_POINT('Ctrl Pts',(2.65230421274883,1.83074399138336,9.18744590603594));
#12680=CARTESIAN_POINT('Ctrl Pts',(2.64378030160727,1.84303199541076,9.18838890461649));
#12681=CARTESIAN_POINT('Ctrl Pts',(2.6310349591373,1.86113519794421,9.18977663021936));
#12682=CARTESIAN_POINT('Ctrl Pts',(2.62687926452469,1.86699612029948,9.19022566594569));
#12683=CARTESIAN_POINT('Ctrl Pts',(2.61945526623255,1.87739258599433,9.19102169111578));
#12684=CARTESIAN_POINT('Ctrl Pts',(2.61619473339349,1.88193356216186,9.19136920460908));
#12685=CARTESIAN_POINT('Ctrl Pts',(2.60916000045344,1.89167728899086,9.19211448556203));
#12686=CARTESIAN_POINT('Ctrl Pts',(2.60538205787526,1.896877225299,9.19251198783122));
#12687=CARTESIAN_POINT('Ctrl Pts',(2.59490949045635,1.91120128828204,9.19360643583568));
#12688=CARTESIAN_POINT('Ctrl Pts',(2.58818224824883,1.92030161347566,9.19430115432792));
#12689=CARTESIAN_POINT('Ctrl Pts',(2.55099350602217,1.97005850746889,9.19809741611763));
#12690=CARTESIAN_POINT('Ctrl Pts',(2.51961999814508,2.01002838935398,9.20113895943597));
#12691=CARTESIAN_POINT('Ctrl Pts',(2.32310159242365,2.24855689683973,9.21935474595476));
#12692=CARTESIAN_POINT('Ctrl Pts',(2.13551256692765,2.42743190190348,9.23335936385393));
#12693=CARTESIAN_POINT('Ctrl Pts',(1.79581040655307,2.68116346683125,9.25729820196802));
#12694=CARTESIAN_POINT('Ctrl Pts',(1.65562654777068,2.76992104126593,9.26684091373934));
#12695=CARTESIAN_POINT('Ctrl Pts',(1.48986637585403,2.85777836006941,9.27812442829722));
#12696=CARTESIAN_POINT('Ctrl Pts',(1.47037600372026,2.86785518190884,9.27945083938159));
#12697=CARTESIAN_POINT('Ctrl Pts',(1.43908328106106,2.88363114730782,9.2815806449037));
#12698=CARTESIAN_POINT('Ctrl Pts',(1.4273462104678,2.88945878514584,9.28237951914445));
#12699=CARTESIAN_POINT('Ctrl Pts',(1.40651728978323,2.89964279004675,9.28379743890598));
#12700=CARTESIAN_POINT('Ctrl Pts',(1.39743987537588,2.90402840677751,9.28441545184472));
#12701=CARTESIAN_POINT('Ctrl Pts',(1.37855574517857,2.91304294802772,9.28570134856046));
#12702=CARTESIAN_POINT('Ctrl Pts',(1.36874595671442,2.91766510432482,9.28636945809643));
#12703=CARTESIAN_POINT('Ctrl Pts',(1.34336077950514,2.92946984265458,9.28809876061871));
#12704=CARTESIAN_POINT('Ctrl Pts',(1.32775119802434,2.93657768171548,9.28916252167605));
#12705=CARTESIAN_POINT('Ctrl Pts',(1.26102660271578,2.96632002912187,9.29371188402403));
#12706=CARTESIAN_POINT('Ctrl Pts',(1.209386592148,2.98774598102589,9.29723850925931));
#12707=CARTESIAN_POINT('Ctrl Pts',(1.07183342575039,3.04066774856621,9.30665339166827));
#12708=CARTESIAN_POINT('Ctrl Pts',(0.985095799150493,3.06986498538147,9.31261250319956));
#12709=CARTESIAN_POINT('Ctrl Pts',(0.660406553527635,3.16398225574356,9.3349711211711));
#12710=CARTESIAN_POINT('Ctrl Pts',(0.416502584125903,3.20521926836399,9.35194162961529));
#12711=CARTESIAN_POINT('Ctrl Pts',(0.0813536956044349,3.22295392914406,
9.37424571010358));
#12712=CARTESIAN_POINT('Ctrl Pts',(-0.00775475380571619,3.22397168958091,
9.38006951616286));
#12713=CARTESIAN_POINT('Ctrl Pts',(-0.11061850414362,3.2208806655178,9.38658716508006));
#12714=CARTESIAN_POINT('Ctrl Pts',(-0.124435534088911,3.22037645764459,
9.38745833889117));
#12715=CARTESIAN_POINT('Ctrl Pts',(-0.145295944476533,3.21948076550597,
9.38876667457754));
#12716=CARTESIAN_POINT('Ctrl Pts',(-0.152341776959527,3.21915505935725,
9.38920738501686));
#12717=CARTESIAN_POINT('Ctrl Pts',(-0.164959541589484,3.21853026184113,
9.38999440652327));
#12718=CARTESIAN_POINT('Ctrl Pts',(-0.170531796884725,3.21823983017888,
9.39034119501025));
#12719=CARTESIAN_POINT('Ctrl Pts',(-0.182614166329064,3.21757861531134,
9.39109144824682));
#12720=CARTESIAN_POINT('Ctrl Pts',(-0.189123898343437,3.21720254760361,
9.39149461285096));
#12721=CARTESIAN_POINT('Ctrl Pts',(-0.207353222164459,3.21609391761046,
9.39262075468844));
#12722=CARTESIAN_POINT('Ctrl Pts',(-0.219070159062452,3.215317048275,9.3933412872343));
#12723=CARTESIAN_POINT('Ctrl Pts',(-0.288154387947364,3.2103571571785,9.39757153764361));
#12724=CARTESIAN_POINT('Ctrl Pts',(-0.345409595099409,3.20470266771449,
9.40100391604283));
#12725=CARTESIAN_POINT('Ctrl Pts',(-0.653570588365002,3.16591298818201,
9.41922684568966));
#12726=CARTESIAN_POINT('Ctrl Pts',(-0.900080585264105,3.1048415486136,9.43296222679318));
#12727=CARTESIAN_POINT('Ctrl Pts',(-1.28986509138494,2.95788461482416,9.45649447512827));
#12728=CARTESIAN_POINT('Ctrl Pts',(-1.43817805786563,2.88867908232728,9.46591447254841));
#12729=CARTESIAN_POINT('Ctrl Pts',(-1.59967309308622,2.79779251669632,9.47706061546423));
#12730=CARTESIAN_POINT('Ctrl Pts',(-1.61864398385091,2.78685998724867,9.47838430205226));
#12731=CARTESIAN_POINT('Ctrl Pts',(-1.6487763986443,2.76908383952427,9.48051053128794));
#12732=CARTESIAN_POINT('Ctrl Pts',(-1.66001038279993,2.76236392318277,9.48130857737277));
#12733=CARTESIAN_POINT('Ctrl Pts',(-1.67982063588193,2.75034939113107,9.48272550560085));
#12734=CARTESIAN_POINT('Ctrl Pts',(-1.6884136421585,2.74508260555808,9.48334335958267));
#12735=CARTESIAN_POINT('Ctrl Pts',(-1.70620492816868,2.73406291229642,9.4846294023192));
#12736=CARTESIAN_POINT('Ctrl Pts',(-1.71539913390263,2.72830369865587,9.48529781918662));
#12737=CARTESIAN_POINT('Ctrl Pts',(-1.73907379116622,2.71330700880579,9.48702894104857));
#12738=CARTESIAN_POINT('Ctrl Pts',(-1.75350964528765,2.7040000888737,9.48809422487012));
#12739=CARTESIAN_POINT('Ctrl Pts',(-1.81480001518858,2.66378844776997,9.4926593151154));
#12740=CARTESIAN_POINT('Ctrl Pts',(-1.86091488820877,2.63177946059573,9.49620050363308));
#12741=CARTESIAN_POINT('Ctrl Pts',(-1.98035413162681,2.54416587160632,9.50566416782904));
#12742=CARTESIAN_POINT('Ctrl Pts',(-2.05216952081148,2.48660012856006,9.51165842230677));
#12743=CARTESIAN_POINT('Ctrl Pts',(-2.30359672599659,2.26674337127322,9.53375417034777));
#12744=CARTESIAN_POINT('Ctrl Pts',(-2.46723286329789,2.08744593288653,9.55039719987753));
#12745=CARTESIAN_POINT('Ctrl Pts',(-2.663655123612,1.81649378285743,9.57266761024716));
#12746=CARTESIAN_POINT('Ctrl Pts',(-2.71479873660925,1.73913184686213,9.57873629335791));
#12747=CARTESIAN_POINT('Ctrl Pts',(-2.76972400385542,1.64770782914626,9.58549209160489));
#12748=CARTESIAN_POINT('Ctrl Pts',(-2.77683015815761,1.63570365196964,9.58637115117821));
#12749=CARTESIAN_POINT('Ctrl Pts',(-2.78742485295167,1.61753836627179,9.58768894027755));
#12750=CARTESIAN_POINT('Ctrl Pts',(-2.79097129348321,1.6114114677634,9.5881312942419));
#12751=CARTESIAN_POINT('Ctrl Pts',(-2.7972776527689,1.60043320605524,9.58892006004445));
#12752=CARTESIAN_POINT('Ctrl Pts',(-2.80004517463904,1.59558632962392,9.58926695862875));
#12753=CARTESIAN_POINT('Ctrl Pts',(-2.80600878783743,1.58507870531524,9.59001610059725));
#12754=CARTESIAN_POINT('Ctrl Pts',(-2.8092003384224,1.57941548676574,9.59041805113255));
#12755=CARTESIAN_POINT('Ctrl Pts',(-2.81806444010061,1.5635747920973,9.59153742176606));
#12756=CARTESIAN_POINT('Ctrl Pts',(-2.82369903394965,1.55337603122321,9.59225244416452));
#12757=CARTESIAN_POINT('Ctrl Pts',(-2.85609538871937,1.49397902119982,9.59638521905967));
#12758=CARTESIAN_POINT('Ctrl Pts',(-2.88162816616604,1.44411709294727,9.59972972498443));
#12759=CARTESIAN_POINT('Ctrl Pts',(-3.01575700741424,1.16444211187001,9.61794643979218));
#12760=CARTESIAN_POINT('Ctrl Pts',(-3.09817900032483,0.923054716826732,
9.63173881364856));
#12761=CARTESIAN_POINT('Ctrl Pts',(-3.18570859213243,0.514082174206023,
9.65536176966456));
#12762=CARTESIAN_POINT('Ctrl Pts',(-3.20773697381939,0.351329983190187,
9.66481285743821));
#12763=CARTESIAN_POINT('Ctrl Pts',(-3.21855927477537,0.165751795175915,
9.6759937772376));
#12764=CARTESIAN_POINT('Ctrl Pts',(-3.21961158512325,0.143870314831026,
9.67731813157889));
#12765=CARTESIAN_POINT('Ctrl Pts',(-3.22093630437289,0.108895955216128,
9.67944522388613));
#12766=CARTESIAN_POINT('Ctrl Pts',(-3.2213521450291,0.0958089539899059,
9.6802434592628));
#12767=CARTESIAN_POINT('Ctrl Pts',(-3.22194692165271,0.0726442245217949,
9.68166059782442));
#12768=CARTESIAN_POINT('Ctrl Pts',(-3.2221583542197,0.0625674513636109,
9.68227847172605));
#12769=CARTESIAN_POINT('Ctrl Pts',(-3.22249918715289,0.0416439451329804,
9.68356443044205));
#12770=CARTESIAN_POINT('Ctrl Pts',(-3.2226211001604,0.0307972330203178,
9.68423274274175));
#12771=CARTESIAN_POINT('Ctrl Pts',(-3.22279453240761,0.00278159494860291,
9.6859633239097));
#12772=CARTESIAN_POINT('Ctrl Pts',(-3.22276361556241,-0.0143873279685257,
9.68702816867261));
#12773=CARTESIAN_POINT('Ctrl Pts',(-3.22204654739059,-0.0876190338672722,
9.69158893827817));
#12774=CARTESIAN_POINT('Ctrl Pts',(-3.22003467467528,-0.143656205561677,
9.69512614878719));
#12775=CARTESIAN_POINT('Ctrl Pts',(-3.21087253438286,-0.29129731510064,
9.70457654195249));
#12776=CARTESIAN_POINT('Ctrl Pts',(-3.20126549255612,-0.382692157390562,
9.71056125480832));
#12777=CARTESIAN_POINT('Ctrl Pts',(-3.152003315448,-0.714310667014597,9.73273901207245));
#12778=CARTESIAN_POINT('Ctrl Pts',(-3.08908152802351,-0.950223591043525,
9.74948244496187));
#12779=CARTESIAN_POINT('Ctrl Pts',(-2.96678166476351,-1.26202453511395,
9.77176154231382));
#12780=CARTESIAN_POINT('Ctrl Pts',(-2.92973094659563,-1.34580062619013,
9.77775345703828));
#12781=CARTESIAN_POINT('Ctrl Pts',(-2.88299531550636,-1.4403642263741,9.78443470487312));
#12782=CARTESIAN_POINT('Ctrl Pts',(-2.87675075076475,-1.45279600366016,
9.78531135087426));
#12783=CARTESIAN_POINT('Ctrl Pts',(-2.86721094744229,-1.47148528569103,
9.78662623839569));
#12784=CARTESIAN_POINT('Ctrl Pts',(-2.86397538915655,-1.47777282953404,
9.78706808122251));
#12785=CARTESIAN_POINT('Ctrl Pts',(-2.85814923070862,-1.48900358710928,
9.78785629887589));
#12786=CARTESIAN_POINT('Ctrl Pts',(-2.85556647007918,-1.49395075017566,
9.78820315755586));
#12787=CARTESIAN_POINT('Ctrl Pts',(-2.84994461869872,-1.50465131123633,
9.78895262920103));
#12788=CARTESIAN_POINT('Ctrl Pts',(-2.84690096056134,-1.51040220490367,
9.78935494707622));
#12789=CARTESIAN_POINT('Ctrl Pts',(-2.83834560884316,-1.52644952754833,
9.79047635235176));
#12790=CARTESIAN_POINT('Ctrl Pts',(-2.83279526655956,-1.53672539605512,
9.79119302804344));
#12791=CARTESIAN_POINT('Ctrl Pts',(-2.80009072036655,-1.59649505770504,
9.79535464469759));
#12792=CARTESIAN_POINT('Ctrl Pts',(-2.77169381693364,-1.64530203835713,
9.79872514163799));
#12793=CARTESIAN_POINT('Ctrl Pts',(-2.60865283788858,-1.90931430755236,
9.81694364049441));
#12794=CARTESIAN_POINT('Ctrl Pts',(-2.45021759577852,-2.10879387516649,
9.83071915178048));
#12795=CARTESIAN_POINT('Ctrl Pts',(-2.15374024844893,-2.40298652498989,
9.85431126676552));
#12796=CARTESIAN_POINT('Ctrl Pts',(-2.02887418081197,-2.50930277753416,
9.86374898835794));
#12797=CARTESIAN_POINT('Ctrl Pts',(-1.87873857697021,-2.61857603550263,
9.87491742070084));
#12798=CARTESIAN_POINT('Ctrl Pts',(-1.86086543534739,-2.63130744865655,
9.87624399463155));
#12799=CARTESIAN_POINT('Ctrl Pts',(-1.83211329116219,-2.65134874795622,
9.87837398979661));
#12800=CARTESIAN_POINT('Ctrl Pts',(-1.82131709964672,-2.65877665656885,
9.87917288903861));
#12801=CARTESIAN_POINT('Ctrl Pts',(-1.80213616556458,-2.67180171971412,
9.88059080996733));
#12802=CARTESIAN_POINT('Ctrl Pts',(-1.79376985189442,-2.67742579793915,
9.8812087987458));
#12803=CARTESIAN_POINT('Ctrl Pts',(-1.77635023594889,-2.68901747386498,
9.88249460191662));
#12804=CARTESIAN_POINT('Ctrl Pts',(-1.76729293966667,-2.69497881184812,
9.88316264184022));
#12805=CARTESIAN_POINT('Ctrl Pts',(-1.74383422122608,-2.71024977440604,
9.88489167062717));
#12806=CARTESIAN_POINT('Ctrl Pts',(-1.72938840997827,-2.71949027207282,
9.88595522642143));
#12807=CARTESIAN_POINT('Ctrl Pts',(-1.66755962161982,-2.75834819943891,
9.89050285297789));
#12808=CARTESIAN_POINT('Ctrl Pts',(-1.61948677151221,-2.78684442464143,
9.89402791235606));
#12809=CARTESIAN_POINT('Ctrl Pts',(-1.53916957404902,-2.83167414442461,
9.89990366609363));
#12810=CARTESIAN_POINT('Ctrl Pts',(-1.50735021788572,-2.84873937595535,
9.90222798148366));
#12811=CARTESIAN_POINT('Ctrl Pts',(-1.47525538675478,-2.86526422976154,
9.90456889022841));
#12812=CARTESIAN_POINT('Origin',(0.,0.,4.68922655072688));
#12813=CARTESIAN_POINT('',(-1.47525557920441,-2.86526413067387,11.4032056183244));
#12814=CARTESIAN_POINT('',(-1.47708659324034,-2.8687591534968,11.1570143151468));
#12815=CARTESIAN_POINT('',(-1.47525540501186,-2.86526422036142,4.68922655072688));
#12816=CARTESIAN_POINT('',(3.22274985762459,0.000957956508987824,10.5578331123621));
#12817=CARTESIAN_POINT('Ctrl Pts',(-1.47525557920443,-2.86526413067385,
11.4032056183244));
#12818=CARTESIAN_POINT('Ctrl Pts',(-1.55962558463346,-2.8218240443327,11.3967822218367));
#12819=CARTESIAN_POINT('Ctrl Pts',(-1.64209689519603,-2.77464724284609,
11.3903638243335));
#12820=CARTESIAN_POINT('Ctrl Pts',(-1.8010868080994,-2.67411042193256,11.3778439993238));
#12821=CARTESIAN_POINT('Ctrl Pts',(-1.87756866665631,-2.62097685199999,
11.3717490710442));
#12822=CARTESIAN_POINT('Ctrl Pts',(-1.96276323435873,-2.55614418275809,
11.364967581164));
#12823=CARTESIAN_POINT('Ctrl Pts',(-1.97382183989785,-2.54761456232175,
11.3640874949074));
#12824=CARTESIAN_POINT('Ctrl Pts',(-1.99040603044308,-2.53465018909514,
11.36276837734));
#12825=CARTESIAN_POINT('Ctrl Pts',(-1.99597284166916,-2.53026879297454,
11.3623257123631));
#12826=CARTESIAN_POINT('Ctrl Pts',(-2.00590142234858,-2.52240128106146,
11.361536495505));
#12827=CARTESIAN_POINT('Ctrl Pts',(-2.01026860632467,-2.5189221645156,11.361189455717));
#12828=CARTESIAN_POINT('Ctrl Pts',(-2.01970132753046,-2.51136743195457,
11.3604401186348));
#12829=CARTESIAN_POINT('Ctrl Pts',(-2.02476356552014,-2.5072878447072,11.3600381138118));
#12830=CARTESIAN_POINT('Ctrl Pts',(-2.03886134501968,-2.49585609985865,
11.358918856345));
#12831=CARTESIAN_POINT('Ctrl Pts',(-2.04786952959166,-2.48847014345071,
11.3582039994555));
#12832=CARTESIAN_POINT('Ctrl Pts',(-2.09988183790694,-2.44535069664492,
11.35407706346));
#12833=CARTESIAN_POINT('Ctrl Pts',(-2.1419931595153,-2.40854934434578,11.3507379774741));
#12834=CARTESIAN_POINT('Ctrl Pts',(-2.37021804312523,-2.19837898327467,
11.3325154773323));
#12835=CARTESIAN_POINT('Ctrl Pts',(-2.53627271948698,-2.00453282905629,
11.3187142659827));
#12836=CARTESIAN_POINT('Ctrl Pts',(-2.76903105961657,-1.65694280405326,
11.2950857487114));
#12837=CARTESIAN_POINT('Ctrl Pts',(-2.84970803114943,-1.5139835367721,11.2856392318007));
#12838=CARTESIAN_POINT('Ctrl Pts',(-2.9284397823553,-1.34567383179771,11.2744631234362));
#12839=CARTESIAN_POINT('Ctrl Pts',(-2.93752060996286,-1.32573385345459,
11.2731385544043));
#12840=CARTESIAN_POINT('Ctrl Pts',(-2.95170357167115,-1.29372915342543,
11.2710110338555));
#12841=CARTESIAN_POINT('Ctrl Pts',(-2.95693679529346,-1.28172301146974,
11.2702125858214));
#12842=CARTESIAN_POINT('Ctrl Pts',(-2.96606890513097,-1.26041837104777,
11.268795018528));
#12843=CARTESIAN_POINT('Ctrl Pts',(-2.9699976336371,-1.25113279574154,11.2681769288483));
#12844=CARTESIAN_POINT('Ctrl Pts',(-2.97806432867333,-1.23181499568147,
11.2668904690997));
#12845=CARTESIAN_POINT('Ctrl Pts',(-2.98219531959709,-1.22178001312148,
11.2662218711312));
#12846=CARTESIAN_POINT('Ctrl Pts',(-2.9927343004414,-1.1958068636574,11.2644904360779));
#12847=CARTESIAN_POINT('Ctrl Pts',(-2.99906561952948,-1.17983814124989,
11.2634250200485));
#12848=CARTESIAN_POINT('Ctrl Pts',(-3.02553309288648,-1.11149261804459,
11.2588607112183));
#12849=CARTESIAN_POINT('Ctrl Pts',(-3.04442608431466,-1.05864796535023,
11.2553204616164));
#12850=CARTESIAN_POINT('Ctrl Pts',(-3.09061690034974,-0.917966149474457,
11.2458605009044));
#12851=CARTESIAN_POINT('Ctrl Pts',(-3.11554936373178,-0.829412029341887,
11.2398690944451));
#12852=CARTESIAN_POINT('Ctrl Pts',(-3.19227882083046,-0.504141170004751,
11.2177603009327));
#12853=CARTESIAN_POINT('Ctrl Pts',(-3.22113139770626,-0.262868800148311,
11.2010997713144));
#12854=CARTESIAN_POINT('Ctrl Pts',(-3.22327656267709,0.0718289220936422,
11.1788279631784));
#12855=CARTESIAN_POINT('Ctrl Pts',(-3.21988794949052,0.164305346742109,
11.1727728340378));
#12856=CARTESIAN_POINT('Ctrl Pts',(-3.21141494718138,0.270418373152363,
11.1660299561688));
#12857=CARTESIAN_POINT('Ctrl Pts',(-3.21021463914389,0.284313289683923,
11.1651510987502));
#12858=CARTESIAN_POINT('Ctrl Pts',(-3.20826903287116,0.305249900405214,
11.1638334582812));
#12859=CARTESIAN_POINT('Ctrl Pts',(-3.20759068519768,0.312297434322119,
11.1633910533549));
#12860=CARTESIAN_POINT('Ctrl Pts',(-3.2063358642608,0.324898539356072,11.1626021172376));
#12861=CARTESIAN_POINT('Ctrl Pts',(-3.20576818094243,0.330452881595464,
11.162255099594));
#12862=CARTESIAN_POINT('Ctrl Pts',(-3.20450790150722,0.342474785370255,
11.1615056024776));
#12863=CARTESIAN_POINT('Ctrl Pts',(-3.20381016152499,0.348941714491311,
11.1611034165942));
#12864=CARTESIAN_POINT('Ctrl Pts',(-3.20180670670892,0.366997801809824,
11.1599831434204));
#12865=CARTESIAN_POINT('Ctrl Pts',(-3.20045764061975,0.378582189160632,
11.1592674589385));
#12866=CARTESIAN_POINT('Ctrl Pts',(-3.19224953043448,0.445883227602772,
11.1551260554791));
#12867=CARTESIAN_POINT('Ctrl Pts',(-3.18399805864601,0.501424138252252,
11.1517739292324));
#12868=CARTESIAN_POINT('Ctrl Pts',(-3.13039205258962,0.807071513004934,
11.1335507822168));
#12869=CARTESIAN_POINT('Ctrl Pts',(-3.05701996011788,1.0513682098473,11.1197582529772));
#12870=CARTESIAN_POINT('Ctrl Pts',(-2.89038256268382,1.43480140705761,11.0961431925978));
#12871=CARTESIAN_POINT('Ctrl Pts',(-2.81371579365257,1.57986057230784,11.0867010159045));
#12872=CARTESIAN_POINT('Ctrl Pts',(-2.71467825288291,1.73698576107125,11.0755297628835));
#12873=CARTESIAN_POINT('Ctrl Pts',(-2.70280755151247,1.75539991284622,11.0742052885981));
#12874=CARTESIAN_POINT('Ctrl Pts',(-2.68354228510609,1.78462598023583,11.0720778915194));
#12875=CARTESIAN_POINT('Ctrl Pts',(-2.67626782295579,1.79551653212933,11.0712794713738));
#12876=CARTESIAN_POINT('Ctrl Pts',(-2.66327600920426,1.81471213071937,11.0698619363849));
#12877=CARTESIAN_POINT('Ctrl Pts',(-2.65758565277239,1.8230353022067,11.0692438509651));
#12878=CARTESIAN_POINT('Ctrl Pts',(-2.64568958411317,1.84026138311309,11.0679573829183));
#12879=CARTESIAN_POINT('Ctrl Pts',(-2.63947777987166,1.84915991158509,11.0672887723064));
#12880=CARTESIAN_POINT('Ctrl Pts',(-2.62331693753186,1.8720632801465,11.0655572676057));
#12881=CARTESIAN_POINT('Ctrl Pts',(-2.61330074964344,1.88602010941229,11.0644917941784));
#12882=CARTESIAN_POINT('Ctrl Pts',(-2.57008805902577,1.94522868562821,11.0599269059579));
#12883=CARTESIAN_POINT('Ctrl Pts',(-2.5358258108675,1.98968693227618,11.056386121302));
#12884=CARTESIAN_POINT('Ctrl Pts',(-2.44239097178528,2.10459129706378,11.0469243676953));
#12885=CARTESIAN_POINT('Ctrl Pts',(-2.38133609116377,2.17343370779137,11.0409316695951));
#12886=CARTESIAN_POINT('Ctrl Pts',(-2.14922051437845,2.41361884040175,11.0188347530876));
#12887=CARTESIAN_POINT('Ctrl Pts',(-1.96196151834427,2.56815047343785,11.0021886538032));
#12888=CARTESIAN_POINT('Ctrl Pts',(-1.6815540356189,2.75083210892615,10.9799181384292));
#12889=CARTESIAN_POINT('Ctrl Pts',(-1.60177343369292,2.79803977986581,10.973852007448));
#12890=CARTESIAN_POINT('Ctrl Pts',(-1.50775919103358,2.84832835933724,10.9670984243568));
#12891=CARTESIAN_POINT('Ctrl Pts',(-1.49541376865095,2.85482922393731,10.9662191982724));
#12892=CARTESIAN_POINT('Ctrl Pts',(-1.47673933272304,2.86450844816374,10.9649011146534));
#12893=CARTESIAN_POINT('Ctrl Pts',(-1.47044161332789,2.86774635741748,10.9644586317073));
#12894=CARTESIAN_POINT('Ctrl Pts',(-1.4591593082244,2.87350010433309,10.9636696114092));
#12895=CARTESIAN_POINT('Ctrl Pts',(-1.45417882665911,2.87602376173337,10.963322587168));
#12896=CARTESIAN_POINT('Ctrl Pts',(-1.44338283151585,2.88145898104969,10.9625731382502));
#12897=CARTESIAN_POINT('Ctrl Pts',(-1.43756507323795,2.88436587827525,10.9621710068267));
#12898=CARTESIAN_POINT('Ctrl Pts',(-1.42129386777355,2.89243447970038,10.9610510390756));
#12899=CARTESIAN_POINT('Ctrl Pts',(-1.41082102751761,2.89755716353035,10.9603356034348));
#12900=CARTESIAN_POINT('Ctrl Pts',(-1.34982066994689,2.92698573463201,10.9561985562239));
#12901=CARTESIAN_POINT('Ctrl Pts',(-1.29869011552112,2.95002816923724,10.9528503565753));
#12902=CARTESIAN_POINT('Ctrl Pts',(-1.01256423107627,3.07009087819637,10.9346274126638));
#12903=CARTESIAN_POINT('Ctrl Pts',(-0.767310856162866,3.14038305454524,
10.920832275842));
#12904=CARTESIAN_POINT('Ctrl Pts',(-0.354560208746654,3.20737609084034,
10.8972131620794));
#12905=CARTESIAN_POINT('Ctrl Pts',(-0.191050714919731,3.22125185441022,
10.8877696689721));
#12906=CARTESIAN_POINT('Ctrl Pts',(-0.00529974196128598,3.22282011361123,
10.8765969432883));
#12907=CARTESIAN_POINT('Ctrl Pts',(0.0166094839844362,3.22278166506746,
10.8752724402596));
#12908=CARTESIAN_POINT('Ctrl Pts',(0.0516120848206564,3.22236330690173,
10.8731450057374));
#12909=CARTESIAN_POINT('Ctrl Pts',(0.0647067302673271,3.22212695592169,
10.8723465771452));
#12910=CARTESIAN_POINT('Ctrl Pts',(0.0878789691468688,3.22156739892338,
10.8709290323899));
#12911=CARTESIAN_POINT('Ctrl Pts',(0.0979572267871528,3.22127670296654,
10.8703109456978));
#12912=CARTESIAN_POINT('Ctrl Pts',(0.118879945858261,3.22057493171657,10.8690244802196));
#12913=CARTESIAN_POINT('Ctrl Pts',(0.129724012814446,3.22015636393875,10.8683558734746));
#12914=CARTESIAN_POINT('Ctrl Pts',(0.15772800000834,3.21893375950179,10.8666243900052));
#12915=CARTESIAN_POINT('Ctrl Pts',(0.174883806375793,3.2180472814885,10.8655589340622));
#12916=CARTESIAN_POINT('Ctrl Pts',(0.24805145342529,3.21367973866508,10.8609942221247));
#12917=CARTESIAN_POINT('Ctrl Pts',(0.303971492726745,3.20887327249658,10.8574536002401));
#12918=CARTESIAN_POINT('Ctrl Pts',(0.451135896167595,3.19234295185569,10.8479923919375));
#12919=CARTESIAN_POINT('Ctrl Pts',(0.542047982303594,3.17816906078065,10.8420000866492));
#12920=CARTESIAN_POINT('Ctrl Pts',(0.866412014270041,3.11327598257188,10.8201165218221));
#12921=CARTESIAN_POINT('Ctrl Pts',(1.09464275278692,3.04054268406527,10.803701380165));
#12922=CARTESIAN_POINT('Ctrl Pts',(1.40014810886269,2.90428378293928,10.7814167287697));
#12923=CARTESIAN_POINT('Ctrl Pts',(1.48579228432837,2.86141644763472,10.7751427147965));
#12924=CARTESIAN_POINT('Ctrl Pts',(1.58167602929379,2.80795579861786,10.7681881096508));
#12925=CARTESIAN_POINT('Ctrl Pts',(1.59389867997548,2.80103585187668,10.7673029413118));
#12926=CARTESIAN_POINT('Ctrl Pts',(1.61223237717275,2.79049722261895,10.7659777169445));
#12927=CARTESIAN_POINT('Ctrl Pts',(1.61837715256677,2.78693799389069,10.7655339783068));
#12928=CARTESIAN_POINT('Ctrl Pts',(1.62908010294893,2.78069120525911,10.7647618914686));
#12929=CARTESIAN_POINT('Ctrl Pts',(1.6336434630515,2.77801270657873,10.7644329638803));
#12930=CARTESIAN_POINT('Ctrl Pts',(1.64357017502513,2.77215322893339,10.7637180317112));
#12931=CARTESIAN_POINT('Ctrl Pts',(1.64893088528951,2.76896792722784,10.763332314453));
#12932=CARTESIAN_POINT('Ctrl Pts',(1.65999103911105,2.76235254092839,10.7625371941743));
#12933=CARTESIAN_POINT('Ctrl Pts',(1.66568918150305,2.75892032555409,10.7621279306267));
#12934=CARTESIAN_POINT('Ctrl Pts',(1.68002616244875,2.7502239898496,10.7610990408874));
#12935=CARTESIAN_POINT('Ctrl Pts',(1.6886509886705,2.74493674707836,10.7604808637656));
#12936=CARTESIAN_POINT('Ctrl Pts',(1.71320090751304,2.72972750609882,10.7587230800798));
#12937=CARTESIAN_POINT('Ctrl Pts',(1.72906472159331,2.71970675471726,10.7575894131268));
#12938=CARTESIAN_POINT('Ctrl Pts',(1.78238551226821,2.68537029574562,10.7537832048515));
#12939=CARTESIAN_POINT('Ctrl Pts',(1.8194258288144,2.66041383834934,10.7511462510898));
#12940=CARTESIAN_POINT('Ctrl Pts',(2.13152175171637,2.44056653566909,10.7288809610057));
#12941=CARTESIAN_POINT('Ctrl Pts',(2.3749574296183,2.2043987770684,10.7109741473272));
#12942=CARTESIAN_POINT('Ctrl Pts',(2.6235119611293,1.87328845512069,10.6868328791834));
#12943=CARTESIAN_POINT('Ctrl Pts',(2.6674361742777,1.81019542813909,10.6822810029715));
#12944=CARTESIAN_POINT('Ctrl Pts',(2.71977023657144,1.72897609662921,10.6764492564413));
#12945=CARTESIAN_POINT('Ctrl Pts',(2.73032617229488,1.71225799703041,10.6752503437857));
#12946=CARTESIAN_POINT('Ctrl Pts',(2.74679918297442,1.68562896691339,10.6733425395163));
#12947=CARTESIAN_POINT('Ctrl Pts',(2.75281810458146,1.67578138291038,10.6726374192599));
#12948=CARTESIAN_POINT('Ctrl Pts',(2.76392950169765,1.65738057185449,10.6713204978176));
#12949=CARTESIAN_POINT('Ctrl Pts',(2.76903551055157,1.648835646169,10.6707092032985));
#12950=CARTESIAN_POINT('Ctrl Pts',(2.78028303274159,1.62981327583443,10.6693488582996));
#12951=CARTESIAN_POINT('Ctrl Pts',(2.78640504995678,1.61932453428315,10.6685991082391));
#12952=CARTESIAN_POINT('Ctrl Pts',(2.8040093057205,1.58876805378918,10.6664156985395));
#12953=CARTESIAN_POINT('Ctrl Pts',(2.81533487337062,1.56861136713751,10.6649764079393));
#12954=CARTESIAN_POINT('Ctrl Pts',(2.90409803173457,1.40657669581037,10.6534120647824));
#12955=CARTESIAN_POINT('Ctrl Pts',(2.97096711974397,1.25919957825345,10.6429110463986));
#12956=CARTESIAN_POINT('Ctrl Pts',(3.12180178625786,0.846990579493617,10.6136678208884));
#12957=CARTESIAN_POINT('Ctrl Pts',(3.18308411018918,0.575334432107627,10.5944506372698));
#12958=CARTESIAN_POINT('Ctrl Pts',(3.21229553976881,0.262043956539741,10.5740783550387));
#12959=CARTESIAN_POINT('Ctrl Pts',(3.21511418750193,0.224834859504792,10.5716890219465));
#12960=CARTESIAN_POINT('Ctrl Pts',(3.21795671821606,0.17608195426987,10.5686051514979));
#12961=CARTESIAN_POINT('Ctrl Pts',(3.21856563976836,0.16457681152917,10.5678807943407));
#12962=CARTESIAN_POINT('Ctrl Pts',(3.21942362377048,0.146532940447777,10.5667503557756));
#12963=CARTESIAN_POINT('Ctrl Pts',(3.21971448617815,0.139996432912698,10.5663419973613));
#12964=CARTESIAN_POINT('Ctrl Pts',(3.22021643665896,0.127885799354535,10.5655875912027));
#12965=CARTESIAN_POINT('Ctrl Pts',(3.22043295805322,0.122312060161479,10.5652412512962));
#12966=CARTESIAN_POINT('Ctrl Pts',(3.22083082272986,0.11133550795636,10.5645608762737));
#12967=CARTESIAN_POINT('Ctrl Pts',(3.22101304241447,0.105932835257869,10.5642267938024));
#12968=CARTESIAN_POINT('Ctrl Pts',(3.22139714672244,0.0936253284672779,
10.5634675083963));
#12969=CARTESIAN_POINT('Ctrl Pts',(3.22159042766405,0.0867202252337855,
10.5630427800223));
#12970=CARTESIAN_POINT('Ctrl Pts',(3.2220561204257,0.0679222451187732,10.5618898486576));
#12971=CARTESIAN_POINT('Ctrl Pts',(3.22228489092747,0.0560282619952359,
10.5611639749329));
#12972=CARTESIAN_POINT('Ctrl Pts',(3.22264488862159,0.029742450308617,10.559567243009));
#12973=CARTESIAN_POINT('Ctrl Pts',(3.22274557949115,0.0153504198564817,
10.5586979364159));
#12974=CARTESIAN_POINT('Ctrl Pts',(3.22274985762459,0.000957956508987824,
10.5578331123621));
#12975=CARTESIAN_POINT('Ctrl Pts',(3.22274985678079,0.000960791019879378,
10.5578332826841));
#12976=CARTESIAN_POINT('Ctrl Pts',(3.22284502429836,-0.318256496901387,
10.5386519256575));
#12977=CARTESIAN_POINT('Ctrl Pts',(3.17551406438504,-0.635789600383076,
10.5216430859734));
#12978=CARTESIAN_POINT('Ctrl Pts',(3.05570701839362,-1.02811652446106,10.4982774444553));
#12979=CARTESIAN_POINT('Ctrl Pts',(3.02551755449615,-1.11382701694309,10.4930317249368));
#12980=CARTESIAN_POINT('Ctrl Pts',(2.97107126515853,-1.24977873948251,10.4843939002583));
#12981=CARTESIAN_POINT('Ctrl Pts',(2.9490600558191,-1.30086724348337,10.4810733252899));
#12982=CARTESIAN_POINT('Ctrl Pts',(2.91855856288254,-1.36690405717254,10.4766713579713));
#12983=CARTESIAN_POINT('Ctrl Pts',(2.91125456898652,-1.3823919861739,10.4756309119887));
#12984=CARTESIAN_POINT('Ctrl Pts',(2.89912586957821,-1.40758810111851,10.4739248117993));
#12985=CARTESIAN_POINT('Ctrl Pts',(2.89437493416836,-1.41733157940731,10.4732617333196));
#12986=CARTESIAN_POINT('Ctrl Pts',(2.88510844896831,-1.43609489433333,10.4719783143048));
#12987=CARTESIAN_POINT('Ctrl Pts',(2.88059952588633,-1.44511787602599,10.4713582119254));
#12988=CARTESIAN_POINT('Ctrl Pts',(2.87012639595589,-1.46583228702481,10.469927796404));
#12989=CARTESIAN_POINT('Ctrl Pts',(2.86413300943782,-1.47750868643941,10.4691164610791));
#12990=CARTESIAN_POINT('Ctrl Pts',(2.84790056561683,-1.50866303546962,10.4669380262231));
#12991=CARTESIAN_POINT('Ctrl Pts',(2.83753319786989,-1.52807300166756,10.4655663950886));
#12992=CARTESIAN_POINT('Ctrl Pts',(2.71837612220439,-1.74576636720364,10.450016847512));
#12993=CARTESIAN_POINT('Ctrl Pts',(2.58922376708028,-1.93213677343821,10.4350730546845));
#12994=CARTESIAN_POINT('Ctrl Pts',(2.2967124191642,-2.2716845654297,10.404820104905));
#12995=CARTESIAN_POINT('Ctrl Pts',(2.13475092148466,-2.42451849944251,10.3896152615607));
#12996=CARTESIAN_POINT('Ctrl Pts',(1.94241045328373,-2.57168466886247,10.3740445904836));
#12997=CARTESIAN_POINT('Ctrl Pts',(1.92635619951598,-2.58373223118786,10.3727624020859));
#12998=CARTESIAN_POINT('Ctrl Pts',(1.90164392252171,-2.60191862765083,10.3708165530086));
#12999=CARTESIAN_POINT('Ctrl Pts',(1.89306669790262,-2.60816576111351,10.370146232016));
#13000=CARTESIAN_POINT('Ctrl Pts',(1.87889627222094,-2.61837991436293,10.3690472933864));
#13001=CARTESIAN_POINT('Ctrl Pts',(1.87332106323312,-2.62237159338074,10.3686170750685));
#13002=CARTESIAN_POINT('Ctrl Pts',(1.86252550120425,-2.63004888815279,10.3677882293625));
#13003=CARTESIAN_POINT('Ctrl Pts',(1.85730684770323,-2.63373682661498,10.36738944668));
#13004=CARTESIAN_POINT('Ctrl Pts',(1.85206003720534,-2.63742131285979,10.3669904307397));
#13005=CARTESIAN_POINT('Ctrl Pts',(1.85204286822498,-2.63743336924312,10.3669891250724));
#13006=CARTESIAN_POINT('Ctrl Pts',(1.85200827980509,-2.63745765738266,10.3669864947322));
#13007=CARTESIAN_POINT('Ctrl Pts',(1.85199086037716,-2.63746988912339,10.3669851700609));
#13008=CARTESIAN_POINT('Ctrl Pts',(1.85195576586537,-2.63749453160466,10.3669825013194));
#13009=CARTESIAN_POINT('Ctrl Pts',(1.85193809086189,-2.63750694228114,10.366981157256));
#13010=CARTESIAN_POINT('Ctrl Pts',(1.85190247998262,-2.63753194627374,10.3669784493354));
#13011=CARTESIAN_POINT('Ctrl Pts',(1.85188454410604,-2.6375445395825,10.3669770854789));
#13012=CARTESIAN_POINT('Ctrl Pts',(1.85184840617116,-2.63756991254374,10.3669743375705));
#13013=CARTESIAN_POINT('Ctrl Pts',(1.85183020402882,-2.63758269224706,10.3669729535129));
#13014=CARTESIAN_POINT('Ctrl Pts',(1.85179352799323,-2.63760844188289,10.3669701647807));
#13015=CARTESIAN_POINT('Ctrl Pts',(1.8517750540992,-2.63762141180751,10.3669687601068));
#13016=CARTESIAN_POINT('Ctrl Pts',(1.85173782884695,-2.63764754587153,10.3669659297099));
#13017=CARTESIAN_POINT('Ctrl Pts',(1.85171907747196,-2.63766071001395,10.3669645039863));
#13018=CARTESIAN_POINT('Ctrl Pts',(1.85168129136368,-2.63768723662504,10.366961631044));
#13019=CARTESIAN_POINT('Ctrl Pts',(1.85166225667835,-2.63770059905095,10.3669601838296));
#13020=CARTESIAN_POINT('Ctrl Pts',(1.8516238979749,-2.63772752639571,10.3669572674537));
#13021=CARTESIAN_POINT('Ctrl Pts',(1.85160457390084,-2.63774109134443,10.3669557982888));
#13022=CARTESIAN_POINT('Ctrl Pts',(1.8515656301836,-2.63776842808412,10.3669528375399));
#13023=CARTESIAN_POINT('Ctrl Pts',(1.85154601060022,-2.63778219982337,10.3669513459613));
#13024=CARTESIAN_POINT('Ctrl Pts',(1.84708169753427,-2.64091579830804,10.3666119527316));
#13025=CARTESIAN_POINT('Ctrl Pts',(1.84262918598116,-2.6440243445692,10.3662748410378));
#13026=CARTESIAN_POINT('Ctrl Pts',(1.83234061762384,-2.651168755314,10.3654990284983));
#13027=CARTESIAN_POINT('Ctrl Pts',(1.82649908532334,-2.65519660321681,10.3650608770086));
#13028=CARTESIAN_POINT('Ctrl Pts',(1.80907676353054,-2.66712492301295,10.3637608614477));
#13029=CARTESIAN_POINT('Ctrl Pts',(1.79745749822692,-2.6749692801828,10.36290271458));
#13030=CARTESIAN_POINT('Ctrl Pts',(1.70709950446866,-2.73511684668989,10.3562944840935));
#13031=CARTESIAN_POINT('Ctrl Pts',(1.62613711227536,-2.78401412150131,10.350754166926));
#13032=CARTESIAN_POINT('Ctrl Pts',(1.33166788885473,-2.94462200004839,10.3314930094696));
#13033=CARTESIAN_POINT('Ctrl Pts',(1.10793218277272,-3.03589138369954,10.3183916060861));
#13034=CARTESIAN_POINT('Ctrl Pts',(0.788119084471142,-3.12623497886247,
10.2994675069156));
#13035=CARTESIAN_POINT('Ctrl Pts',(0.699121278738718,-3.14733289752156,
10.2941890526453));
#13036=CARTESIAN_POINT('Ctrl Pts',(0.554478384177032,-3.17518408874531,
10.2855022530201));
#13037=CARTESIAN_POINT('Ctrl Pts',(0.499342319239361,-3.18432048547578,
10.2821665051944));
#13038=CARTESIAN_POINT('Ctrl Pts',(0.427010102499228,-3.19438165247303,
10.2777472344394));
#13039=CARTESIAN_POINT('Ctrl Pts',(0.410002874366996,-3.19660904625651,
10.276705068272));
#13040=CARTESIAN_POINT('Ctrl Pts',(0.38221346511501,-3.20002313648449,10.2749968578659));
#13041=CARTESIAN_POINT('Ctrl Pts',(0.371441500054232,-3.20129136668941,
10.2743334017013));
#13042=CARTESIAN_POINT('Ctrl Pts',(0.350642214861469,-3.2036337647008,10.2730497517792));
#13043=CARTESIAN_POINT('Ctrl Pts',(0.340615838712425,-3.20471529279946,
10.2724297988624));
#13044=CARTESIAN_POINT('Ctrl Pts',(0.317543671443908,-3.20709455031482,
10.2710004465885));
#13045=CARTESIAN_POINT('Ctrl Pts',(0.304494774535512,-3.20835976194212,
10.2701900299765));
#13046=CARTESIAN_POINT('Ctrl Pts',(0.269573840309987,-3.21153071290395,
10.26801566431));
#13047=CARTESIAN_POINT('Ctrl Pts',(0.247689740222265,-3.21329259940096,
10.2666472101627));
#13048=CARTESIAN_POINT('Ctrl Pts',(0.059988465600142,-3.22647557303819,
10.254858011993));
#13049=CARTESIAN_POINT('Ctrl Pts',(-0.106438700738981,-3.22527498780651,
10.2440383384694));
#13050=CARTESIAN_POINT('Ctrl Pts',(-0.531338313986339,-3.18928379415443,
10.2155797395566));
#13051=CARTESIAN_POINT('Ctrl Pts',(-0.787039498767731,-3.1359874064069,
10.1975971022901));
#13052=CARTESIAN_POINT('Ctrl Pts',(-1.07954729539195,-3.03694815678367,
10.1774853033915));
#13053=CARTESIAN_POINT('Ctrl Pts',(-1.1251955315476,-3.02033310938187,10.1743639042678));
#13054=CARTESIAN_POINT('Ctrl Pts',(-1.18085402766399,-2.99863734623587,
10.1705941498794));
#13055=CARTESIAN_POINT('Ctrl Pts',(-1.19123357578031,-2.99452913585048,
10.1698927107355));
#13056=CARTESIAN_POINT('Ctrl Pts',(-1.20752540810535,-2.98798273829578,
10.1687944355655));
#13057=CARTESIAN_POINT('Ctrl Pts',(-1.21345202120171,-2.98558078931128,
10.1683954736367));
#13058=CARTESIAN_POINT('Ctrl Pts',(-1.22455360523872,-2.98104300057448,
10.1676492657864));
#13059=CARTESIAN_POINT('Ctrl Pts',(-1.22973009961706,-2.97891134242453,
10.1673017846651));
#13060=CARTESIAN_POINT('Ctrl Pts',(-1.24159083835303,-2.9739909560196,10.1665066461189));
#13061=CARTESIAN_POINT('Ctrl Pts',(-1.24827124460703,-2.97119318097447,
10.1660595444378));
#13062=CARTESIAN_POINT('Ctrl Pts',(-1.2657887305887,-2.96378729431802,10.1648889738636));
#13063=CARTESIAN_POINT('Ctrl Pts',(-1.27661019941558,-2.95914221440038,
10.1641676937968));
#13064=CARTESIAN_POINT('Ctrl Pts',(-1.35040293112984,-2.92698678512689,
10.1592602260017));
#13065=CARTESIAN_POINT('Ctrl Pts',(-1.41251083056509,-2.89752556693551,
10.1551847600551));
#13066=CARTESIAN_POINT('Ctrl Pts',(-1.47417450518162,-2.86582055618364,
10.1511479553663));
#13067=CARTESIAN_POINT('Ctrl Pts',(-1.47471499453864,-2.86554246467336,
10.1511125730562));
#13068=CARTESIAN_POINT('Ctrl Pts',(-1.47525540501219,-2.86526422036124,
10.1510771966379));
#13069=CARTESIAN_POINT('',(3.219554665156,0.0024747518059529,10.314228031951));
#13070=CARTESIAN_POINT('Ctrl Pts',(-1.47525538675478,-2.86526422976154,
9.90456889022841));
#13071=CARTESIAN_POINT('Ctrl Pts',(-1.42608413530922,-2.89058132017682,
9.9081553061229));
#13072=CARTESIAN_POINT('Ctrl Pts',(-1.3762662959304,-2.91463002933362,9.91178081147647));
#13073=CARTESIAN_POINT('Ctrl Pts',(-1.10064096532606,-3.03903929931898,
9.93178094839435));
#13074=CARTESIAN_POINT('Ctrl Pts',(-0.864512675695613,-3.11444578920707,
9.9487879064623));
#13075=CARTESIAN_POINT('Ctrl Pts',(-0.535068846551581,-3.17925885939,9.97109842536471));
#13076=CARTESIAN_POINT('Ctrl Pts',(-0.447356568786386,-3.19278260631622,
9.97689759602164));
#13077=CARTESIAN_POINT('Ctrl Pts',(-0.345464231859352,-3.20421016714256,
9.98339114517325));
#13078=CARTESIAN_POINT('Ctrl Pts',(-0.331728354010996,-3.20566134299046,
9.98426143367154));
#13079=CARTESIAN_POINT('Ctrl Pts',(-0.310967743538574,-3.20771980176948,
9.9855686826844));
#13080=CARTESIAN_POINT('Ctrl Pts',(-0.303949859257804,-3.20839239331602,
9.98600918378697));
#13081=CARTESIAN_POINT('Ctrl Pts',(-0.291374193910605,-3.20955600823922,
9.98679596302675));
#13082=CARTESIAN_POINT('Ctrl Pts',(-0.285817315268795,-3.21005563109679,
9.9871427174924));
#13083=CARTESIAN_POINT('Ctrl Pts',(-0.273761364423272,-3.21110803605871,
9.98789305152055));
#13084=CARTESIAN_POINT('Ctrl Pts',(-0.267261922870133,-3.21165551861589,
9.9882963301175));
#13085=CARTESIAN_POINT('Ctrl Pts',(-0.249048001287875,-3.21313410071747,
9.98942313393491));
#13086=CARTESIAN_POINT('Ctrl Pts',(-0.237329883312136,-3.21402087618217,
9.99014420971895));
#13087=CARTESIAN_POINT('Ctrl Pts',(-0.168074167435059,-3.2188810106791,
9.99438442331592));
#13088=CARTESIAN_POINT('Ctrl Pts',(-0.110439159877188,-3.22137362544372,
9.99782579394302));
#13089=CARTESIAN_POINT('Ctrl Pts',(0.200148389134544,-3.22645938590669,
10.0160489870111));
#13090=CARTESIAN_POINT('Ctrl Pts',(0.452691870845346,-3.20081178328196,
10.029778169041));
#13091=CARTESIAN_POINT('Ctrl Pts',(0.859077090697755,-3.11043021258567,
10.0532963674504));
#13092=CARTESIAN_POINT('Ctrl Pts',(1.0155513856581,-3.06291276088429,10.0627086543546));
#13093=CARTESIAN_POINT('Ctrl Pts',(1.18819183158754,-2.99579693215432,10.0738491812351));
#13094=CARTESIAN_POINT('Ctrl Pts',(1.20856218172659,-2.98763727781313,10.0751757454327));
#13095=CARTESIAN_POINT('Ctrl Pts',(1.24096173859374,-2.97427356764129,10.077305723501));
#13096=CARTESIAN_POINT('Ctrl Pts',(1.25304550623379,-2.96920296429354,10.0781046153966));
#13097=CARTESIAN_POINT('Ctrl Pts',(1.27436955453815,-2.96010159032109,10.0795225223718));
#13098=CARTESIAN_POINT('Ctrl Pts',(1.28362253157654,-2.95610087434726,10.0801405045478));
#13099=CARTESIAN_POINT('Ctrl Pts',(1.29307358353671,-2.95196177587413,10.0807745401857));
#13100=CARTESIAN_POINT('Ctrl Pts',(1.29329065361507,-2.95186668126035,10.0807891041314));
#13101=CARTESIAN_POINT('Ctrl Pts',(1.29369497105309,-2.95168950368619,10.0808162339662));
#13102=CARTESIAN_POINT('Ctrl Pts',(1.29388222044804,-2.95160742713306,10.0808287996007));
#13103=CARTESIAN_POINT('Ctrl Pts',(1.29423101296137,-2.95145450222513,10.0808522079338));
#13104=CARTESIAN_POINT('Ctrl Pts',(1.29439255882738,-2.95138365809453,10.080863050526));
#13105=CARTESIAN_POINT('Ctrl Pts',(1.29469349286324,-2.95125165738314,10.0808832501146));
#13106=CARTESIAN_POINT('Ctrl Pts',(1.2948328836109,-2.95119050371,10.0808926070677));
#13107=CARTESIAN_POINT('Ctrl Pts',(1.295092563856,-2.95107655454774,10.0809100399306));
#13108=CARTESIAN_POINT('Ctrl Pts',(1.29521285590914,-2.95102376094181,10.0809181158509));
#13109=CARTESIAN_POINT('Ctrl Pts',(1.29543697084459,-2.95092538535371,10.0809331628941));
#13110=CARTESIAN_POINT('Ctrl Pts',(1.295540796335,-2.95087980446283,10.0809401340724));
#13111=CARTESIAN_POINT('Ctrl Pts',(1.29573424476606,-2.95079486562865,10.0809531234767));
#13112=CARTESIAN_POINT('Ctrl Pts',(1.29582387043132,-2.95075550815367,10.0809591417965));
#13113=CARTESIAN_POINT('Ctrl Pts',(1.2960220916993,-2.95066845212975,10.0809724528357));
#13114=CARTESIAN_POINT('Ctrl Pts',(1.29613068892749,-2.95062075058619,10.0809797457865));
#13115=CARTESIAN_POINT('Ctrl Pts',(1.29634431710112,-2.95052689992457,10.0809940929456));
#13116=CARTESIAN_POINT('Ctrl Pts',(1.2964493422163,-2.95048075383071,10.0810011467376));
#13117=CARTESIAN_POINT('Ctrl Pts',(1.29665594485246,-2.95038996329112,10.0810150234768));
#13118=CARTESIAN_POINT('Ctrl Pts',(1.29675752329404,-2.95034531887204,10.0810218464629));
#13119=CARTESIAN_POINT('Ctrl Pts',(1.29695735535531,-2.95025747900218,10.0810352697684));
#13120=CARTESIAN_POINT('Ctrl Pts',(1.29705560995379,-2.9502142835234,10.081041870132));
#13121=CARTESIAN_POINT('Ctrl Pts',(1.29724891233806,-2.9501292908477,10.0810548560562));
#13122=CARTESIAN_POINT('Ctrl Pts',(1.29734396121599,-2.95008749354587,10.08106124167));
#13123=CARTESIAN_POINT('Ctrl Pts',(1.29753096570892,-2.95000524840497,10.0810738056633));
#13124=CARTESIAN_POINT('Ctrl Pts',(1.29762292249541,-2.94996480040091,10.0810799841027));
#13125=CARTESIAN_POINT('Ctrl Pts',(1.29780385200112,-2.94988520686447,10.0810921410283));
#13126=CARTESIAN_POINT('Ctrl Pts',(1.29789282598168,-2.94984606110413,10.0810981195817));
#13127=CARTESIAN_POINT('Ctrl Pts',(1.29806789489787,-2.9497690268191,10.08110988374));
#13128=CARTESIAN_POINT('Ctrl Pts',(1.29815399118848,-2.94973113800339,10.0811156694197));
#13129=CARTESIAN_POINT('Ctrl Pts',(1.29832340568559,-2.94965657408345,10.0811270545666));
#13130=CARTESIAN_POINT('Ctrl Pts',(1.29840672536958,-2.94961989861393,10.0811326541179));
#13131=CARTESIAN_POINT('Ctrl Pts',(1.29857068377375,-2.94954771948243,10.0811436734897));
#13132=CARTESIAN_POINT('Ctrl Pts',(1.2986513240798,-2.94951221538847,10.0811490934026));
#13133=CARTESIAN_POINT('Ctrl Pts',(1.29881001711054,-2.94944233868442,10.0811597597315));
#13134=CARTESIAN_POINT('Ctrl Pts',(1.29888807154065,-2.94940796557202,10.0811650062488));
#13135=CARTESIAN_POINT('Ctrl Pts',(1.29904167570169,-2.94934031507084,10.0811753313181));
#13136=CARTESIAN_POINT('Ctrl Pts',(1.29911722722685,-2.94930703712607,10.0811804099778));
#13137=CARTESIAN_POINT('Ctrl Pts',(1.29926594634109,-2.94924152445466,10.0811904074134));
#13138=CARTESIAN_POINT('Ctrl Pts',(1.29933909480496,-2.94920929837146,10.0811953248916));
#13139=CARTESIAN_POINT('Ctrl Pts',(1.29948306548533,-2.94914586465413,10.0812050038071));
#13140=CARTESIAN_POINT('Ctrl Pts',(1.29955388775872,-2.94911465719814,10.0812097652373));
#13141=CARTESIAN_POINT('Ctrl Pts',(1.29969328609028,-2.9490532260724,10.0812191374052));
#13142=CARTESIAN_POINT('Ctrl Pts',(1.29976186223343,-2.94902300255519,10.0812237481384));
#13143=CARTESIAN_POINT('Ctrl Pts',(1.29989684539823,-2.94896350589331,10.0812328240652));
#13144=CARTESIAN_POINT('Ctrl Pts',(1.29996325247529,-2.94893423290189,10.0812372892531));
#13145=CARTESIAN_POINT('Ctrl Pts',(1.31053599315781,-2.94427322257542,10.0819482194315));
#13146=CARTESIAN_POINT('Ctrl Pts',(1.32101738898217,-2.93958542163187,10.0826566095034));
#13147=CARTESIAN_POINT('Ctrl Pts',(1.34997829329839,-2.92644649388387,10.0846240648758));
#13148=CARTESIAN_POINT('Ctrl Pts',(1.36840301698019,-2.91787656122391,10.085887219836));
#13149=CARTESIAN_POINT('Ctrl Pts',(1.40932447906762,-2.89836984359615,10.0887188398179));
#13150=CARTESIAN_POINT('Ctrl Pts',(1.43177722100558,-2.88734431097182,10.0902903304164));
#13151=CARTESIAN_POINT('Ctrl Pts',(1.50089422166295,-2.85239963193541,10.0951842238588));
#13152=CARTESIAN_POINT('Ctrl Pts',(1.5471028852963,-2.82760309787463,10.0985366401983));
#13153=CARTESIAN_POINT('Ctrl Pts',(1.72753088496866,-2.72503477481736,10.1119515561755));
#13154=CARTESIAN_POINT('Ctrl Pts',(1.85665243310276,-2.63875145970691,10.1222935253476));
#13155=CARTESIAN_POINT('Ctrl Pts',(2.16011968383358,-2.4026312121583,10.1482487848494));
#13156=CARTESIAN_POINT('Ctrl Pts',(2.3256406485633,-2.24280275427979,10.1639655827974));
#13157=CARTESIAN_POINT('Ctrl Pts',(2.48806062547722,-2.04847230483622,10.1801720922222));
#13158=CARTESIAN_POINT('Ctrl Pts',(2.50312727316403,-2.0300340865497,10.18168352622));
#13159=CARTESIAN_POINT('Ctrl Pts',(2.52357143491082,-2.00444126482277,10.1837436631921));
#13160=CARTESIAN_POINT('Ctrl Pts',(2.52912512833821,-1.99742926306286,10.1843042646309));
#13161=CARTESIAN_POINT('Ctrl Pts',(2.53793182538466,-1.98621445334932,10.1851946475874));
#13162=CARTESIAN_POINT('Ctrl Pts',(2.54120370230815,-1.98202662680045,10.1855257592558));
#13163=CARTESIAN_POINT('Ctrl Pts',(2.54796579259157,-1.97332724534269,10.1862106997462));
#13164=CARTESIAN_POINT('Ctrl Pts',(2.55145439373001,-1.96881450995197,10.1865644059782));
#13165=CARTESIAN_POINT('Ctrl Pts',(2.55978618690903,-1.95797744943358,10.1874100381803));
#13166=CARTESIAN_POINT('Ctrl Pts',(2.5646179885906,-1.95164433003633,10.1879011594503));
#13167=CARTESIAN_POINT('Ctrl Pts',(2.58106097379721,-1.92992573399434,10.1895752034502));
#13168=CARTESIAN_POINT('Ctrl Pts',(2.59255785367073,-1.9144536835358,10.190750371415));
#13169=CARTESIAN_POINT('Ctrl Pts',(2.65717830536732,-1.82584024347576,10.1973884656028));
#13170=CARTESIAN_POINT('Ctrl Pts',(2.70734958682327,-1.75058573944091,10.2026711360758));
#13171=CARTESIAN_POINT('Ctrl Pts',(2.87096015946836,-1.4812809114951,10.2207385517243));
#13172=CARTESIAN_POINT('Ctrl Pts',(2.967227057881,-1.27756751748756,10.2330013144909));
#13173=CARTESIAN_POINT('Ctrl Pts',(3.0626547173377,-1.0051614243851,10.2493761674999));
#13174=CARTESIAN_POINT('Ctrl Pts',(3.08198754169092,-0.944222232435921,
10.2530344534341));
#13175=CARTESIAN_POINT('Ctrl Pts',(3.12384792697356,-0.79724294937789,10.2618960329593));
#13176=CARTESIAN_POINT('Ctrl Pts',(3.14465021461784,-0.710770771948116,
10.2671409765452));
#13177=CARTESIAN_POINT('Ctrl Pts',(3.16550237738691,-0.605035981498551,
10.2736405024501));
#13178=CARTESIAN_POINT('Ctrl Pts',(3.1689916486619,-0.58648593119685,10.2747838858624));
#13179=CARTESIAN_POINT('Ctrl Pts',(3.17448854200507,-0.555780367741568,
10.2766820884816));
#13180=CARTESIAN_POINT('Ctrl Pts',(3.17658980230377,-0.54364192420868,10.2774339163744));
#13181=CARTESIAN_POINT('Ctrl Pts',(3.18026428772516,-0.521666426952067,
10.2787977427621));
#13182=CARTESIAN_POINT('Ctrl Pts',(3.18186160126185,-0.511833515568684,
10.2794089653726));
#13183=CARTESIAN_POINT('Ctrl Pts',(3.18487368151964,-0.492732277424092,
10.2805982778261));
#13184=CARTESIAN_POINT('Ctrl Pts',(3.18629364442625,-0.483464862181792,
10.2811761955267));
#13185=CARTESIAN_POINT('Ctrl Pts',(3.18931846284915,-0.463131023994156,
10.2824462302536));
#13186=CARTESIAN_POINT('Ctrl Pts',(3.19090619623556,-0.452062213202765,
10.2831388841888));
#13187=CARTESIAN_POINT('Ctrl Pts',(3.19466754877879,-0.424832567341122,
10.2848461302208));
#13188=CARTESIAN_POINT('Ctrl Pts',(3.19677616163418,-0.408663203765155,
10.2858627665606));
#13189=CARTESIAN_POINT('Ctrl Pts',(3.21484596686634,-0.26139153043618,10.2951490927864));
#13190=CARTESIAN_POINT('Ctrl Pts',(3.22285444874402,-0.129459657241155,
10.303668699674));
#13191=CARTESIAN_POINT('Ctrl Pts',(3.22274897165249,0.002574531576424,10.3123883511433));
#13192=CARTESIAN_POINT('Ctrl Pts',(3.219554665156,0.0024747518059529,10.314228031951));
#13193=CARTESIAN_POINT('Ctrl Pts',(3.22212746863257,0.36848297700967,10.3367720053601));
#13194=CARTESIAN_POINT('Ctrl Pts',(2.99522905709534,1.80797061601092,10.4256269582238));
#13195=CARTESIAN_POINT('Ctrl Pts',(0.872388983325508,3.71103042484282,10.5807928905419));
#13196=CARTESIAN_POINT('Ctrl Pts',(-2.65122281047819,2.7393115444244,10.7797258289053));
#13197=CARTESIAN_POINT('Ctrl Pts',(-3.70009722952212,-0.630335825586912,
10.9717996371069));
#13198=CARTESIAN_POINT('Ctrl Pts',(-2.32704138798567,-2.42295171699722,
11.0975624658541));
#13199=CARTESIAN_POINT('Ctrl Pts',(-1.47708659324034,-2.8687591534968,11.1570143151468));
#13200=CARTESIAN_POINT('Origin',(0.,0.,4.68922655072688));
#13201=CARTESIAN_POINT('',(-1.47525540501257,-2.86526422036105,12.6567692800014));
#13202=CARTESIAN_POINT('',(-1.47525514217501,-2.86526435568975,12.4082778759135));
#13203=CARTESIAN_POINT('',(-1.47525540501186,-2.86526422036142,4.68922655072688));
#13204=CARTESIAN_POINT('Ctrl Pts',(-1.47525540501245,-2.86526422036111,
12.6567692800014));
#13205=CARTESIAN_POINT('Ctrl Pts',(-1.47619473560958,-2.86478058170375,
12.6567037974063));
#13206=CARTESIAN_POINT('Ctrl Pts',(-1.47713382808388,-2.86429648128078,
12.6566382984126));
#13207=CARTESIAN_POINT('Ctrl Pts',(-1.4975799459372,-2.85374381612472,12.6552115211502));
#13208=CARTESIAN_POINT('Ctrl Pts',(-1.51698342780398,-2.84347686886961,
12.6538432292352));
#13209=CARTESIAN_POINT('Ctrl Pts',(-1.68039354959082,-2.75486317396149,
12.6421964820092));
#13210=CARTESIAN_POINT('Ctrl Pts',(-1.81831116618325,-2.66584384159589,
12.6315304384339));
#13211=CARTESIAN_POINT('Ctrl Pts',(-2.1515527384478,-2.41282365798401,12.6036225825653));
#13212=CARTESIAN_POINT('Ctrl Pts',(-2.33530593020492,-2.23545044242906,
12.5860524973474));
#13213=CARTESIAN_POINT('Ctrl Pts',(-2.53151275203996,-1.99516025806213,
12.5657648530545));
#13214=CARTESIAN_POINT('Ctrl Pts',(-2.56562630930633,-1.951098100943,12.5621731041873));
#13215=CARTESIAN_POINT('Ctrl Pts',(-2.6054651856129,-1.89678784670337,12.5579198844388));
#13216=CARTESIAN_POINT('Ctrl Pts',(-2.61229707577267,-1.88736773483683,
12.5571883220117));
#13217=CARTESIAN_POINT('Ctrl Pts',(-2.62286474518232,-1.87262925435896,
12.5560535643887));
#13218=CARTESIAN_POINT('Ctrl Pts',(-2.62663563143923,-1.86733635353298,
12.5556480078588));
#13219=CARTESIAN_POINT('Ctrl Pts',(-2.63361678649892,-1.85747445866487,
12.5548960529092));
#13220=CARTESIAN_POINT('Ctrl Pts',(-2.63683115968704,-1.85290857268435,
12.5545493794605));
#13221=CARTESIAN_POINT('Ctrl Pts',(-2.64409878612255,-1.842527994079,12.5537645176564));
#13222=CARTESIAN_POINT('Ctrl Pts',(-2.64814472457018,-1.83670828378848,
12.5533268314023));
#13223=CARTESIAN_POINT('Ctrl Pts',(-2.66011531209191,-1.8193679152882,12.5520294757472));
#13224=CARTESIAN_POINT('Ctrl Pts',(-2.66798433904022,-1.80780880290746,
12.5511735010759));
#13225=CARTESIAN_POINT('Ctrl Pts',(-2.72795358574787,-1.71847325060117,
12.5446227544761));
#13226=CARTESIAN_POINT('Ctrl Pts',(-2.77672318446368,-1.63850327925736,
12.5391336918004));
#13227=CARTESIAN_POINT('Ctrl Pts',(-2.9382653934292,-1.34562900287555,12.5199186546022));
#13228=CARTESIAN_POINT('Ctrl Pts',(-3.03058341738554,-1.12236245184774,
12.5068195674281));
#13229=CARTESIAN_POINT('Ctrl Pts',(-3.12262260647631,-0.802387216530855,
12.4878659580322));
#13230=CARTESIAN_POINT('Ctrl Pts',(-3.1442718616317,-0.712846203559643,
12.4825512437766));
#13231=CARTESIAN_POINT('Ctrl Pts',(-3.17290627152424,-0.567395950289029,
12.4738102345405));
#13232=CARTESIAN_POINT('Ctrl Pts',(-3.18231250173899,-0.512014584879206,
12.4704577296295));
#13233=CARTESIAN_POINT('Ctrl Pts',(-3.19270011637933,-0.439407349369612,
12.46601935475));
#13234=CARTESIAN_POINT('Ctrl Pts',(-3.19499764675104,-0.422377640592802,
12.4649752972422));
#13235=CARTESIAN_POINT('Ctrl Pts',(-3.19852388336614,-0.394563461531825,
12.4632647663584));
#13236=CARTESIAN_POINT('Ctrl Pts',(-3.19983451341419,-0.383789577562793,
12.4626008946562));
#13237=CARTESIAN_POINT('Ctrl Pts',(-3.20225760785037,-0.36299507371952,
12.4613169884182));
#13238=CARTESIAN_POINT('Ctrl Pts',(-3.20337752189715,-0.352975436960663,
12.4606971976679));
#13239=CARTESIAN_POINT('Ctrl Pts',(-3.20584381149837,-0.329931015790019,
12.4592690045522));
#13240=CARTESIAN_POINT('Ctrl Pts',(-3.20715785209024,-0.316903017568776,
12.4584595903064));
#13241=CARTESIAN_POINT('Ctrl Pts',(-3.21045735552717,-0.28206513262069,
12.4562896616383));
#13242=CARTESIAN_POINT('Ctrl Pts',(-3.21229993402519,-0.260242706565,12.4549246709453));
#13243=CARTESIAN_POINT('Ctrl Pts',(-3.22601025526251,-0.0754138263689908,
12.4433131278362));
#13244=CARTESIAN_POINT('Ctrl Pts',(-3.22568281614904,0.0882338028203065,
12.432681411931));
#13245=CARTESIAN_POINT('Ctrl Pts',(-3.19320935247579,0.503698484376278,
12.4048899543915));
#13246=CARTESIAN_POINT('Ctrl Pts',(-3.14375836722508,0.753044771747766,
12.3874046746089));
#13247=CARTESIAN_POINT('Ctrl Pts',(-3.04794466935143,1.04853968504443,12.3670714471105));
#13248=CARTESIAN_POINT('Ctrl Pts',(-3.02881508240208,1.10257985535222,12.3633739565753));
#13249=CARTESIAN_POINT('Ctrl Pts',(-3.00404406329149,1.16703662579351,12.3590129911835));
#13250=CARTESIAN_POINT('Ctrl Pts',(-2.99977536298582,1.1779656199368,12.3582753006768));
#13251=CARTESIAN_POINT('Ctrl Pts',(-2.99304187570814,1.19493112747953,12.3571331322803));
#13252=CARTESIAN_POINT('Ctrl Pts',(-2.99061834716971,1.20098375198059,12.3567262438932));
#13253=CARTESIAN_POINT('Ctrl Pts',(-2.98608589129861,1.21220450754753,12.355973084361));
#13254=CARTESIAN_POINT('Ctrl Pts',(-2.98398192495134,1.21737446606616,12.3556265302511));
#13255=CARTESIAN_POINT('Ctrl Pts',(-2.9791866317673,1.22907054591091,12.3548435446411));
#13256=CARTESIAN_POINT('Ctrl Pts',(-2.97648729489427,1.23559329040738,12.354407605262));
#13257=CARTESIAN_POINT('Ctrl Pts',(-2.96842909111313,1.25488568068073,12.35312021111));
#13258=CARTESIAN_POINT('Ctrl Pts',(-2.96300924376663,1.26762990571747,12.3522723675196));
#13259=CARTESIAN_POINT('Ctrl Pts',(-2.92189854131814,1.36259319028294,12.3459712062301));
#13260=CARTESIAN_POINT('Ctrl Pts',(-2.88287017405998,1.44333433988521,12.3407063022715));
#13261=CARTESIAN_POINT('Ctrl Pts',(-2.72438795711605,1.73904303105259,12.3213950129442));
#13262=CARTESIAN_POINT('Ctrl Pts',(-2.5838362598838,1.94174269989726,12.3080392414193));
#13263=CARTESIAN_POINT('Ctrl Pts',(-2.36117702484197,2.1953005865531,12.2888250595191));
#13264=CARTESIAN_POINT('Ctrl Pts',(-2.2978584671852,2.26149202112921,12.2835391186751));
#13265=CARTESIAN_POINT('Ctrl Pts',(-2.19145583701924,2.36363453417611,12.2748411232642));
#13266=CARTESIAN_POINT('Ctrl Pts',(-2.1501005301157,2.40131506376535,12.2715019115213));
#13267=CARTESIAN_POINT('Ctrl Pts',(-2.09480720218862,2.44912122587711,12.2670786910635));
#13268=CARTESIAN_POINT('Ctrl Pts',(-2.08173780063864,2.4602397657669,12.2660361330823));
#13269=CARTESIAN_POINT('Ctrl Pts',(-2.06026213679578,2.47821612573831,12.2643274419006));
#13270=CARTESIAN_POINT('Ctrl Pts',(-2.05190882681644,2.48513689765095,12.2636638995881));
#13271=CARTESIAN_POINT('Ctrl Pts',(-2.03572324384206,2.49840951910628,12.262380196543));
#13272=CARTESIAN_POINT('Ctrl Pts',(-2.02789577634355,2.50476704850547,12.2617602772615));
#13273=CARTESIAN_POINT('Ctrl Pts',(-2.00982616691826,2.51930310397465,12.2603311655412));
#13274=CARTESIAN_POINT('Ctrl Pts',(-1.99956376451013,2.52745605192764,12.2595209569638));
#13275=CARTESIAN_POINT('Ctrl Pts',(-1.97198773956722,2.54909070658342,12.2573475126865));
#13276=CARTESIAN_POINT('Ctrl Pts',(-1.95458591469057,2.56245837800697,12.2559797778881));
#13277=CARTESIAN_POINT('Ctrl Pts',(-1.80467832633018,2.67519835414471,12.2442278728856));
#13278=CARTESIAN_POINT('Ctrl Pts',(-1.6648512892947,2.76438151077136,12.2334476854209));
#13279=CARTESIAN_POINT('Ctrl Pts',(-1.29083593980754,2.96423203106929,12.2051509434149));
#13280=CARTESIAN_POINT('Ctrl Pts',(-1.04904592999842,3.05817394012085,12.187296163694));
#13281=CARTESIAN_POINT('Ctrl Pts',(-0.749541532113809,3.13478437267555,
12.1671374364729));
#13282=CARTESIAN_POINT('Ctrl Pts',(-0.700153944727436,3.14618351464393,
12.163877541682));
#13283=CARTESIAN_POINT('Ctrl Pts',(-0.639437277930541,3.15869679714524,
12.159964678851));
#13284=CARTESIAN_POINT('Ctrl Pts',(-0.628347505382622,3.16092152862965,
12.1592538474349));
#13285=CARTESIAN_POINT('Ctrl Pts',(-0.610937743852355,3.16431887549834,
12.158144188094));
#13286=CARTESIAN_POINT('Ctrl Pts',(-0.604625696057268,3.16553102055254,
12.15774316197));
#13287=CARTESIAN_POINT('Ctrl Pts',(-0.592814117609411,3.16776265957437,
12.1569951968635));
#13288=CARTESIAN_POINT('Ctrl Pts',(-0.58731562099644,3.16878670903568,12.1566480101098));
#13289=CARTESIAN_POINT('Ctrl Pts',(-0.574740844954814,3.17109480209489,
12.1558562773945));
#13290=CARTESIAN_POINT('Ctrl Pts',(-0.567662927653378,3.17236947496112,
12.1554122695709));
#13291=CARTESIAN_POINT('Ctrl Pts',(-0.549150758582309,3.17563942019839,
12.1542550977663));
#13292=CARTESIAN_POINT('Ctrl Pts',(-0.537709771102787,3.17759665380526,
12.1535440422503));
#13293=CARTESIAN_POINT('Ctrl Pts',(-0.461739817088373,3.19017093136881,
12.1488482415702));
#13294=CARTESIAN_POINT('Ctrl Pts',(-0.396906115463345,3.19888435396724,
12.1449636675359));
#13295=CARTESIAN_POINT('Ctrl Pts',(-0.300698357953886,3.20884382804193,
12.1393211295345));
#13296=CARTESIAN_POINT('Ctrl Pts',(-0.269503260280589,3.21161428437234,
12.1375103865045));
#13297=CARTESIAN_POINT('Ctrl Pts',(0.000726964663289101,3.23164841284286,
12.1219505056869));
#13298=CARTESIAN_POINT('Ctrl Pts',(0.240963267835843,3.22265429209174,12.1089121721284));
#13299=CARTESIAN_POINT('Ctrl Pts',(0.569158991719774,3.17343251751868,12.0900211238264));
#13300=CARTESIAN_POINT('Ctrl Pts',(0.659691103190586,3.15585513074762,12.084700796398));
#13301=CARTESIAN_POINT('Ctrl Pts',(0.804012032936248,3.12135259113154,12.0759513989263));
#13302=CARTESIAN_POINT('Ctrl Pts',(0.858329324728526,3.10685492706569,12.072596304542));
#13303=CARTESIAN_POINT('Ctrl Pts',(0.928723213883803,3.08607942392808,12.0681549780869));
#13304=CARTESIAN_POINT('Ctrl Pts',(0.945169616767288,3.08108217945138,12.0671106291311));
#13305=CARTESIAN_POINT('Ctrl Pts',(0.971935010736505,3.07271503979346,12.0653997406673));
#13306=CARTESIAN_POINT('Ctrl Pts',(0.982278478991355,3.06942410983237,12.0647358049315));
#13307=CARTESIAN_POINT('Ctrl Pts',(1.00219660347124,3.06297586846961,12.0634518590359));
#13308=CARTESIAN_POINT('Ctrl Pts',(1.01177346955445,3.05982575410037,12.0628320931146));
#13309=CARTESIAN_POINT('Ctrl Pts',(1.03375217201273,3.05248184294397,12.0614040778255));
#13310=CARTESIAN_POINT('Ctrl Pts',(1.04614348650381,3.04825733037083,12.0605948174016));
#13311=CARTESIAN_POINT('Ctrl Pts',(1.07918561683694,3.03676722961454,12.0584255693009));
#13312=CARTESIAN_POINT('Ctrl Pts',(1.09978843666799,3.02936662667686,12.0570611097661));
#13313=CARTESIAN_POINT('Ctrl Pts',(1.27316639549322,2.96508689136535,12.0454763652371));
#13314=CARTESIAN_POINT('Ctrl Pts',(1.42147478806425,2.89691006061307,12.0348729697757));
#13315=CARTESIAN_POINT('Ctrl Pts',(1.78477905815851,2.69526553319872,12.0071659596091));
#13316=CARTESIAN_POINT('Ctrl Pts',(1.99040382436097,2.54719059929882,11.9897383267371));
#13317=CARTESIAN_POINT('Ctrl Pts',(2.21971949049879,2.33717282794068,11.9693720511778));
#13318=CARTESIAN_POINT('Ctrl Pts',(2.26173002654632,2.29654299902525,11.9656007074992));
#13319=CARTESIAN_POINT('Ctrl Pts',(2.31086992280861,2.24636082509433,11.9611646799951));
#13320=CARTESIAN_POINT('Ctrl Pts',(2.31907820923738,2.23788583852116,11.9604228354107));
#13321=CARTESIAN_POINT('Ctrl Pts',(2.33175981210671,2.22464748515599,11.9592756456731));
#13322=CARTESIAN_POINT('Ctrl Pts',(2.33626539486858,2.21991537250976,11.9588678564516));
#13323=CARTESIAN_POINT('Ctrl Pts',(2.34459230272368,2.21111637803907,11.9581138745836));
#13324=CARTESIAN_POINT('Ctrl Pts',(2.34841742212452,2.20705331051225,11.9577673936231));
#13325=CARTESIAN_POINT('Ctrl Pts',(2.35704450910685,2.19784173868495,11.9569856426085));
#13326=CARTESIAN_POINT('Ctrl Pts',(2.36184015894349,2.19268743601107,11.9565508580707));
#13327=CARTESIAN_POINT('Ctrl Pts',(2.37595871242727,2.17741293535599,11.9552700294249));
#13328=CARTESIAN_POINT('Ctrl Pts',(2.3852338759679,2.16724854754257,11.9544275419528));
#13329=CARTESIAN_POINT('Ctrl Pts',(2.45281227276223,2.09223194503135,11.9482787120151));
#13330=CARTESIAN_POINT('Ctrl Pts',(2.50853253827676,2.02509012289934,11.9431506280972));
#13331=CARTESIAN_POINT('Ctrl Pts',(2.71463763954851,1.75515419583803,11.9235782660041));
#13332=CARTESIAN_POINT('Ctrl Pts',(2.84371913698329,1.53723809334595,11.9098871789854));
#13333=CARTESIAN_POINT('Ctrl Pts',(2.98212971547954,1.22512832159454,11.8904224790711));
#13334=CARTESIAN_POINT('Ctrl Pts',(3.01481884032023,1.14232334457073,11.8852789515334));
#13335=CARTESIAN_POINT('Ctrl Pts',(3.0620359497016,1.00650748598984,11.8767942322024));
#13336=CARTESIAN_POINT('Ctrl Pts',(3.07870920263555,0.954290617893719,11.8735212953733));
#13337=CARTESIAN_POINT('Ctrl Pts',(3.09880782422475,0.885323530008186,11.8691736898158));
#13338=CARTESIAN_POINT('Ctrl Pts',(3.10344359717685,0.868933545257085,11.8681386927785));
#13339=CARTESIAN_POINT('Ctrl Pts',(3.11081138333749,0.842073140956572,11.8664392755297));
#13340=CARTESIAN_POINT('Ctrl Pts',(3.11362101128111,0.831624212619681,11.8657773920793));
#13341=CARTESIAN_POINT('Ctrl Pts',(3.11895001043523,0.81140020460836,11.864494691062));
#13342=CARTESIAN_POINT('Ctrl Pts',(3.12147618158367,0.801627035308575,11.8638741031005));
#13343=CARTESIAN_POINT('Ctrl Pts',(3.12719276372811,0.779074117363573,11.8624402634746));
#13344=CARTESIAN_POINT('Ctrl Pts',(3.13035080679509,0.766286421630827,11.8616259737636));
#13345=CARTESIAN_POINT('Ctrl Pts',(3.138613002571,0.731927156483886,11.859434436022));
#13346=CARTESIAN_POINT('Ctrl Pts',(3.14357305888789,0.710321987610526,11.8580525705126));
#13347=CARTESIAN_POINT('Ctrl Pts',(3.19391146281884,0.480195229483713,11.8432906800071));
#13348=CARTESIAN_POINT('Ctrl Pts',(3.21868566259682,0.267748686197534,11.8292345209011));
#13349=CARTESIAN_POINT('Ctrl Pts',(3.22261353595994,0.0353028390036726,
11.8135680300132));
#13350=CARTESIAN_POINT('Ctrl Pts',(3.2227664150345,0.0161529798790844,11.8122756787049));
#13351=CARTESIAN_POINT('Ctrl Pts',(3.22254099906837,-0.226242497291643,
11.7959007038741));
#13352=CARTESIAN_POINT('Ctrl Pts',(3.1991374061631,-0.448877816708697,11.7806320218433));
#13353=CARTESIAN_POINT('Ctrl Pts',(3.1480726137505,-0.690145486886651,11.764858078822));
#13354=CARTESIAN_POINT('Ctrl Pts',(3.14299331856508,-0.712920085269498,
11.7633773627682));
#13355=CARTESIAN_POINT('Ctrl Pts',(3.13564137771531,-0.744277809341747,
11.7613519358791));
#13356=CARTESIAN_POINT('Ctrl Pts',(3.13358010042799,-0.752909068696944,
11.7607958347463));
#13357=CARTESIAN_POINT('Ctrl Pts',(3.13023035094593,-0.766683521448196,
11.7599107255696));
#13358=CARTESIAN_POINT('Ctrl Pts',(3.12896481019171,-0.771832164136228,
11.759580415868));
#13359=CARTESIAN_POINT('Ctrl Pts',(3.12630836422833,-0.782525560207517,
11.7588955164548));
#13360=CARTESIAN_POINT('Ctrl Pts',(3.12491540876568,-0.788069748923611,
11.7585410562112));
#13361=CARTESIAN_POINT('Ctrl Pts',(3.12153118564186,-0.801389444844727,
11.7576909561421));
#13362=CARTESIAN_POINT('Ctrl Pts',(3.11952559033726,-0.809161343447773,
11.7571961423366));
#13363=CARTESIAN_POINT('Ctrl Pts',(3.11251466974097,-0.835915893804152,
11.7554966773848));
#13364=CARTESIAN_POINT('Ctrl Pts',(3.10736482867215,-0.85486070006757,11.7543001003763));
#13365=CARTESIAN_POINT('Ctrl Pts',(3.07666862674289,-0.963839308073972,
11.7474499560186));
#13366=CARTESIAN_POINT('Ctrl Pts',(3.04738083677664,-1.0527817682856,11.7419894428558));
#13367=CARTESIAN_POINT('Ctrl Pts',(2.9845001477277,-1.21899556925063,11.7318161141954));
#13368=CARTESIAN_POINT('Ctrl Pts',(2.95167120000717,-1.29646808977821,11.7270875533678));
#13369=CARTESIAN_POINT('Ctrl Pts',(2.80218367048182,-1.61403504874381,11.7074393911293));
#13370=CARTESIAN_POINT('Ctrl Pts',(2.65898297315646,-1.84041729271843,11.6926777492949));
#13371=CARTESIAN_POINT('Ctrl Pts',(2.46713354274841,-2.0737919083236,11.6746529493628));
#13372=CARTESIAN_POINT('Ctrl Pts',(2.44429777212406,-2.10065919405715,11.6725322964045));
#13373=CARTESIAN_POINT('Ctrl Pts',(2.4112476918558,-2.13827538603683,11.6694948567551));
#13374=CARTESIAN_POINT('Ctrl Pts',(2.4013924394172,-2.14933743243355,11.6685929998813));
#13375=CARTESIAN_POINT('Ctrl Pts',(2.38521729708612,-2.16724312769131,11.6671188837575));
#13376=CARTESIAN_POINT('Ctrl Pts',(2.37894331894642,-2.17412810367687,11.6665485705697));
#13377=CARTESIAN_POINT('Ctrl Pts',(2.36571586682559,-2.18851791684877,11.665349176972));
#13378=CARTESIAN_POINT('Ctrl Pts',(2.35875633798489,-2.19601702385896,11.6647198411901));
#13379=CARTESIAN_POINT('Ctrl Pts',(2.34205336716119,-2.213843984046,11.6632134260617));
#13380=CARTESIAN_POINT('Ctrl Pts',(2.33227721300811,-2.22414076704486,11.6623349393322));
#13381=CARTESIAN_POINT('Ctrl Pts',(2.29879923042876,-2.25893818223412,11.6593371834228));
#13382=CARTESIAN_POINT('Ctrl Pts',(2.27477749051116,-2.28312654872859,11.6572039594849));
#13383=CARTESIAN_POINT('Ctrl Pts',(2.13926184564403,-2.41532020771901,11.6452626633037));
#13384=CARTESIAN_POINT('Ctrl Pts',(2.02047668968535,-2.51552672605947,11.6351228598179));
#13385=CARTESIAN_POINT('Ctrl Pts',(1.75035522967044,-2.71188684810519,11.6128154184088));
#13386=CARTESIAN_POINT('Ctrl Pts',(1.59726605259747,-2.80478357669678,11.6006070194257));
#13387=CARTESIAN_POINT('Ctrl Pts',(1.41021681310188,-2.89798551556075,11.5865839363803));
#13388=CARTESIAN_POINT('Ctrl Pts',(1.38296933931043,-2.91108697683825,11.5845627609746));
#13389=CARTESIAN_POINT('Ctrl Pts',(1.2729104100378,-2.96211277361997,11.5764946069882));
#13390=CARTESIAN_POINT('Ctrl Pts',(1.18868419553505,-2.99690610548107,11.5705346805874));
#13391=CARTESIAN_POINT('Ctrl Pts',(1.09002983869993,-3.03284448870427,11.5638843011003));
#13392=CARTESIAN_POINT('Ctrl Pts',(1.07693955213573,-3.03751740066594,11.5630084620682));
#13393=CARTESIAN_POINT('Ctrl Pts',(1.05714554495973,-3.04443933146092,11.5616944506215));
#13394=CARTESIAN_POINT('Ctrl Pts',(1.05046418339184,-3.04675114636058,11.5612526852176));
#13395=CARTESIAN_POINT('Ctrl Pts',(1.03849360151569,-3.05084902385153,11.5604644386424));
#13396=CARTESIAN_POINT('Ctrl Pts',(1.03320731760689,-3.0526433409642,11.5601174745965));
#13397=CARTESIAN_POINT('Ctrl Pts',(1.02174463003235,-3.05650092039963,11.5593675799754));
#13398=CARTESIAN_POINT('Ctrl Pts',(1.01556664603151,-3.05855919587052,11.5589649457553));
#13399=CARTESIAN_POINT('Ctrl Pts',(0.998274687096857,-3.06426206659673,
11.5578421564981));
#13400=CARTESIAN_POINT('Ctrl Pts',(0.987146913883587,-3.06786494876582,
11.5571244217848));
#13401=CARTESIAN_POINT('Ctrl Pts',(0.921964360582787,-3.08857797685089,
11.5529468920375));
#13402=CARTESIAN_POINT('Ctrl Pts',(0.867481545450114,-3.10432100163293,
11.5495621983289));
#13403=CARTESIAN_POINT('Ctrl Pts',(0.567053143084973,-3.182602603636,11.5313372259335));
#13404=CARTESIAN_POINT('Ctrl Pts',(0.314778572355372,-3.2173669450883,11.5175662244789));
#13405=CARTESIAN_POINT('Ctrl Pts',(-0.102609078521045,-3.22527084468108,
11.4939847295924));
#13406=CARTESIAN_POINT('Ctrl Pts',(-0.266212305677577,-3.21590131087481,
11.4845535338796));
#13407=CARTESIAN_POINT('Ctrl Pts',(-0.450094124506783,-3.19123998684728,
11.4733945641864));
#13408=CARTESIAN_POINT('Ctrl Pts',(-0.471773684566638,-3.18810710749064,
11.4720703297883));
#13409=CARTESIAN_POINT('Ctrl Pts',(-0.506360322041596,-3.18274854156049,
11.4699432452501));
#13410=CARTESIAN_POINT('Ctrl Pts',(-0.519288928402661,-3.18066471911724,
11.4691448956423));
#13411=CARTESIAN_POINT('Ctrl Pts',(-0.542148179714665,-3.17683719540533,
11.4677274422646));
#13412=CARTESIAN_POINT('Ctrl Pts',(-0.552084072998699,-3.17512557035948,
11.4671093675229));
#13413=CARTESIAN_POINT('Ctrl Pts',(-0.572698137509648,-3.1714747654765,
11.4658228781847));
#13414=CARTESIAN_POINT('Ctrl Pts',(-0.583374858295766,-3.16952821644742,
11.4651542353869));
#13415=CARTESIAN_POINT('Ctrl Pts',(-0.610928330344991,-3.16436080979207,
11.4634225537547));
#13416=CARTESIAN_POINT('Ctrl Pts',(-0.627789354657151,-3.16105888384223,
11.4623569345819));
#13417=CARTESIAN_POINT('Ctrl Pts',(-0.699631712380283,-3.14639239597509,
11.4577905759502));
#13418=CARTESIAN_POINT('Ctrl Pts',(-0.754334652233257,-3.13372753045579,
11.4542484334825));
#13419=CARTESIAN_POINT('Ctrl Pts',(-0.89776193465971,-3.0965481762599,11.4447821297314));
#13420=CARTESIAN_POINT('Ctrl Pts',(-0.985810180822148,-3.06965191144472,
11.4387861534985));
#13421=CARTESIAN_POINT('Ctrl Pts',(-1.21070675631613,-2.9902779126194,11.423008239846));
#13422=CARTESIAN_POINT('Ctrl Pts',(-1.34523599042925,-2.93220808941505,
11.4131044842263));
#13423=CARTESIAN_POINT('Ctrl Pts',(-1.47525557920443,-2.86526413067386,
11.4032056183244));
#13424=CARTESIAN_POINT('',(3.22749356206024,0.00107973417029931,11.5643095400564));
#13425=CARTESIAN_POINT('Ctrl Pts',(-1.47708659324034,-2.8687591534968,11.1570143151468));
#13426=CARTESIAN_POINT('Ctrl Pts',(-1.37902487374519,-2.92019323452928,
11.1638734453086));
#13427=CARTESIAN_POINT('Ctrl Pts',(-0.304424137651661,-3.4118415492434,
11.2370435549249));
#13428=CARTESIAN_POINT('Ctrl Pts',(2.16938213632706,-3.09513680703482,11.3727804995698));
#13429=CARTESIAN_POINT('Ctrl Pts',(3.22315092886655,-1.00817079531109,11.5016583140529));
#13430=CARTESIAN_POINT('Ctrl Pts',(3.22764049557943,0.00108461746384235,
11.5642251490816));
#13431=CARTESIAN_POINT('Ctrl Pts',(3.22274986808945,0.000922078856079595,
11.5670340712653));
#13432=CARTESIAN_POINT('Ctrl Pts',(3.22274249037896,0.0267078512451821,
11.5687062102123));
#13433=CARTESIAN_POINT('Ctrl Pts',(3.22242563788659,0.052493591020987,11.5703659999436));
#13434=CARTESIAN_POINT('Ctrl Pts',(3.22138428404907,0.0953564309527305,
11.5731015027928));
#13435=CARTESIAN_POINT('Ctrl Pts',(3.2208333897793,0.112436021340087,11.5741853081487));
#13436=CARTESIAN_POINT('Ctrl Pts',(3.21984681431238,0.136966150523044,11.5757321982439));
#13437=CARTESIAN_POINT('Ctrl Pts',(3.21952107635683,0.144420481582638,11.5762009870684));
#13438=CARTESIAN_POINT('Ctrl Pts',(3.21890592421196,0.157459467209442,11.5770186525729));
#13439=CARTESIAN_POINT('Ctrl Pts',(3.21862785916603,0.163044589177729,11.5773681428694));
#13440=CARTESIAN_POINT('Ctrl Pts',(3.21805643252585,0.173950438145847,11.5780490791059));
#13441=CARTESIAN_POINT('Ctrl Pts',(3.21776440807274,0.179271229269288,11.5783805987438));
#13442=CARTESIAN_POINT('Ctrl Pts',(3.21715365382935,0.189916780604091,11.579042460404));
#13443=CARTESIAN_POINT('Ctrl Pts',(3.2168349014236,0.195241475791694,11.5793728015094));
#13444=CARTESIAN_POINT('Ctrl Pts',(3.21603427612127,0.208081245841575,11.5801677160106));
#13445=CARTESIAN_POINT('Ctrl Pts',(3.21553927782859,0.215595513574288,11.5806315568701));
#13446=CARTESIAN_POINT('Ctrl Pts',(3.21361722643613,0.243292538737717,11.5823364140497));
#13447=CARTESIAN_POINT('Ctrl Pts',(3.21202642019436,0.263463966103473,11.5835685920823));
#13448=CARTESIAN_POINT('Ctrl Pts',(3.20668281311921,0.323947402387177,11.5872384421211));
#13449=CARTESIAN_POINT('Ctrl Pts',(3.20236015899617,0.36420641922359,11.5896480693079));
#13450=CARTESIAN_POINT('Ctrl Pts',(3.16096800382506,0.691482425800945,11.6090436302363));
#13451=CARTESIAN_POINT('Ctrl Pts',(3.08614843790116,0.972415922668809,11.6245891255178));
#13452=CARTESIAN_POINT('Ctrl Pts',(2.94058238012473,1.32174546642264,11.6461645806989));
#13453=CARTESIAN_POINT('Ctrl Pts',(2.90297014836683,1.40242588019415,11.6513077463558));
#13454=CARTESIAN_POINT('Ctrl Pts',(2.83687897755517,1.53011057963693,11.6597917030701));
#13455=CARTESIAN_POINT('Ctrl Pts',(2.81045184794963,1.57812565752283,11.6630642441681));
#13456=CARTESIAN_POINT('Ctrl Pts',(2.77422603063957,1.64014556145109,11.6674111758868));
#13457=CARTESIAN_POINT('Ctrl Pts',(2.76552118869172,1.65478097324236,11.6684459035223));
#13458=CARTESIAN_POINT('Ctrl Pts',(2.75109799803448,1.67859892997589,11.6701448387876));
#13459=CARTESIAN_POINT('Ctrl Pts',(2.74544860766733,1.68782300631652,11.670806510797));
#13460=CARTESIAN_POINT('Ctrl Pts',(2.73443942089812,1.70559679840141,11.6720887731784));
#13461=CARTESIAN_POINT('Ctrl Pts',(2.7290856884291,1.71415013542971,11.6727091339611));
#13462=CARTESIAN_POINT('Ctrl Pts',(2.71665398157593,1.73380565860496,11.6741424056968));
#13463=CARTESIAN_POINT('Ctrl Pts',(2.70954800068266,1.74488983639341,11.6749563536819));
#13464=CARTESIAN_POINT('Ctrl Pts',(2.69030244115566,1.77450873132731,11.677146869809));
#13465=CARTESIAN_POINT('Ctrl Pts',(2.67803948175904,1.79296206233852,11.6785280505755));
#13466=CARTESIAN_POINT('Ctrl Pts',(2.54205176089383,1.99308890073625,11.6936901921808));
#13467=CARTESIAN_POINT('Ctrl Pts',(2.4002655229634,2.16174052258144,11.7081913687182));
#13468=CARTESIAN_POINT('Ctrl Pts',(2.11062723143564,2.44234738538761,11.7353924766799));
#13469=CARTESIAN_POINT('Ctrl Pts',(1.96812630188285,2.55857203759592,11.7479303185372));
#13470=CARTESIAN_POINT('Ctrl Pts',(1.77834919370969,2.68807091224547,11.7630607501357));
#13471=CARTESIAN_POINT('Ctrl Pts',(1.7396381930857,2.71328407830959,11.7660711726151));
#13472=CARTESIAN_POINT('Ctrl Pts',(1.68407525005283,2.74779498292184,11.7702719988765));
#13473=CARTESIAN_POINT('Ctrl Pts',(1.66766313108956,2.75778651037123,11.7714983486244));
#13474=CARTESIAN_POINT('Ctrl Pts',(1.64232839598178,2.77290115470138,11.7733681375891));
#13475=CARTESIAN_POINT('Ctrl Pts',(1.63346926812361,2.77812914218243,11.7740176488681));
#13476=CARTESIAN_POINT('Ctrl Pts',(1.61878011121123,2.78670301483388,11.7750872704197));
#13477=CARTESIAN_POINT('Ctrl Pts',(1.61296445047471,2.79007319343898,11.7755088646787));
#13478=CARTESIAN_POINT('Ctrl Pts',(1.6016956348499,2.79655646868358,11.7763220703072));
#13479=CARTESIAN_POINT('Ctrl Pts',(1.59624384727609,2.79967186842773,11.7767138264377));
#13480=CARTESIAN_POINT('Ctrl Pts',(1.58612074454396,2.8054174884159,11.7774381179487));
#13481=CARTESIAN_POINT('Ctrl Pts',(1.5814520211789,2.80805195925302,11.777770920269));
#13482=CARTESIAN_POINT('Ctrl Pts',(1.57061901960535,2.81412922711128,11.7785402938721));
#13483=CARTESIAN_POINT('Ctrl Pts',(1.56444999683427,2.8175634192107,11.7789763090534));
#13484=CARTESIAN_POINT('Ctrl Pts',(1.54573176673379,2.82790311592356,11.7802930334057));
#13485=CARTESIAN_POINT('Ctrl Pts',(1.53314756161647,2.83474536770029,11.7811697914067));
#13486=CARTESIAN_POINT('Ctrl Pts',(1.43376245344371,2.88792736356153,11.788030988222));
#13487=CARTESIAN_POINT('Ctrl Pts',(1.34491702221414,2.93035859548682,11.7937881091403));
#13488=CARTESIAN_POINT('Ctrl Pts',(1.03680590172559,3.06053564091246,11.8129610100627));
#13489=CARTESIAN_POINT('Ctrl Pts',(0.809910356764825,3.12824243046199,11.8258154074241));
#13490=CARTESIAN_POINT('Ctrl Pts',(0.487227554761787,3.1870320886624,11.8444885765798));
#13491=CARTESIAN_POINT('Ctrl Pts',(0.396152940850973,3.1996289070675,11.8497934096994));
#13492=CARTESIAN_POINT('Ctrl Pts',(0.248834866693381,3.213618578218,11.8585194256859));
#13493=CARTESIAN_POINT('Ctrl Pts',(0.192874340959847,3.2174620541282,11.8618671377285));
#13494=CARTESIAN_POINT('Ctrl Pts',(0.119688718202076,3.22057246839202,11.8662998246035));
#13495=CARTESIAN_POINT('Ctrl Pts',(0.102527692945166,3.22116445836857,11.8673431157513));
#13496=CARTESIAN_POINT('Ctrl Pts',(0.0745187561960433,3.22190660911981,
11.869052554973));
#13497=CARTESIAN_POINT('Ctrl Pts',(0.0636732267531638,3.22213918981772,
11.8697161061062));
#13498=CARTESIAN_POINT('Ctrl Pts',(0.0427491398346177,3.22248222039309,
11.870999506736));
#13499=CARTESIAN_POINT('Ctrl Pts',(0.0326708192485477,3.2226001557116,11.8716191132431));
#13500=CARTESIAN_POINT('Ctrl Pts',(0.0094996513050964,3.22276259479761,
11.8730470445237));
#13501=CARTESIAN_POINT('Ctrl Pts',(-0.00359317861399371,3.22277459136332,
11.8738563815905));
#13502=CARTESIAN_POINT('Ctrl Pts',(-0.0385888829571881,3.22259340110126,
11.8760264602931));
#13503=CARTESIAN_POINT('Ctrl Pts',(-0.0604900250462614,3.22225670133831,
11.8773916810165));
#13504=CARTESIAN_POINT('Ctrl Pts',(-0.246202783867658,3.21750763303492,
11.8890306188454));
#13505=CARTESIAN_POINT('Ctrl Pts',(-0.409435950707107,3.20083093786686,
11.8996916386932));
#13506=CARTESIAN_POINT('Ctrl Pts',(-0.820554761215995,3.12686258942418,
11.9275521612582));
#13507=CARTESIAN_POINT('Ctrl Pts',(-1.06423534226815,3.05253633609439,11.9450773907194));
#13508=CARTESIAN_POINT('Ctrl Pts',(-1.34831418354115,2.9276867165127,11.9653784695869));
#13509=CARTESIAN_POINT('Ctrl Pts',(-1.39936376652582,2.90363265888656,11.9690169591603));
#13510=CARTESIAN_POINT('Ctrl Pts',(-1.46018735612178,2.87299613494754,11.9733176645033));
#13511=CARTESIAN_POINT('Ctrl Pts',(-1.47058736667286,2.86768664836898,11.9740517852065));
#13512=CARTESIAN_POINT('Ctrl Pts',(-1.48673694128351,2.85933089363235,11.9751895504171));
#13513=CARTESIAN_POINT('Ctrl Pts',(-1.49250640045858,2.85632360530528,11.9755955771843));
#13514=CARTESIAN_POINT('Ctrl Pts',(-1.50320789439459,2.85070425250725,11.9763478192089));
#13515=CARTESIAN_POINT('Ctrl Pts',(-1.50814220391267,2.84809687379613,11.9766943129702));
#13516=CARTESIAN_POINT('Ctrl Pts',(-1.51931380963264,2.84215642098321,11.9774780160625));
#13517=CARTESIAN_POINT('Ctrl Pts',(-1.52554690824573,2.83881563446275,11.9779147283269));
#13518=CARTESIAN_POINT('Ctrl Pts',(-1.54401149050716,2.82884069850565,11.9792069425469));
#13519=CARTESIAN_POINT('Ctrl Pts',(-1.55621124626149,2.82214772000768,11.9800587917559));
#13520=CARTESIAN_POINT('Ctrl Pts',(-1.64842050612833,2.77078050687666,11.9864855571273));
#13521=CARTESIAN_POINT('Ctrl Pts',(-1.72654327477322,2.72278652588155,11.9918634389635));
#13522=CARTESIAN_POINT('Ctrl Pts',(-2.00418739588655,2.53545540677384,12.0111231880685));
#13523=CARTESIAN_POINT('Ctrl Pts',(-2.18980515551159,2.37698713604192,12.0243472221739));
#13524=CARTESIAN_POINT('Ctrl Pts',(-2.41851899609109,2.13197634680636,12.0434293555514));
#13525=CARTESIAN_POINT('Ctrl Pts',(-2.47830328780289,2.0621755901511,12.0487320989932));
#13526=CARTESIAN_POINT('Ctrl Pts',(-2.5696420606219,1.9458162778558,12.0574549913814));
#13527=CARTESIAN_POINT('Ctrl Pts',(-2.60310391669494,1.90081843695513,12.0608017383624));
#13528=CARTESIAN_POINT('Ctrl Pts',(-2.64525609121311,1.8409325253953,12.0652333251167));
#13529=CARTESIAN_POINT('Ctrl Pts',(-2.65502606899793,1.8268138674625,12.0662765074791));
#13530=CARTESIAN_POINT('Ctrl Pts',(-2.67078382627517,1.80364879828592,12.0679858132374));
#13531=CARTESIAN_POINT('Ctrl Pts',(-2.67683964968382,1.79464891262382,12.0686493404749));
#13532=CARTESIAN_POINT('Ctrl Pts',(-2.68843440750514,1.77722806334803,12.069932726349));
#13533=CARTESIAN_POINT('Ctrl Pts',(-2.6939795079997,1.76881134081716,12.0705523421653));
#13534=CARTESIAN_POINT('Ctrl Pts',(-2.70663723012357,1.74940101587895,12.0719803400093));
#13535=CARTESIAN_POINT('Ctrl Pts',(-2.7137224811148,1.73838985765786,12.0727897346387));
#13536=CARTESIAN_POINT('Ctrl Pts',(-2.73248197900168,1.70884162608429,12.0749600680681));
#13537=CARTESIAN_POINT('Ctrl Pts',(-2.74403448692855,1.69022843570866,12.0763254876082));
#13538=CARTESIAN_POINT('Ctrl Pts',(-2.84047054421035,1.53125765982343,12.0879745419554));
#13539=CARTESIAN_POINT('Ctrl Pts',(-2.91470085818788,1.38474803167294,12.0986462585612));
#13540=CARTESIAN_POINT('Ctrl Pts',(-3.07473557039341,0.99837275599216,12.1265404312895));
#13541=CARTESIAN_POINT('Ctrl Pts',(-3.14388207541768,0.752826505316417,
12.1440893178192));
#13542=CARTESIAN_POINT('Ctrl Pts',(-3.19217173853121,0.446419487259036,
12.1643778785104));
#13543=CARTESIAN_POINT('Ctrl Pts',(-3.1994444548833,0.390905165253747,12.1679870563966));
#13544=CARTESIAN_POINT('Ctrl Pts',(-3.20647952486802,0.323639206522639,
12.1722578775545));
#13545=CARTESIAN_POINT('Ctrl Pts',(-3.20762850341694,0.312045947333867,
12.1729902884519));
#13546=CARTESIAN_POINT('Ctrl Pts',(-3.20932060802965,0.293974574578464,
12.1741259857712));
#13547=CARTESIAN_POINT('Ctrl Pts',(-3.20990702858604,0.287500756917704,
12.1745316407617));
#13548=CARTESIAN_POINT('Ctrl Pts',(-3.21096057573848,0.275464874375558,
12.1752835472067));
#13549=CARTESIAN_POINT('Ctrl Pts',(-3.2114328356937,0.269903424390084,12.175630074949));
#13550=CARTESIAN_POINT('Ctrl Pts',(-3.21247137274394,0.257284602528006,
12.1764143048046));
#13551=CARTESIAN_POINT('Ctrl Pts',(-3.21302884250843,0.250226591043907,
12.1768515070534));
#13552=CARTESIAN_POINT('Ctrl Pts',(-3.2146158099064,0.229254067373092,12.1781465171027));
#13553=CARTESIAN_POINT('Ctrl Pts',(-3.21557822656471,0.215334432624636,
12.1790006486707));
#13554=CARTESIAN_POINT('Ctrl Pts',(-3.22224828259434,0.108815182573246,
12.1854987241927));
#13555=CARTESIAN_POINT('Ctrl Pts',(-3.22404591461609,0.0160048392417297,
12.1909406570997));
#13556=CARTESIAN_POINT('Ctrl Pts',(-3.21607478716334,-0.318555463778213,
12.2101739790226));
#13557=CARTESIAN_POINT('Ctrl Pts',(-3.18311398985177,-0.558938893050106,
12.2233255010249));
#13558=CARTESIAN_POINT('Ctrl Pts',(-3.10091533984071,-0.882556932284656,
12.2423336450347));
#13559=CARTESIAN_POINT('Ctrl Pts',(-3.07445830211507,-0.970714632711053,
12.2476440267163));
#13560=CARTESIAN_POINT('Ctrl Pts',(-3.02584787840065,-1.1106361636464,12.2563783359346));
#13561=CARTESIAN_POINT('Ctrl Pts',(-3.00604670539333,-1.16316408942087,
12.2597286096372));
#13562=CARTESIAN_POINT('Ctrl Pts',(-2.97840865036355,-1.23105421900172,
12.2641642165881));
#13563=CARTESIAN_POINT('Ctrl Pts',(-2.97180540927946,-1.2469102494939,12.2652077963702));
#13564=CARTESIAN_POINT('Ctrl Pts',(-2.96082501647664,-1.27269418467854,
12.2669175897189));
#13565=CARTESIAN_POINT('Ctrl Pts',(-2.95652386484686,-1.28265423943773,
12.2675812042683));
#13566=CARTESIAN_POINT('Ctrl Pts',(-2.94813015614229,-1.30182476718858,
12.2688646441174));
#13567=CARTESIAN_POINT('Ctrl Pts',(-2.94404451753865,-1.31103814478786,
12.2694842259787));
#13568=CARTESIAN_POINT('Ctrl Pts',(-2.93455313430845,-1.33217372140194,
12.2709119808665));
#13569=CARTESIAN_POINT('Ctrl Pts',(-2.92911786045172,-1.34408239090049,
12.2717211653687));
#13570=CARTESIAN_POINT('Ctrl Pts',(-2.91439791287889,-1.37582039915591,
12.2738905689524));
#13571=CARTESIAN_POINT('Ctrl Pts',(-2.90498358407239,-1.3955885150647,12.2752552627428));
#13572=CARTESIAN_POINT('Ctrl Pts',(-2.82358863429697,-1.56210816238581,
12.2868674713166));
#13573=CARTESIAN_POINT('Ctrl Pts',(-2.74075219450701,-1.70326084694038,
12.2975002346816));
#13574=CARTESIAN_POINT('Ctrl Pts',(-2.5032958898301,-2.04540118072834,12.3252741370639));
#13575=CARTESIAN_POINT('Ctrl Pts',(-2.3350347729996,-2.23556790716262,12.3427393135935));
#13576=CARTESIAN_POINT('Ctrl Pts',(-2.10332622493173,-2.44242703613689,
12.3630734111069));
#13577=CARTESIAN_POINT('Ctrl Pts',(-2.05936318504076,-2.47960788865712,
12.3667874966365));
#13578=CARTESIAN_POINT('Ctrl Pts',(-2.00525695221621,-2.52293481037836,
12.3711651592417));
#13579=CARTESIAN_POINT('Ctrl Pts',(-1.99604907480359,-2.5302259983696,12.3719036131642));
#13580=CARTESIAN_POINT('Ctrl Pts',(-1.98166704757851,-2.54148692651986,
12.373046617751));
#13581=CARTESIAN_POINT('Ctrl Pts',(-1.97652047338424,-2.54549148598286,
12.373453585523));
#13582=CARTESIAN_POINT('Ctrl Pts',(-1.96694791562539,-2.5528933760697,12.3742066816674));
#13583=CARTESIAN_POINT('Ctrl Pts',(-1.9625253055307,-2.55629480268904,12.3745530941412));
#13584=CARTESIAN_POINT('Ctrl Pts',(-1.95249289569975,-2.56396934104302,
12.3753354854073));
#13585=CARTESIAN_POINT('Ctrl Pts',(-1.94687790502244,-2.56823552555741,
12.3757709741234));
#13586=CARTESIAN_POINT('Ctrl Pts',(-1.93021695415085,-2.58080822234851,
12.3770562193339));
#13587=CARTESIAN_POINT('Ctrl Pts',(-1.91913134787049,-2.58906227351373,
12.3779023812981));
#13588=CARTESIAN_POINT('Ctrl Pts',(-1.83631109790268,-2.64990383507711,
12.3841602991194));
#13589=CARTESIAN_POINT('Ctrl Pts',(-1.76247290626276,-2.69957795642286,
12.389386535945));
#13590=CARTESIAN_POINT('Ctrl Pts',(-1.61766785356306,-2.78851665839571,
12.3991714145107));
#13591=CARTESIAN_POINT('Ctrl Pts',(-1.54714526428157,-2.82824987494954,
12.4037409095));
#13592=CARTESIAN_POINT('Ctrl Pts',(-1.47525514217493,-2.86526435568979,
12.4082778759135));
#13593=CARTESIAN_POINT('Origin',(0.,0.,4.68922655072688));
#13594=CARTESIAN_POINT('',(-1.47525547426955,-2.8652641847023,13.9035519756546));
#13595=CARTESIAN_POINT('',(-1.4752554049854,-2.86526422037504,13.6541509617524));
#13596=CARTESIAN_POINT('',(-1.47525540501186,-2.86526422036142,4.68922655072688));
#13597=CARTESIAN_POINT('',(3.22274998502511,0.000310677704944338,13.0638091501483));
#13598=CARTESIAN_POINT('Ctrl Pts',(-1.47525547426939,-2.86526418470238,
13.9035519756546));
#13599=CARTESIAN_POINT('Ctrl Pts',(-1.54303258806227,-2.83036738227594,
13.8992923598215));
#13600=CARTESIAN_POINT('Ctrl Pts',(-1.60960295797985,-2.79304953613835,
13.8950259309918));
#13601=CARTESIAN_POINT('Ctrl Pts',(-1.81607017557258,-2.6674584409174,13.8813804824954));
#13602=CARTESIAN_POINT('Ctrl Pts',(-1.95046699540141,-2.57081957006326,
13.8718588107835));
#13603=CARTESIAN_POINT('Ctrl Pts',(-2.09362411535334,-2.45017078621481,
13.8605985964914));
#13604=CARTESIAN_POINT('Ctrl Pts',(-2.11025375650396,-2.43586285835686,
13.859272399019));
#13605=CARTESIAN_POINT('Ctrl Pts',(-2.13658212788618,-2.41273830262775,
13.8571427568952));
#13606=CARTESIAN_POINT('Ctrl Pts',(-2.14637557782703,-2.40403019471789,
13.8563438300992));
#13607=CARTESIAN_POINT('Ctrl Pts',(-2.163610160559,-2.388516342501,13.8549257086795));
#13608=CARTESIAN_POINT('Ctrl Pts',(-2.17107301754225,-2.38173491264197,
13.8543075463185));
#13609=CARTESIAN_POINT('Ctrl Pts',(-2.18649842783968,-2.36758524224134,
13.8530212301857));
#13610=CARTESIAN_POINT('Ctrl Pts',(-2.19445583780695,-2.36021160609201,
13.8523528499798));
#13611=CARTESIAN_POINT('Ctrl Pts',(-2.2149053182932,-2.34106952902646,13.8506226123593));
#13612=CARTESIAN_POINT('Ctrl Pts',(-2.22734076000807,-2.32924134197813,
13.8495581827643));
#13613=CARTESIAN_POINT('Ctrl Pts',(-2.27992692897469,-2.27841689123593,
13.8450038129448));
#13614=CARTESIAN_POINT('Ctrl Pts',(-2.31915055819439,-2.23847948086697,
13.8414727395624));
#13615=CARTESIAN_POINT('Ctrl Pts',(-2.41979742033047,-2.13051521614022,
13.8320435057938));
#13616=CARTESIAN_POINT('Ctrl Pts',(-2.47938994046956,-2.06085847778673,
13.8260742277801));
#13617=CARTESIAN_POINT('Ctrl Pts',(-2.68733680650509,-1.79569929280763,
13.8037853191059));
#13618=CARTESIAN_POINT('Ctrl Pts',(-2.81618655403238,-1.58599904794723,
13.7869027223514));
#13619=CARTESIAN_POINT('Ctrl Pts',(-2.95809217792732,-1.28215198604447,
13.7646080669701));
#13620=CARTESIAN_POINT('Ctrl Pts',(-2.9927580909071,-1.19901012732734,13.7587190744549));
#13621=CARTESIAN_POINT('Ctrl Pts',(-3.028693413358,-1.10151075320558,13.7521377382162));
#13622=CARTESIAN_POINT('Ctrl Pts',(-3.03340358651978,-1.08847252105512,
13.7512642206489));
#13623=CARTESIAN_POINT('Ctrl Pts',(-3.04038615681228,-1.06874667428207,
13.7499530010915));
#13624=CARTESIAN_POINT('Ctrl Pts',(-3.04272087001189,-1.06208151559836,
13.7495117282581));
#13625=CARTESIAN_POINT('Ctrl Pts',(-3.04686168534694,-1.0501345583423,13.748724011933));
#13626=CARTESIAN_POINT('Ctrl Pts',(-3.04867598500958,-1.04485571264213,
13.7483770883238));
#13627=CARTESIAN_POINT('Ctrl Pts',(-3.05257896700212,-1.03340296605372,
13.7476268836894));
#13628=CARTESIAN_POINT('Ctrl Pts',(-3.05466263278768,-1.02722745371197,
13.7472239011641));
#13629=CARTESIAN_POINT('Ctrl Pts',(-3.06044154448486,-1.00992699352833,
13.7460991560499));
#13630=CARTESIAN_POINT('Ctrl Pts',(-3.0640948913819,-0.998788008494019,
13.7453798274397));
#13631=CARTESIAN_POINT('Ctrl Pts',(-3.08519785149469,-0.93323983538195,
13.7411739263593));
#13632=CARTESIAN_POINT('Ctrl Pts',(-3.10125996544684,-0.878390534686486,
13.7377636513281));
#13633=CARTESIAN_POINT('Ctrl Pts',(-3.18058642451351,-0.578113508837934,
13.7195370382248));
#13634=CARTESIAN_POINT('Ctrl Pts',(-3.21619491058329,-0.326285608225221,
13.7057827935169));
#13635=CARTESIAN_POINT('Ctrl Pts',(-3.22562274707539,0.0905874172435899,
13.6822276235085));
#13636=CARTESIAN_POINT('Ctrl Pts',(-3.21687571246231,0.254063868117312,
13.6728051940844));
#13637=CARTESIAN_POINT('Ctrl Pts',(-3.19293929805797,0.437876549399655,
13.6616560295008));
#13638=CARTESIAN_POINT('Ctrl Pts',(-3.18988987774838,0.459564756225506,
13.6603319869841));
#13639=CARTESIAN_POINT('Ctrl Pts',(-3.18466441909867,0.494167550209274,
13.6582051524482));
#13640=CARTESIAN_POINT('Ctrl Pts',(-3.18263027271072,0.507103114992514,
13.6574068592696));
#13641=CARTESIAN_POINT('Ctrl Pts',(-3.17889051030178,0.529975787586873,
13.6559894711812));
#13642=CARTESIAN_POINT('Ctrl Pts',(-3.17721698043603,0.539918019216727,
13.6553714049834));
#13643=CARTESIAN_POINT('Ctrl Pts',(-3.17364511867495,0.560546175040645,
13.6540848986102));
#13644=CARTESIAN_POINT('Ctrl Pts',(-3.17173940665668,0.571230676075219,
13.6534162300606));
#13645=CARTESIAN_POINT('Ctrl Pts',(-3.16667716027091,0.598805966746297,
13.6516844068493));
#13646=CARTESIAN_POINT('Ctrl Pts',(-3.16343947281233,0.615681335279812,
13.6506186710489));
#13647=CARTESIAN_POINT('Ctrl Pts',(-3.14904444515144,0.687597719786117,
13.646051135372));
#13648=CARTESIAN_POINT('Ctrl Pts',(-3.13658490945476,0.742365144170672,
13.6425079059423));
#13649=CARTESIAN_POINT('Ctrl Pts',(-3.09993888730017,0.885987095718178,
13.633037959115));
#13650=CARTESIAN_POINT('Ctrl Pts',(-3.07336571726649,0.974173944725516,
13.6270393580275));
#13651=CARTESIAN_POINT('Ctrl Pts',(-2.96367548140917,1.28874820706117,13.6049988003053));
#13652=CARTESIAN_POINT('Ctrl Pts',(-2.85900920374412,1.50675012446826,13.5884208857116));
#13653=CARTESIAN_POINT('Ctrl Pts',(-2.68142134092985,1.79020258254658,13.5661559125677));
#13654=CARTESIAN_POINT('Ctrl Pts',(-2.62839566569023,1.86718651204528,13.5600372081405));
#13655=CARTESIAN_POINT('Ctrl Pts',(-2.56367300761934,1.95291925709105,13.5532326671665));
#13656=CARTESIAN_POINT('Ctrl Pts',(-2.5551790499884,1.96401959100875,13.5523518560313));
#13657=CARTESIAN_POINT('Ctrl Pts',(-2.54226998144362,1.98066431351743,13.551031867226));
#13658=CARTESIAN_POINT('Ctrl Pts',(-2.53790848971449,1.98624980339979,13.5505890489268));
#13659=CARTESIAN_POINT('Ctrl Pts',(-2.53007751054666,1.99621054290907,13.549799666462));
#13660=CARTESIAN_POINT('Ctrl Pts',(-2.52661505469898,2.00059118961085,13.549452613532));
#13661=CARTESIAN_POINT('Ctrl Pts',(-2.51909753232944,2.0100515989803,13.5487033704109));
#13662=CARTESIAN_POINT('Ctrl Pts',(-2.51503849099403,2.01512808489499,13.5483014720329));
#13663=CARTESIAN_POINT('Ctrl Pts',(-2.50366705809702,2.02926201629485,13.5471828114905));
#13664=CARTESIAN_POINT('Ctrl Pts',(-2.49632082252718,2.03829228258205,13.5464684409392));
#13665=CARTESIAN_POINT('Ctrl Pts',(-2.45349026034932,2.09036231968875,13.5423499755261));
#13666=CARTESIAN_POINT('Ctrl Pts',(-2.41693982384847,2.13251772423204,13.5390185239296));
#13667=CARTESIAN_POINT('Ctrl Pts',(-2.20769910009121,2.36154997597489,13.520796381851));
#13668=CARTESIAN_POINT('Ctrl Pts',(-2.01443066061862,2.52842841246223,13.5069900726337));
#13669=CARTESIAN_POINT('Ctrl Pts',(-1.66770050215146,2.76256278142866,13.483358762301));
#13670=CARTESIAN_POINT('Ctrl Pts',(-1.52509496310787,2.84377442822509,13.4739150247416));
#13671=CARTESIAN_POINT('Ctrl Pts',(-1.35708863378552,2.92316785186097,13.4627389780137));
#13672=CARTESIAN_POINT('Ctrl Pts',(-1.33713799125516,2.93234749064328,13.4614113787347));
#13673=CARTESIAN_POINT('Ctrl Pts',(-1.30512850881835,2.94668102470496,13.4592799104338));
#13674=CARTESIAN_POINT('Ctrl Pts',(-1.29312910837099,2.95196656264869,13.4584805716562));
#13675=CARTESIAN_POINT('Ctrl Pts',(-1.27184410397463,2.96118757295278,13.4570619732111));
#13676=CARTESIAN_POINT('Ctrl Pts',(-1.26257160148976,2.96515298331546,13.4564437481153));
#13677=CARTESIAN_POINT('Ctrl Pts',(-1.2432888067475,2.97329247348944,13.455157554643));
#13678=CARTESIAN_POINT('Ctrl Pts',(-1.23327576332165,2.97745966839048,13.4544893610906));
#13679=CARTESIAN_POINT('Ctrl Pts',(-1.2073764243642,2.98808530944424,13.4527601500264));
#13680=CARTESIAN_POINT('Ctrl Pts',(-1.19145942776883,2.99446757542719,13.4516965661283));
#13681=CARTESIAN_POINT('Ctrl Pts',(-1.12349114483691,3.02109323277472,13.4471507001349));
#13682=CARTESIAN_POINT('Ctrl Pts',(-1.07097188995434,3.04010777025807,13.443627475715));
#13683=CARTESIAN_POINT('Ctrl Pts',(-0.931308748587889,3.08660453434112,
13.4342244952542));
#13684=CARTESIAN_POINT('Ctrl Pts',(-0.843449136185809,3.11176069340846,
13.428274113069));
#13685=CARTESIAN_POINT('Ctrl Pts',(-0.514007625866643,3.19110950358245,
13.4058632639788));
#13686=CARTESIAN_POINT('Ctrl Pts',(-0.267519530766325,3.22114906003356,
13.3888254172375));
#13687=CARTESIAN_POINT('Ctrl Pts',(0.0683554982004519,3.22323726544437,
13.366509294822));
#13688=CARTESIAN_POINT('Ctrl Pts',(0.156741438929809,3.22015001854749,13.3607309370937));
#13689=CARTESIAN_POINT('Ctrl Pts',(0.258660421649681,3.21238274392139,13.3542574994357));
#13690=CARTESIAN_POINT('Ctrl Pts',(0.272417711615473,3.21124535244927,13.3533877267107));
#13691=CARTESIAN_POINT('Ctrl Pts',(0.293189288914914,3.20939360315166,13.3520810122999));
#13692=CARTESIAN_POINT('Ctrl Pts',(0.300209029068424,3.20874458319702,13.3516405353656));
#13693=CARTESIAN_POINT('Ctrl Pts',(0.312782247797374,3.20754048697188,13.3508536742618));
#13694=CARTESIAN_POINT('Ctrl Pts',(0.318336443286197,3.20699401628944,13.3505068144321));
#13695=CARTESIAN_POINT('Ctrl Pts',(0.330383106417583,3.20577715459673,13.3497561017607));
#13696=CARTESIAN_POINT('Ctrl Pts',(0.336874945860679,3.20510147024643,13.3493525509116));
#13697=CARTESIAN_POINT('Ctrl Pts',(0.355063226827502,3.20315252416093,13.3482246121953));
#13698=CARTESIAN_POINT('Ctrl Pts',(0.366754955893441,3.20183491147731,13.3475026806788));
#13699=CARTESIAN_POINT('Ctrl Pts',(0.435906375976321,3.19365806251771,13.3432498990653));
#13700=CARTESIAN_POINT('Ctrl Pts',(0.493184089225305,3.18531577838369,13.3397973447783));
#13701=CARTESIAN_POINT('Ctrl Pts',(0.799402117971898,3.13225714526095,13.3215676277044));
#13702=CARTESIAN_POINT('Ctrl Pts',(1.04266783510849,3.05989358148588,13.3078407872682));
#13703=CARTESIAN_POINT('Ctrl Pts',(1.42481624202104,2.89527727577188,13.2843339292745));
#13704=CARTESIAN_POINT('Ctrl Pts',(1.56950911323301,2.8194614094535,13.2749313441962));
#13705=CARTESIAN_POINT('Ctrl Pts',(1.72808506189678,2.72036946197471,13.2636847783017));
#13706=CARTESIAN_POINT('Ctrl Pts',(1.74819762755504,2.70748831921958,13.2622402899411));
#13707=CARTESIAN_POINT('Ctrl Pts',(1.77867118788821,2.68749033309294,13.2600230577577));
#13708=CARTESIAN_POINT('Ctrl Pts',(1.7891370811748,2.68053427189861,13.2592563403086));
#13709=CARTESIAN_POINT('Ctrl Pts',(1.80766180439341,2.66806515982784,13.2578897934385));
#13710=CARTESIAN_POINT('Ctrl Pts',(1.81573681032634,2.66257633288509,13.2572908867698));
#13711=CARTESIAN_POINT('Ctrl Pts',(1.82396708114496,2.65692711553739,13.2566771284976));
#13712=CARTESIAN_POINT('Ctrl Pts',(1.82414747100889,2.65680326979342,13.2566636745902));
#13713=CARTESIAN_POINT('Ctrl Pts',(1.82449631202256,2.6565637224954,13.2566376540142));
#13714=CARTESIAN_POINT('Ctrl Pts',(1.82466476963494,2.65644801995459,13.2566250870734));
#13715=CARTESIAN_POINT('Ctrl Pts',(1.82499103828847,2.65622388162727,13.2566007446468));
#13716=CARTESIAN_POINT('Ctrl Pts',(1.82514884549013,2.65611545136244,13.2565889696231));
#13717=CARTESIAN_POINT('Ctrl Pts',(1.82545489885312,2.65590512012645,13.2565661305442));
#13718=CARTESIAN_POINT('Ctrl Pts',(1.82560314615233,2.65580322080147,13.2565550665517));
#13719=CARTESIAN_POINT('Ctrl Pts',(1.82589102085572,2.65560531163277,13.2565335797267));
#13720=CARTESIAN_POINT('Ctrl Pts',(1.82603064921561,2.65550930319193,13.2565231569483));
#13721=CARTESIAN_POINT('Ctrl Pts',(1.82630210199719,2.65532262076383,13.2565028920095));
#13722=CARTESIAN_POINT('Ctrl Pts',(1.82643392724926,2.65523194796468,13.2564930498941));
#13723=CARTESIAN_POINT('Ctrl Pts',(1.8266904854685,2.65505545247603,13.2564738934623));
#13724=CARTESIAN_POINT('Ctrl Pts',(1.82681521913522,2.65496963081685,13.2564645791856));
#13725=CARTESIAN_POINT('Ctrl Pts',(1.82705821814233,2.6548024127288,13.2564464321075));
#13726=CARTESIAN_POINT('Ctrl Pts',(1.82717648409353,2.65472101718573,13.25643759934));
#13727=CARTESIAN_POINT('Ctrl Pts',(1.82740709745644,2.65456227677371,13.256420374452));
#13728=CARTESIAN_POINT('Ctrl Pts',(1.82751944541041,2.65448493266603,13.2564119823601));
#13729=CARTESIAN_POINT('Ctrl Pts',(1.82773870948594,2.65433396338863,13.2563956026701));
#13730=CARTESIAN_POINT('Ctrl Pts',(1.82784562606501,2.6542603388942,13.2563876150982));
#13731=CARTESIAN_POINT('Ctrl Pts',(1.82805446002122,2.65411651383503,13.2563720123042));
#13732=CARTESIAN_POINT('Ctrl Pts',(1.82815637780279,2.65404631386008,13.2563643971047));
#13733=CARTESIAN_POINT('Ctrl Pts',(1.82835560025163,2.65390907445809,13.2563495103625));
#13734=CARTESIAN_POINT('Ctrl Pts',(1.82845290528395,2.65384203554416,13.2563422388392));
#13735=CARTESIAN_POINT('Ctrl Pts',(1.82864324808455,2.6537108822367,13.2563280137412));
#13736=CARTESIAN_POINT('Ctrl Pts',(1.82873628616771,2.65364676830211,13.2563210601842));
#13737=CARTESIAN_POINT('Ctrl Pts',(1.82891840595857,2.65352125270398,13.2563074479043));
#13738=CARTESIAN_POINT('Ctrl Pts',(1.82900748792792,2.65345985145985,13.2563007891985));
#13739=CARTESIAN_POINT('Ctrl Pts',(1.82918197571369,2.65333956986007,13.2562877457825));
#13740=CARTESIAN_POINT('Ctrl Pts',(1.82926738180885,2.6532806898463,13.2562813610841));
#13741=CARTESIAN_POINT('Ctrl Pts',(1.82943477139101,2.65316527748324,13.2562688468243));
#13742=CARTESIAN_POINT('Ctrl Pts',(1.82951675510313,2.65310874545581,13.2562627172752));
#13743=CARTESIAN_POINT('Ctrl Pts',(1.82967752985226,2.65299787192051,13.2562506962088));
#13744=CARTESIAN_POINT('Ctrl Pts',(1.82975632108939,2.65294353070216,13.2562448047025));
#13745=CARTESIAN_POINT('Ctrl Pts',(1.82991092003765,2.65283689579824,13.2562332441597));
#13746=CARTESIAN_POINT('Ctrl Pts',(1.82998672791179,2.65278460238447,13.2562275751343));
#13747=CARTESIAN_POINT('Ctrl Pts',(1.83986503517043,2.64596977226778,13.2554888225628));
#13748=CARTESIAN_POINT('Ctrl Pts',(1.84962987022553,2.63915303089014,13.254753667877));
#13749=CARTESIAN_POINT('Ctrl Pts',(1.86983555667426,2.62488040710172,13.2532221729703));
#13750=CARTESIAN_POINT('Ctrl Pts',(1.88027010020347,2.61741599735144,13.2524255117581));
#13751=CARTESIAN_POINT('Ctrl Pts',(1.93725188108929,2.57613717978342,13.2480429712109));
#13752=CARTESIAN_POINT('Ctrl Pts',(1.98292928738133,2.54114509091567,13.244411482129));
#13753=CARTESIAN_POINT('Ctrl Pts',(2.10167304200838,2.44502744336957,13.2346439710303));
#13754=CARTESIAN_POINT('Ctrl Pts',(2.17300355299145,2.38185674476608,13.2284303222268));
#13755=CARTESIAN_POINT('Ctrl Pts',(2.34373830785972,2.21659271736009,13.212686524404));
#13756=CARTESIAN_POINT('Ctrl Pts',(2.43936775474247,2.11089385302071,13.2030493433906));
#13757=CARTESIAN_POINT('Ctrl Pts',(2.64328784588221,1.85307079718243,13.1807994533654));
#13758=CARTESIAN_POINT('Ctrl Pts',(2.74600647518844,1.69714666823927,13.1682213424386));
#13759=CARTESIAN_POINT('Ctrl Pts',(2.84165769087714,1.52030071515126,13.1554777750602));
#13760=CARTESIAN_POINT('Ctrl Pts',(2.84854763418732,1.50735168145237,13.1545530969659));
#13761=CARTESIAN_POINT('Ctrl Pts',(2.85865530732638,1.48803838556439,13.1531869481878));
#13762=CARTESIAN_POINT('Ctrl Pts',(2.86194059524063,1.48170996981639,13.1527413591609));
#13763=CARTESIAN_POINT('Ctrl Pts',(2.86776278822654,1.47040313242541,13.1519489721851));
#13764=CARTESIAN_POINT('Ctrl Pts',(2.87030776870668,1.46542898016969,13.1516016699928));
#13765=CARTESIAN_POINT('Ctrl Pts',(2.87577127136868,1.45468175260473,13.1508540711102));
#13766=CARTESIAN_POINT('Ctrl Pts',(2.87868534392187,1.44890651838495,13.1504540545464));
#13767=CARTESIAN_POINT('Ctrl Pts',(2.8867312543569,1.43284069503262,13.1493459325319));
#13768=CARTESIAN_POINT('Ctrl Pts',(2.89182549434616,1.4225312340237,13.1486401461141));
#13769=CARTESIAN_POINT('Ctrl Pts',(2.92031736028403,1.36408526697886,13.1446675649681));
#13770=CARTESIAN_POINT('Ctrl Pts',(2.94256970216377,1.31539591920006,13.1414675274994));
#13771=CARTESIAN_POINT('Ctrl Pts',(3.06424136383938,1.03061133214331,13.1232489150708));
#13772=CARTESIAN_POINT('Ctrl Pts',(3.13644897315352,0.783869572471844,13.1093529120562));
#13773=CARTESIAN_POINT('Ctrl Pts',(3.20070073527963,0.399359848305915,13.0873376944129));
#13774=CARTESIAN_POINT('Ctrl Pts',(3.21450392718355,0.266331696759462,13.0796706962223));
#13775=CARTESIAN_POINT('Ctrl Pts',(3.22119157718624,0.104223928745983,13.0700514696201));
#13776=CARTESIAN_POINT('Ctrl Pts',(3.22199056138468,0.0755946409071718,
13.068342574647));
#13777=CARTESIAN_POINT('Ctrl Pts',(3.22263444413199,0.0314104431670769,
13.0656878356073));
#13778=CARTESIAN_POINT('Ctrl Pts',(3.22274848599569,0.0158605448984554,
13.0647502303399));
#13779=CARTESIAN_POINT('Ctrl Pts',(3.22274998502511,0.000310677704944338,
13.0638091501483));
#13780=CARTESIAN_POINT('Ctrl Pts',(3.22274998514752,0.000309405382385037,
13.0638090731471));
#13781=CARTESIAN_POINT('Ctrl Pts',(3.22275119902617,-0.0123342900247772,
13.0630438747345));
#13782=CARTESIAN_POINT('Ctrl Pts',(3.22267800609396,-0.0249777782407157,
13.062276390535));
#13783=CARTESIAN_POINT('Ctrl Pts',(3.22241626611493,-0.0473981902040759,
13.0609112122533));
#13784=CARTESIAN_POINT('Ctrl Pts',(3.22225761857131,-0.0571753163518782,
13.0603144614021));
#13785=CARTESIAN_POINT('Ctrl Pts',(3.22185504357169,-0.0765493239484438,
13.0591290771725));
#13786=CARTESIAN_POINT('Ctrl Pts',(3.22161272659472,-0.0861461401344853,
13.0585405004048));
#13787=CARTESIAN_POINT('Ctrl Pts',(3.22104429950888,-0.105271461766646,
13.0573646830768));
#13788=CARTESIAN_POINT('Ctrl Pts',(3.22071877733159,-0.114799887972164,
13.0567774669285));
#13789=CARTESIAN_POINT('Ctrl Pts',(3.21973418090167,-0.140303238418092,
13.0552019017124));
#13790=CARTESIAN_POINT('Ctrl Pts',(3.21899850461072,-0.156274779957418,
13.0542111539936));
#13791=CARTESIAN_POINT('Ctrl Pts',(3.21587088744193,-0.21471140892968,13.0505710168166));
#13792=CARTESIAN_POINT('Ctrl Pts',(3.212757294087,-0.257131957836759,13.0478990935361));
#13793=CARTESIAN_POINT('Ctrl Pts',(3.17882940242412,-0.620659162934107,
13.0247379994649));
#13794=CARTESIAN_POINT('Ctrl Pts',(3.10080090528168,-0.935477557963266,
13.0026390784345));
#13795=CARTESIAN_POINT('Ctrl Pts',(2.93529802703581,-1.33500792121011,12.9736255945994));
#13796=CARTESIAN_POINT('Ctrl Pts',(2.88801347589584,-1.43443500080322,12.9663447777142));
#13797=CARTESIAN_POINT('Ctrl Pts',(2.82558525661003,-1.55004562884681,12.9579594462058));
#13798=CARTESIAN_POINT('Ctrl Pts',(2.81525300971195,-1.56873326049306,12.9566067059801));
#13799=CARTESIAN_POINT('Ctrl Pts',(2.80064694735087,-1.59454167238341,12.9547437232736));
#13800=CARTESIAN_POINT('Ctrl Pts',(2.79653047593873,-1.6017502206779,12.954223943739));
#13801=CARTESIAN_POINT('Ctrl Pts',(2.78950604055004,-1.61394141548422,12.9533459600165));
#13802=CARTESIAN_POINT('Ctrl Pts',(2.78661248375302,-1.61893227469542,12.9529868361295));
#13803=CARTESIAN_POINT('Ctrl Pts',(2.78106454856922,-1.62844251003251,12.9523031403497));
#13804=CARTESIAN_POINT('Ctrl Pts',(2.77841253452232,-1.63296320250473,12.9519784139127));
#13805=CARTESIAN_POINT('Ctrl Pts',(2.77140214404592,-1.64484677855304,12.9511254565011));
#13806=CARTESIAN_POINT('Ctrl Pts',(2.76702541836773,-1.65219887028441,12.9505984138741));
#13807=CARTESIAN_POINT('Ctrl Pts',(2.75161026250186,-1.67786042375699,12.9487608444603));
#13808=CARTESIAN_POINT('Ctrl Pts',(2.74041868421446,-1.69607786667844,12.9474599212906));
#13809=CARTESIAN_POINT('Ctrl Pts',(2.59724133330157,-1.92402178358547,12.9312099961186));
#13810=CARTESIAN_POINT('Ctrl Pts',(2.44165315088042,-2.11799220538469,12.9176357934344));
#13811=CARTESIAN_POINT('Ctrl Pts',(2.11481365107245,-2.44099822242077,12.8919025499043));
#13812=CARTESIAN_POINT('Ctrl Pts',(1.95001647775332,-2.57455377885432,12.8798856179341));
#13813=CARTESIAN_POINT('Ctrl Pts',(1.75916989388126,-2.70031970899399,12.8661353192103));
#13814=CARTESIAN_POINT('Ctrl Pts',(1.74493405863099,-2.70954061799208,12.8651108740881));
#13815=CARTESIAN_POINT('Ctrl Pts',(1.72096373665046,-2.7247995484285,12.8633876186979));
#13816=CARTESIAN_POINT('Ctrl Pts',(1.71126854484763,-2.73089888573605,12.8626910825326));
#13817=CARTESIAN_POINT('Ctrl Pts',(1.69226589332731,-2.7427127064052,12.8613266560411));
#13818=CARTESIAN_POINT('Ctrl Pts',(1.68296148561487,-2.74843182140175,12.860658948299));
#13819=CARTESIAN_POINT('Ctrl Pts',(1.66531738539575,-2.75915388224619,12.8593933689835));
#13820=CARTESIAN_POINT('Ctrl Pts',(1.65698375018078,-2.76416659923867,12.8587958658004));
#13821=CARTESIAN_POINT('Ctrl Pts',(1.63783130545497,-2.77556914033468,12.8574231914112));
#13822=CARTESIAN_POINT('Ctrl Pts',(1.62699761212112,-2.78193353638748,12.8566471027428));
#13823=CARTESIAN_POINT('Ctrl Pts',(1.59547096301335,-2.80020713382859,12.8543895599933));
#13824=CARTESIAN_POINT('Ctrl Pts',(1.57468288148178,-2.81194974339738,12.8529021118477));
#13825=CARTESIAN_POINT('Ctrl Pts',(1.41072778233451,-2.90217519996156,12.8411771459762));
#13826=CARTESIAN_POINT('Ctrl Pts',(1.2619367389219,-2.96989476271101,12.8305566484586));
#13827=CARTESIAN_POINT('Ctrl Pts',(0.870986988370921,-3.11313012284401,
12.8027905526368));
#13828=CARTESIAN_POINT('Ctrl Pts',(0.623878354689254,-3.17190293184503,
12.7853195598051));
#13829=CARTESIAN_POINT('Ctrl Pts',(0.31524401270032,-3.20781154981545,12.7649783010641));
#13830=CARTESIAN_POINT('Ctrl Pts',(0.257871271765716,-3.21293278936775,
12.7612626594714));
#13831=CARTESIAN_POINT('Ctrl Pts',(0.188661883698338,-3.21724451885631,
12.7568832315541));
#13832=CARTESIAN_POINT('Ctrl Pts',(0.176931540294084,-3.2179109435394,12.7561445106756));
#13833=CARTESIAN_POINT('Ctrl Pts',(0.158682940705784,-3.21884759494317,
12.755001096622));
#13834=CARTESIAN_POINT('Ctrl Pts',(0.152167208892545,-3.21916219806809,
12.7545939846412));
#13835=CARTESIAN_POINT('Ctrl Pts',(0.140074805848101,-3.21970926688188,
12.7538406215615));
#13836=CARTESIAN_POINT('Ctrl Pts',(0.134498537636614,-3.21994702729603,
12.7534940861688));
#13837=CARTESIAN_POINT('Ctrl Pts',(0.12187280824391,-3.22045250631243,12.7527114095447));
#13838=CARTESIAN_POINT('Ctrl Pts',(0.114823086455957,-3.220711565455,12.7522757587842));
#13839=CARTESIAN_POINT('Ctrl Pts',(0.0939539996455488,-3.22140984243835,
12.7509900069638));
#13840=CARTESIAN_POINT('Ctrl Pts',(0.0801323876580535,-3.22178328621796,
12.7501435034033));
#13841=CARTESIAN_POINT('Ctrl Pts',(-0.0226838977505775,-3.22389919302676,
12.7438812564736));
#13842=CARTESIAN_POINT('Ctrl Pts',(-0.111722977459457,-3.22204308678329,
12.7386513038527));
#13843=CARTESIAN_POINT('Ctrl Pts',(-0.446771128824899,-3.20114968864684,
12.7193226341891));
#13844=CARTESIAN_POINT('Ctrl Pts',(-0.690395170900753,-3.15758336300304,
12.7059249965003));
#13845=CARTESIAN_POINT('Ctrl Pts',(-1.01427312948718,-3.06034841874645,
12.6866691705564));
#13846=CARTESIAN_POINT('Ctrl Pts',(-1.10070523818209,-3.03033471719388,
12.6813890255472));
#13847=CARTESIAN_POINT('Ctrl Pts',(-1.23771352645921,-2.97612281282823,
12.6726996975242));
#13848=CARTESIAN_POINT('Ctrl Pts',(-1.28914098489699,-2.95420999953359,
12.6693631673588));
#13849=CARTESIAN_POINT('Ctrl Pts',(-1.35557130146388,-2.9238396444789,12.6649430044264));
#13850=CARTESIAN_POINT('Ctrl Pts',(-1.37111473608007,-2.91658296346666,
12.6639007496217));
#13851=CARTESIAN_POINT('Ctrl Pts',(-1.39639069799493,-2.90453580329068,
12.6621924303761));
#13852=CARTESIAN_POINT('Ctrl Pts',(-1.40615840992103,-2.89981960399327,
12.6615289546448));
#13853=CARTESIAN_POINT('Ctrl Pts',(-1.42496108559957,-2.89062366339293,
12.6602452925046));
#13854=CARTESIAN_POINT('Ctrl Pts',(-1.4339992083745,-2.88615064151755,12.6596253470745));
#13855=CARTESIAN_POINT('Ctrl Pts',(-1.45379319400704,-2.87623854752048,
12.6582611583369));
#13856=CARTESIAN_POINT('Ctrl Pts',(-1.46453979368046,-2.87078143005618,
12.6575162864758));
#13857=CARTESIAN_POINT('Ctrl Pts',(-1.47525540501245,-2.86526422036111,
12.6567692800014));
#13858=CARTESIAN_POINT('Ctrl Pts',(-1.47525514217493,-2.86526435568979,
12.4082778759135));
#13859=CARTESIAN_POINT('Ctrl Pts',(-1.32807964289666,-2.94104145167791,
12.4175660823812));
#13860=CARTESIAN_POINT('Ctrl Pts',(-1.17517331519269,-3.00542385950792,
12.4267296437769));
#13861=CARTESIAN_POINT('Ctrl Pts',(-0.931083016729306,-3.08667586857259,
12.441378750016));
#13862=CARTESIAN_POINT('Ctrl Pts',(-0.843114619318536,-3.11185464542109,
12.4466592428265));
#13863=CARTESIAN_POINT('Ctrl Pts',(-0.69985798827533,-3.14633761954119,
12.4553488670451));
#13864=CARTESIAN_POINT('Ctrl Pts',(-0.645188435910395,-3.1580014141481,
12.4586853274482));
#13865=CARTESIAN_POINT('Ctrl Pts',(-0.573385657482078,-3.17137833986141,
12.463105186689));
#13866=CARTESIAN_POINT('Ctrl Pts',(-0.556501154831585,-3.17438468584578,
12.4641472076288));
#13867=CARTESIAN_POINT('Ctrl Pts',(-0.528903383519519,-3.17907161804855,
12.4658550885166));
#13868=CARTESIAN_POINT('Ctrl Pts',(-0.518204066352105,-3.18083317431952,
12.466518360654));
#13869=CARTESIAN_POINT('Ctrl Pts',(-0.497541203884748,-3.18412812778795,
12.4678015894037));
#13870=CARTESIAN_POINT('Ctrl Pts',(-0.487578940676515,-3.18566883976614,
12.4684213050038));
#13871=CARTESIAN_POINT('Ctrl Pts',(-0.46465077986819,-3.18910472078019,
12.4698500154164));
#13872=CARTESIAN_POINT('Ctrl Pts',(-0.451680290949744,-3.19096759211842,
12.4706600261323));
#13873=CARTESIAN_POINT('Ctrl Pts',(-0.416962725831033,-3.19573794787928,
12.4728330865919));
#13874=CARTESIAN_POINT('Ctrl Pts',(-0.395197012861291,-3.19850249786062,
12.4742006347867));
#13875=CARTESIAN_POINT('Ctrl Pts',(-0.208787010211332,-3.2202474197314,
12.4859590069656));
#13876=CARTESIAN_POINT('Ctrl Pts',(-0.0429591055232302,-3.22672044094313,
12.4967463871683));
#13877=CARTESIAN_POINT('Ctrl Pts',(0.380799355072473,-3.21058686226732,
12.5250441529312));
#13878=CARTESIAN_POINT('Ctrl Pts',(0.636857764156288,-3.16974519918415,
12.5428915885471));
#13879=CARTESIAN_POINT('Ctrl Pts',(0.934019170458942,-3.0848491542892,12.563044025325));
#13880=CARTESIAN_POINT('Ctrl Pts',(0.982418519562595,-3.06977859962972,
12.5663042640375));
#13881=CARTESIAN_POINT('Ctrl Pts',(1.04115982971537,-3.04995600718061,12.5702173096445));
#13882=CARTESIAN_POINT('Ctrl Pts',(1.05185544222868,-3.04628389589195,12.5709279952417));
#13883=CARTESIAN_POINT('Ctrl Pts',(1.06859784199426,-3.04043705749284,12.5720373917615));
#13884=CARTESIAN_POINT('Ctrl Pts',(1.07465770741686,-3.03830045619146,12.5724383001979));
#13885=CARTESIAN_POINT('Ctrl Pts',(1.0859785386791,-3.03427082444546,12.5731860211055));
#13886=CARTESIAN_POINT('Ctrl Pts',(1.09124090944121,-3.03238224844945,12.5735330813293));
#13887=CARTESIAN_POINT('Ctrl Pts',(1.10325799770103,-3.02803418508311,12.574324485739));
#13888=CARTESIAN_POINT('Ctrl Pts',(1.11000940665089,-3.02556579089449,12.5747682924215));
#13889=CARTESIAN_POINT('Ctrl Pts',(1.13079581765924,-3.01788709301247,12.5761323358988));
#13890=CARTESIAN_POINT('Ctrl Pts',(1.14480305434446,-3.01260147949301,12.5770481927608));
#13891=CARTESIAN_POINT('Ctrl Pts',(1.31169888091134,-2.94829140951464,12.5879265564671));
#13892=CARTESIAN_POINT('Ctrl Pts',(1.4599297277231,-2.87777632466277,12.5972517623185));
#13893=CARTESIAN_POINT('Ctrl Pts',(1.74402251538407,-2.7150012027269,12.6156379056276));
#13894=CARTESIAN_POINT('Ctrl Pts',(1.87948320605962,-2.62304942145194,12.6246777734408));
#13895=CARTESIAN_POINT('Ctrl Pts',(2.08234395733136,-2.46153261112885,12.6394140712876));
#13896=CARTESIAN_POINT('Ctrl Pts',(2.15460196470166,-2.39853859479889,12.644935017842));
#13897=CARTESIAN_POINT('Ctrl Pts',(2.2657581053933,-2.29255227765536,12.6539833537267));
#13898=CARTESIAN_POINT('Ctrl Pts',(2.30649151818237,-2.25156656282776,12.6574299549641));
#13899=CARTESIAN_POINT('Ctrl Pts',(2.35799772013009,-2.19687630329258,12.6619752616268));
#13900=CARTESIAN_POINT('Ctrl Pts',(2.36979347626904,-2.18414688187869,12.6630295453128));
#13901=CARTESIAN_POINT('Ctrl Pts',(2.38882175317119,-2.16327685529851,12.6647524745948));
#13902=CARTESIAN_POINT('Ctrl Pts',(2.39611694107342,-2.15519366210888,12.6654184437282));
#13903=CARTESIAN_POINT('Ctrl Pts',(2.4100765445244,-2.13956769408213,12.6667033742869));
#13904=CARTESIAN_POINT('Ctrl Pts',(2.41674687133113,-2.13203035256774,12.6673220757543));
#13905=CARTESIAN_POINT('Ctrl Pts',(2.43195284746966,-2.11468483855536,12.6687434465091));
#13906=CARTESIAN_POINT('Ctrl Pts',(2.4404646246128,-2.10485605844719,12.6695470976707));
#13907=CARTESIAN_POINT('Ctrl Pts',(2.46295361190521,-2.07856761883061,12.6716920644322));
#13908=CARTESIAN_POINT('Ctrl Pts',(2.47682507865841,-2.06201875198085,12.6730376976517));
#13909=CARTESIAN_POINT('Ctrl Pts',(2.58558647651959,-1.92958382203471,12.68377150118));
#13910=CARTESIAN_POINT('Ctrl Pts',(2.67244554100373,-1.80736676720248,12.6934808220081));
#13911=CARTESIAN_POINT('Ctrl Pts',(2.86744260258071,-1.48803707138875,12.7183364730947));
#13912=CARTESIAN_POINT('Ctrl Pts',(2.96406624210033,-1.2848280678903,12.7337429744435));
#13913=CARTESIAN_POINT('Ctrl Pts',(3.06840533998564,-0.989399829864131,
12.7546184921491));
#13914=CARTESIAN_POINT('Ctrl Pts',(3.09453617955183,-0.904362837698054,
12.7604549186173));
#13915=CARTESIAN_POINT('Ctrl Pts',(3.12197045948239,-0.799864454496833,
12.7673351950641));
#13916=CARTESIAN_POINT('Ctrl Pts',(3.12665829718623,-0.781338997897061,
12.7685439255011));
#13917=CARTESIAN_POINT('Ctrl Pts',(3.13305998437349,-0.755060068471666,
12.7702419412962));
#13918=CARTESIAN_POINT('Ctrl Pts',(3.1349102780138,-0.747340701864984,12.7707387089341));
#13919=CARTESIAN_POINT('Ctrl Pts',(3.13803994037495,-0.734067689367205,
12.7715893114564));
#13920=CARTESIAN_POINT('Ctrl Pts',(3.13933312778204,-0.728517367503911,
12.7719439360743));
#13921=CARTESIAN_POINT('Ctrl Pts',(3.1418054056881,-0.717777594063654,12.7726280297301));
#13922=CARTESIAN_POINT('Ctrl Pts',(3.14298636664496,-0.712588648388276,
12.7729576099082));
#13923=CARTESIAN_POINT('Ctrl Pts',(3.14612596954831,-0.698634108110556,
12.7738414740361));
#13924=CARTESIAN_POINT('Ctrl Pts',(3.14806084676547,-0.6898631334293,12.7743944009279));
#13925=CARTESIAN_POINT('Ctrl Pts',(3.15504216740492,-0.657575086454122,
12.7764206266544));
#13926=CARTESIAN_POINT('Ctrl Pts',(3.15986211185853,-0.634009136853062,
12.7778815211945));
#13927=CARTESIAN_POINT('Ctrl Pts',(3.20302355340606,-0.410249413958796,
12.7916018108761));
#13928=CARTESIAN_POINT('Ctrl Pts',(3.22256012396323,-0.206867382593006,
12.8029491858007));
#13929=CARTESIAN_POINT('Ctrl Pts',(3.22296310569356,0.229014011018249,12.8273020880819));
#13930=CARTESIAN_POINT('Ctrl Pts',(3.19812848998415,0.460322081304765,12.8402815110925));
#13931=CARTESIAN_POINT('Ctrl Pts',(3.14083707101853,0.722921592924151,12.8563016916263));
#13932=CARTESIAN_POINT('Ctrl Pts',(3.13237345173311,0.758755248147586,12.8585146150015));
#13933=CARTESIAN_POINT('Ctrl Pts',(3.11958335295439,0.809039150874073,12.8616610990742));
#13934=CARTESIAN_POINT('Ctrl Pts',(3.11576633017217,0.823616905721149,12.8625782028728));
#13935=CARTESIAN_POINT('Ctrl Pts',(3.10941331294041,0.847203631754731,12.8640702519149));
#13936=CARTESIAN_POINT('Ctrl Pts',(3.10694003691891,0.856229378387173,12.8646431522876));
#13937=CARTESIAN_POINT('Ctrl Pts',(3.10169264103197,0.875056619371128,12.8658423268489));
#13938=CARTESIAN_POINT('Ctrl Pts',(3.09891129657857,0.884855976229839,12.866468831192));
#13939=CARTESIAN_POINT('Ctrl Pts',(3.09220597764269,0.908061046235031,12.8679580572882));
#13940=CARTESIAN_POINT('Ctrl Pts',(3.08824123810762,0.921454674538707,12.8688221050648));
#13941=CARTESIAN_POINT('Ctrl Pts',(3.07469214710865,0.966156198854201,12.8717211619859));
#13942=CARTESIAN_POINT('Ctrl Pts',(3.06471802291581,0.997342926156683,12.8737689147052));
#13943=CARTESIAN_POINT('Ctrl Pts',(3.00837016330244,1.16469649555872,12.884897572402));
#13944=CARTESIAN_POINT('Ctrl Pts',(2.95340038800004,1.29777704968047,12.8942617343917));
#13945=CARTESIAN_POINT('Ctrl Pts',(2.77953975058517,1.64991933857387,12.9204046279798));
#13946=CARTESIAN_POINT('Ctrl Pts',(2.64386722339222,1.85957879987468,12.9375692406869));
#13947=CARTESIAN_POINT('Ctrl Pts',(2.44311534142933,2.10278921598091,12.9583219593562));
#13948=CARTESIAN_POINT('Ctrl Pts',(2.39922654963696,2.15273046579338,12.9626294675551));
#13949=CARTESIAN_POINT('Ctrl Pts',(2.34585707858172,2.20979819804294,12.9675716736054));
#13950=CARTESIAN_POINT('Ctrl Pts',(2.33784673901691,2.21827098069142,12.9683059694807));
#13951=CARTESIAN_POINT('Ctrl Pts',(2.3248114187996,2.23190980097087,12.9694885686297));
#13952=CARTESIAN_POINT('Ctrl Pts',(2.31981486976677,2.23710269434689,12.9699389749901));
#13953=CARTESIAN_POINT('Ctrl Pts',(2.31090963060719,2.24629595573078,12.9707365294205));
#13954=CARTESIAN_POINT('Ctrl Pts',(2.30700790909753,2.25030294641519,12.9710842091079));
#13955=CARTESIAN_POINT('Ctrl Pts',(2.29860925613849,2.25888339383814,12.9718288259189));
#13956=CARTESIAN_POINT('Ctrl Pts',(2.2941091094302,2.26345357696786,12.9722255032189));
#13957=CARTESIAN_POINT('Ctrl Pts',(2.28167434553954,2.27600668418538,12.9733153815941));
#13958=CARTESIAN_POINT('Ctrl Pts',(2.27371141559396,2.28396161370644,12.9740063858905));
#13959=CARTESIAN_POINT('Ctrl Pts',(2.2302088974021,2.32696743274951,12.9777450912158));
#13960=CARTESIAN_POINT('Ctrl Pts',(2.19389814724152,2.36123288067854,12.980734915097));
#13961=CARTESIAN_POINT('Ctrl Pts',(1.96437123842322,2.56796285424501,12.998952949677));
#13962=CARTESIAN_POINT('Ctrl Pts',(1.75172921718002,2.7174737027081,13.0129954683047));
#13963=CARTESIAN_POINT('Ctrl Pts',(1.37722761058508,2.9183727880272,13.0369882672184));
#13964=CARTESIAN_POINT('Ctrl Pts',(1.22517275157435,2.98539722672146,13.0465446220541));
#13965=CARTESIAN_POINT('Ctrl Pts',(1.0479428742098,3.04769008871387,13.0578433748978));
#13966=CARTESIAN_POINT('Ctrl Pts',(1.02716612049091,3.05475512420929,13.0591700166121));
#13967=CARTESIAN_POINT('Ctrl Pts',(0.993869548144303,3.06569936934389,13.0613000960157));
#13968=CARTESIAN_POINT('Ctrl Pts',(0.98139518034783,3.06971542556511,13.0620990110482));
#13969=CARTESIAN_POINT('Ctrl Pts',(0.95928224087124,3.07668600449792,13.0635169452393));
#13970=CARTESIAN_POINT('Ctrl Pts',(0.94965359443676,3.07967161152451,13.0641349313674));
#13971=CARTESIAN_POINT('Ctrl Pts',(0.929639846959014,3.08577460037859,13.0654207142771));
#13972=CARTESIAN_POINT('Ctrl Pts',(0.919252717725339,3.08888484177537,13.0660887365144));
#13973=CARTESIAN_POINT('Ctrl Pts',(0.892398724783401,3.09677834432983,13.0678176877604));
#13974=CARTESIAN_POINT('Ctrl Pts',(0.875909188204659,3.10148265731174,13.0688811833354));
#13975=CARTESIAN_POINT('Ctrl Pts',(0.80553621599143,3.12095344735486,13.073428263993));
#13976=CARTESIAN_POINT('Ctrl Pts',(0.751313908730492,3.13444824425033,13.0769528260938));
#13977=CARTESIAN_POINT('Ctrl Pts',(0.607519783942016,3.16629020183804,13.0863608591637));
#13978=CARTESIAN_POINT('Ctrl Pts',(0.517475562756523,3.1822461390512,13.092315063787));
#13979=CARTESIAN_POINT('Ctrl Pts',(0.181828556465332,3.22710074705305,13.1147111154533));
#13980=CARTESIAN_POINT('Ctrl Pts',(-0.0661520216945494,3.23153973885737,
13.1317283138849));
#13981=CARTESIAN_POINT('Ctrl Pts',(-0.400370352298577,3.19901090298698,
13.1540405549022));
#13982=CARTESIAN_POINT('Ctrl Pts',(-0.488169418444432,3.18679476766393,
13.1598327232073));
#13983=CARTESIAN_POINT('Ctrl Pts',(-0.588947421548988,3.16850898024592,
13.1663194270417));
#13984=CARTESIAN_POINT('Ctrl Pts',(-0.60251788651561,3.16595648039392,13.1671894676034));
#13985=CARTESIAN_POINT('Ctrl Pts',(-0.6229908642707,3.161969265294,13.168496414642));
#13986=CARTESIAN_POINT('Ctrl Pts',(-0.629905557544051,3.16059903221658,
13.1689368594266));
#13987=CARTESIAN_POINT('Ctrl Pts',(-0.642284943777616,3.15810366211542,
13.169723575349));
#13988=CARTESIAN_POINT('Ctrl Pts',(-0.647751239821438,3.15698701652705,
13.1700703225124));
#13989=CARTESIAN_POINT('Ctrl Pts',(-0.65960229246785,3.15453402693439,13.1708206840841));
#13990=CARTESIAN_POINT('Ctrl Pts',(-0.665985880647245,3.15319249648276,
13.1712239972947));
#13991=CARTESIAN_POINT('Ctrl Pts',(-0.68386075064628,3.14937933447135,13.1723509983891));
#13992=CARTESIAN_POINT('Ctrl Pts',(-0.695342787437986,3.14686417510242,
13.1730722354391));
#13993=CARTESIAN_POINT('Ctrl Pts',(-0.763125691563052,3.13162710701117,
13.1773153860123));
#13994=CARTESIAN_POINT('Ctrl Pts',(-0.819094224153468,3.11745645817755,
13.1807594064041));
#13995=CARTESIAN_POINT('Ctrl Pts',(-1.11807584950103,3.03314833711307,13.1989827462395));
#13996=CARTESIAN_POINT('Ctrl Pts',(-1.35259168286045,2.93608661492708,13.212710164885));
#13997=CARTESIAN_POINT('Ctrl Pts',(-1.7159561714079,2.73282052353992,13.2362306927792));
#13998=CARTESIAN_POINT('Ctrl Pts',(-1.85225995471956,2.64233538428435,13.2456473779133));
#13999=CARTESIAN_POINT('Ctrl Pts',(-1.99837559765314,2.5284564246973,13.2567898231132));
#14000=CARTESIAN_POINT('Ctrl Pts',(-2.01550655745929,2.51482210136046,13.2581134405736));
#14001=CARTESIAN_POINT('Ctrl Pts',(-2.04265555215683,2.49275895538259,13.2602395799217));
#14002=CARTESIAN_POINT('Ctrl Pts',(-2.05276364388935,2.48444165332742,13.2610376058395));
#14003=CARTESIAN_POINT('Ctrl Pts',(-2.07056414831487,2.46961196320611,13.2624545108718));
#14004=CARTESIAN_POINT('Ctrl Pts',(-2.07827725280712,2.46312460056263,13.2630723619367));
#14005=CARTESIAN_POINT('Ctrl Pts',(-2.0942297717035,2.44957892952702,13.2643584111904));
#14006=CARTESIAN_POINT('Ctrl Pts',(-2.10246421739755,2.44251499046088,13.2650268375547));
#14007=CARTESIAN_POINT('Ctrl Pts',(-2.12364300702489,2.42416026231451,13.2667580111607));
#14008=CARTESIAN_POINT('Ctrl Pts',(-2.1365329057906,2.41280743589956,13.2678233375172));
#14009=CARTESIAN_POINT('Ctrl Pts',(-2.19115875263822,2.36391455179486,13.2723888584959));
#14010=CARTESIAN_POINT('Ctrl Pts',(-2.23199868794235,2.32539241957981,13.2759304447597));
#14011=CARTESIAN_POINT('Ctrl Pts',(-2.33707735928795,2.22095803410522,13.2853954695223));
#14012=CARTESIAN_POINT('Ctrl Pts',(-2.39953127467968,2.15333051479323,13.2913907120885));
#14013=CARTESIAN_POINT('Ctrl Pts',(-2.61529386198287,1.89863637644144,13.3134736964007));
#14014=CARTESIAN_POINT('Ctrl Pts',(-2.75031097836682,1.69716138434015,13.3301016764129));
#14015=CARTESIAN_POINT('Ctrl Pts',(-2.90423618238228,1.40005384004871,13.3523702712656));
#14016=CARTESIAN_POINT('Ctrl Pts',(-2.94336952550922,1.31579553520197,13.3584499966489));
#14017=CARTESIAN_POINT('Ctrl Pts',(-2.9841383347074,1.2170582155401,13.3652165204361));
#14018=CARTESIAN_POINT('Ctrl Pts',(-2.98938046256159,1.20412489689205,13.3660959289163));
#14019=CARTESIAN_POINT('Ctrl Pts',(-2.99715551093824,1.18457863310282,13.3674141418255));
#14020=CARTESIAN_POINT('Ctrl Pts',(-2.99975083732108,1.17799092144918,13.3678565739394));
#14021=CARTESIAN_POINT('Ctrl Pts',(-3.00435321270779,1.16619487613558,13.3686454296903));
#14022=CARTESIAN_POINT('Ctrl Pts',(-3.00636845474568,1.16098984996485,13.3689923404721));
#14023=CARTESIAN_POINT('Ctrl Pts',(-3.0107012684395,1.14971199999952,13.3697414534169));
#14024=CARTESIAN_POINT('Ctrl Pts',(-3.01301398687422,1.14363741080339,13.3701433630243));
#14025=CARTESIAN_POINT('Ctrl Pts',(-3.01941982053713,1.12665752850819,13.371262483001));
#14026=CARTESIAN_POINT('Ctrl Pts',(-3.02347226392441,1.11573684985899,13.3719772975185));
#14027=CARTESIAN_POINT('Ctrl Pts',(-3.04664464720478,1.05223761393905,13.3761062909239));
#14028=CARTESIAN_POINT('Ctrl Pts',(-3.06445335346116,0.999186731959985,
13.379447381951));
#14029=CARTESIAN_POINT('Ctrl Pts',(-3.15546951366754,0.702675608467921,
13.397664270947));
#14030=CARTESIAN_POINT('Ctrl Pts',(-3.20105776246953,0.451660785888588,
13.411459238772));
#14031=CARTESIAN_POINT('Ctrl Pts',(-3.226741044131,0.0341526453691606,13.4350857161843));
#14032=CARTESIAN_POINT('Ctrl Pts',(-3.22429731215423,-0.13007899355528,
13.4445375580286));
#14033=CARTESIAN_POINT('Ctrl Pts',(-3.20737233354436,-0.315214528777687,
13.4557193283967));
#14034=CARTESIAN_POINT('Ctrl Pts',(-3.20515555615476,-0.337009361427066,
13.4570437139644));
#14035=CARTESIAN_POINT('Ctrl Pts',(-3.20125908316678,-0.371792005362685,
13.4591708540761));
#14036=CARTESIAN_POINT('Ctrl Pts',(-3.19972210333762,-0.384795356365263,
13.4599691058792));
#14037=CARTESIAN_POINT('Ctrl Pts',(-3.19686184889068,-0.407790966154418,
13.4613862723029));
#14038=CARTESIAN_POINT('Ctrl Pts',(-3.19557085247388,-0.41778711818746,
13.4620041576086));
#14039=CARTESIAN_POINT('Ctrl Pts',(-3.1927931209413,-0.438528585214108,
13.4632901388356));
#14040=CARTESIAN_POINT('Ctrl Pts',(-3.19129898494474,-0.449272764881063,
13.4639584622399));
#14041=CARTESIAN_POINT('Ctrl Pts',(-3.18729995129729,-0.477002478016162,
13.4656890697067));
#14042=CARTESIAN_POINT('Ctrl Pts',(-3.18471353451077,-0.493975736538595,
13.466753929685));
#14043=CARTESIAN_POINT('Ctrl Pts',(-3.17310287998171,-0.566285454392075,
13.4713147460004));
#14044=CARTESIAN_POINT('Ctrl Pts',(-3.16277148365997,-0.621399233831103,
13.4748519879831));
#14045=CARTESIAN_POINT('Ctrl Pts',(-3.13173288046499,-0.766032537866834,
13.4843024573245));
#14046=CARTESIAN_POINT('Ctrl Pts',(-3.10862736737544,-0.854979565707767,
13.4902872144924));
#14047=CARTESIAN_POINT('Ctrl Pts',(-3.01055241267302,-1.17555576173496,
13.512463997259));
#14048=CARTESIAN_POINT('Ctrl Pts',(-2.91322060300083,-1.39945983489746,
13.5292063073026));
#14049=CARTESIAN_POINT('Ctrl Pts',(-2.74587375349919,-1.68957946321284,
13.5514852062674));
#14050=CARTESIAN_POINT('Ctrl Pts',(-2.69675930457981,-1.76691653965921,
13.5574778785254));
#14051=CARTESIAN_POINT('Ctrl Pts',(-2.63646091979439,-1.85347914125896,
13.5641598756857));
#14052=CARTESIAN_POINT('Ctrl Pts',(-2.62843502575435,-1.86484327505048,
13.5650365556203));
#14053=CARTESIAN_POINT('Ctrl Pts',(-2.61621900121881,-1.88190480720376,
13.5663514883278));
#14054=CARTESIAN_POINT('Ctrl Pts',(-2.61208341909765,-1.8876407973064,13.5667933426496));
#14055=CARTESIAN_POINT('Ctrl Pts',(-2.60465021961238,-1.89787932742662,
13.5675815750426));
#14056=CARTESIAN_POINT('Ctrl Pts',(-2.60135976719143,-1.9023869404529,13.5679284370278));
#14057=CARTESIAN_POINT('Ctrl Pts',(-2.59420767441188,-1.91213138646455,
13.5686779073967));
#14058=CARTESIAN_POINT('Ctrl Pts',(-2.59034189091565,-1.91736506357444,
13.5690802207338));
#14059=CARTESIAN_POINT('Ctrl Pts',(-2.57949324415851,-1.93195976996552,
13.5702016059116));
#14060=CARTESIAN_POINT('Ctrl Pts',(-2.5724752253207,-1.94129471597344,13.5709182661558));
#14061=CARTESIAN_POINT('Ctrl Pts',(-2.53124006064151,-1.99552696332442,
13.5750796493784));
#14062=CARTESIAN_POINT('Ctrl Pts',(-2.49589644752285,-2.0395602294932,13.5784499375394));
#14063=CARTESIAN_POINT('Ctrl Pts',(-2.29537316687291,-2.2763597204278,13.596668358589));
#14064=CARTESIAN_POINT('Ctrl Pts',(-2.10900786186528,-2.45003357393953,
13.6104439451503));
#14065=CARTESIAN_POINT('Ctrl Pts',(-1.77204017750306,-2.69681563626451,
13.6340360711576));
#14066=CARTESIAN_POINT('Ctrl Pts',(-1.63274012608523,-2.78335952069482,
13.643473722262));
#14067=CARTESIAN_POINT('Ctrl Pts',(-1.48340867397894,-2.86105528026574,
13.6535982023777));
#14068=CARTESIAN_POINT('Ctrl Pts',(-1.47933426699413,-2.86316411275432,
13.6538744332376));
#14069=CARTESIAN_POINT('Ctrl Pts',(-1.4752554049854,-2.86526422037504,13.6541509617524));
#14070=CARTESIAN_POINT('Origin',(0.,0.,4.68922655072688));
#14071=CARTESIAN_POINT('',(-1.47525540626678,-2.86526421971528,15.1508554073139));
#14072=CARTESIAN_POINT('',(-1.47525516809587,-2.86526434234373,14.9065719799118));
#14073=CARTESIAN_POINT('',(-1.47525540501186,-2.86526422036142,4.68922655072688));
#14074=CARTESIAN_POINT('Ctrl Pts',(-1.47525540626678,-2.86526421971528,
15.1508554073139));
#14075=CARTESIAN_POINT('Ctrl Pts',(-1.50339105412724,-2.85077785356121,
15.1488133657421));
#14076=CARTESIAN_POINT('Ctrl Pts',(-1.53131412858722,-2.83587665466912,
15.1467909671531));
#14077=CARTESIAN_POINT('Ctrl Pts',(-1.56922412136404,-2.81492260591201,
15.1440556586238));
#14078=CARTESIAN_POINT('Ctrl Pts',(-1.57940231774181,-2.80922443903595,
15.1433223176556));
#14079=CARTESIAN_POINT('Ctrl Pts',(-1.59520807439074,-2.80026267955658,
15.1421854088157));
#14080=CARTESIAN_POINT('Ctrl Pts',(-1.60085694755529,-2.79703716642421,
15.1417794653858));
#14081=CARTESIAN_POINT('Ctrl Pts',(-1.61133619693371,-2.79101135716602,
15.1410271619145));
#14082=CARTESIAN_POINT('Ctrl Pts',(-1.61616901541381,-2.78821563902556,
15.1406805245355));
#14083=CARTESIAN_POINT('Ctrl Pts',(-1.6271133574999,-2.78184647353503,15.1398962141376));
#14084=CARTESIAN_POINT('Ctrl Pts',(-1.63322037227713,-2.77826544777702,
15.1394590402937));
#14085=CARTESIAN_POINT('Ctrl Pts',(-1.65132034225001,-2.76757169884925,
15.1381646104348));
#14086=CARTESIAN_POINT('Ctrl Pts',(-1.66327917396285,-2.7604011278715,15.1373110245124));
#14087=CARTESIAN_POINT('Ctrl Pts',(-1.75411951229551,-2.70512815644969,
15.1308368158665));
#14088=CARTESIAN_POINT('Ctrl Pts',(-1.8309541822147,-2.6537264037884,15.1254165093946));
#14089=CARTESIAN_POINT('Ctrl Pts',(-2.10092552907359,-2.45580118795912,
15.1061741392801));
#14090=CARTESIAN_POINT('Ctrl Pts',(-2.27959126223985,-2.29092211366912,
15.0929979577751));
#14091=CARTESIAN_POINT('Ctrl Pts',(-2.49822154229909,-2.03800410913888,
15.0739653603523));
#14092=CARTESIAN_POINT('Ctrl Pts',(-2.55534259492575,-1.96590791113413,
15.0686583249957));
#14093=CARTESIAN_POINT('Ctrl Pts',(-2.64223063083345,-1.84604519517854,
15.0599287925599));
#14094=CARTESIAN_POINT('Ctrl Pts',(-2.67396703037729,-1.79976812756134,
15.0565798320844));
#14095=CARTESIAN_POINT('Ctrl Pts',(-2.71381987443033,-1.73827337098048,
15.0521454975276));
#14096=CARTESIAN_POINT('Ctrl Pts',(-2.7230462002902,-1.72378420819638,15.0511018392976));
#14097=CARTESIAN_POINT('Ctrl Pts',(-2.73791153667383,-1.70002227725716,
15.0493917982837));
#14098=CARTESIAN_POINT('Ctrl Pts',(-2.74362039425488,-1.6907934390385,15.0487280143001));
#14099=CARTESIAN_POINT('Ctrl Pts',(-2.75454327758538,-1.67293471275003,
15.0474441623079));
#14100=CARTESIAN_POINT('Ctrl Pts',(-2.75976363640794,-1.66430883212461,
15.0468243374637));
#14101=CARTESIAN_POINT('Ctrl Pts',(-2.77167210792768,-1.64442173216434,
15.0453959003581));
#14102=CARTESIAN_POINT('Ctrl Pts',(-2.77833218598325,-1.63314401179675,
15.0445862750852));
#14103=CARTESIAN_POINT('Ctrl Pts',(-2.79595006120658,-1.60289142846693,
15.0424154126279));
#14104=CARTESIAN_POINT('Ctrl Pts',(-2.80678324777666,-1.58384514328681,
15.0410496931151));
#14105=CARTESIAN_POINT('Ctrl Pts',(-2.89705248471956,-1.42130405278582,
15.0294011727022));
#14106=CARTESIAN_POINT('Ctrl Pts',(-2.96560938703671,-1.27207096805266,
15.0187303653674));
#14107=CARTESIAN_POINT('Ctrl Pts',(-3.11082541207775,-0.879581921124254,
14.9908172214239));
#14108=CARTESIAN_POINT('Ctrl Pts',(-3.17055178420517,-0.631265207656641,
14.973246866533));
#14109=CARTESIAN_POINT('Ctrl Pts',(-3.20698716349528,-0.323193508378476,
14.9529593616129));
#14110=CARTESIAN_POINT('Ctrl Pts',(-3.21209489830478,-0.267708730078014,
14.9493679436506));
#14111=CARTESIAN_POINT('Ctrl Pts',(-3.21652775534488,-0.200504765022391,
14.9451150615929));
#14112=CARTESIAN_POINT('Ctrl Pts',(-3.21723074828495,-0.188889607286423,
14.9443835186858));
#14113=CARTESIAN_POINT('Ctrl Pts',(-3.21822829277222,-0.170781879985132,
14.9432487846746));
#14114=CARTESIAN_POINT('Ctrl Pts',(-3.21856613362683,-0.164291935809402,
14.9428432323927));
#14115=CARTESIAN_POINT('Ctrl Pts',(-3.21915776009772,-0.152223711706366,
14.9420912812633));
#14116=CARTESIAN_POINT('Ctrl Pts',(-3.21941667674598,-0.146645848885181,
14.9417446074122));
#14117=CARTESIAN_POINT('Ctrl Pts',(-3.21997135556272,-0.13398608289893,
14.9409597395251));
#14118=CARTESIAN_POINT('Ctrl Pts',(-3.22025825199285,-0.126903876196469,
14.9405220476225));
#14119=CARTESIAN_POINT('Ctrl Pts',(-3.221041680693,-0.105847003915736,14.9392246596969));
#14120=CARTESIAN_POINT('Ctrl Pts',(-3.22147063581203,-0.0918697775634275,
14.9383686586757));
#14121=CARTESIAN_POINT('Ctrl Pts',(-3.22407146658485,0.0157099974861362,
14.9318170610924));
#14122=CARTESIAN_POINT('Ctrl Pts',(-3.22225457462109,0.109373870880423,
14.9263272341586));
#14123=CARTESIAN_POINT('Ctrl Pts',(-3.20120368336465,0.44317932895907,14.9071124929251));
#14124=CARTESIAN_POINT('Ctrl Pts',(-3.15915526917128,0.681075111207615,
14.894014257169));
#14125=CARTESIAN_POINT('Ctrl Pts',(-3.06493090883859,1.00039791195416,14.8750615227365));
#14126=CARTESIAN_POINT('Ctrl Pts',(-3.03509761190753,1.08755597849624,14.869746727306));
#14127=CARTESIAN_POINT('Ctrl Pts',(-2.98112607902476,1.2256262665161,14.8610055967566));
#14128=CARTESIAN_POINT('Ctrl Pts',(-2.95931365455275,1.27739365887942,14.8576530543894));
#14129=CARTESIAN_POINT('Ctrl Pts',(-2.92907662560662,1.34421835114289,14.8532146368152));
#14130=CARTESIAN_POINT('Ctrl Pts',(-2.9218675900796,1.3598171283211,14.8521705750905));
#14131=CARTESIAN_POINT('Ctrl Pts',(-2.90990241961235,1.38517264855677,14.8504600390333));
#14132=CARTESIAN_POINT('Ctrl Pts',(-2.90522107490098,1.39496446527128,14.8497961664049));
#14133=CARTESIAN_POINT('Ctrl Pts',(-2.89609583320821,1.41380625806437,14.8485122595942));
#14134=CARTESIAN_POINT('Ctrl Pts',(-2.8916587482981,1.42285940632668,14.8478924692038));
#14135=CARTESIAN_POINT('Ctrl Pts',(-2.88136149032117,1.44362217358492,14.846464278664));
#14136=CARTESIAN_POINT('Ctrl Pts',(-2.87547231665418,1.45531713588244,14.8456548666459));
#14137=CARTESIAN_POINT('Ctrl Pts',(-2.85954343532276,1.4864751955103,14.8434849478338));
#14138=CARTESIAN_POINT('Ctrl Pts',(-2.84937647052493,1.50587212483134,14.842119964833));
#14139=CARTESIAN_POINT('Ctrl Pts',(-2.76166897843788,1.66913507012453,14.8305088107152));
#14140=CARTESIAN_POINT('Ctrl Pts',(-2.67349814897883,1.80699211393752,14.8198775059535));
#14141=CARTESIAN_POINT('Ctrl Pts',(-2.42296518032278,2.13998406775255,14.7920872954272));
#14142=CARTESIAN_POINT('Ctrl Pts',(-2.24733465651383,2.32374137579747,14.7746028751454));
#14143=CARTESIAN_POINT('Ctrl Pts',(-2.00779899942243,2.52153668333864,14.7542691674285));
#14144=CARTESIAN_POINT('Ctrl Pts',(-1.96262438345589,2.55685560014849,14.7505705877408));
#14145=CARTESIAN_POINT('Ctrl Pts',(-1.90709491950525,2.59793075562248,14.7462085142417));
#14146=CARTESIAN_POINT('Ctrl Pts',(-1.89762328979931,2.60485721355607,14.7454707617328));
#14147=CARTESIAN_POINT('Ctrl Pts',(-1.88283009242172,2.61555174198484,14.7443285183764));
#14148=CARTESIAN_POINT('Ctrl Pts',(-1.87753467845655,2.61935557053818,14.743921616532));
#14149=CARTESIAN_POINT('Ctrl Pts',(-1.86768448521687,2.62638599253376,14.7431684447596));
#14150=CARTESIAN_POINT('Ctrl Pts',(-1.86313290980243,2.62961679323124,14.7428218917869));
#14151=CARTESIAN_POINT('Ctrl Pts',(-1.85280611240399,2.63690669147152,14.7420389248222));
#14152=CARTESIAN_POINT('Ctrl Pts',(-1.84702594869169,2.64095863973448,14.7416030028516));
#14153=CARTESIAN_POINT('Ctrl Pts',(-1.82986782707738,2.65290275715568,14.7403157077876));
#14154=CARTESIAN_POINT('Ctrl Pts',(-1.81845209451341,2.66074074261734,14.7394679450505));
#14155=CARTESIAN_POINT('Ctrl Pts',(-1.7328007421428,2.71873980476605,14.7331691478427));
#14156=CARTESIAN_POINT('Ctrl Pts',(-1.65654543491967,2.76586422762953,14.7279063671988));
#14157=CARTESIAN_POINT('Ctrl Pts',(-1.36402972012538,2.93018900306362,14.7085940471418));
#14158=CARTESIAN_POINT('Ctrl Pts',(-1.13655495339117,3.02569688703108,14.6952357524548));
#14159=CARTESIAN_POINT('Ctrl Pts',(-0.812507264135596,3.11998917228078,
14.6760190515784));
#14160=CARTESIAN_POINT('Ctrl Pts',(-0.723550771799499,3.14181044292119,
14.6707334484948));
#14161=CARTESIAN_POINT('Ctrl Pts',(-0.578945280369275,3.17081518860871,
14.6620359581591));
#14162=CARTESIAN_POINT('Ctrl Pts',(-0.523825492131568,3.18038564959663,
14.6586969026522));
#14163=CARTESIAN_POINT('Ctrl Pts',(-0.451510534592544,3.19101084617937,
14.6542738603294));
#14164=CARTESIAN_POINT('Ctrl Pts',(-0.434514719841401,3.1933695250957,14.6532313200056));
#14165=CARTESIAN_POINT('Ctrl Pts',(-0.406744766683932,3.19699764334492,
14.6515226504859));
#14166=CARTESIAN_POINT('Ctrl Pts',(-0.395981480669193,3.19834862064699,
14.6508591120512));
#14167=CARTESIAN_POINT('Ctrl Pts',(-0.375199898331274,3.20085055687497,
14.6495754113896));
#14168=CARTESIAN_POINT('Ctrl Pts',(-0.365182604606776,3.20200888705172,
14.6489554905865));
#14169=CARTESIAN_POINT('Ctrl Pts',(-0.34213300609411,3.20456461332747,14.6475263680116));
#14170=CARTESIAN_POINT('Ctrl Pts',(-0.329097349809334,3.20592955023028,
14.646716150051));
#14171=CARTESIAN_POINT('Ctrl Pts',(-0.294215746842355,3.20936694571269,
14.6445426642336));
#14172=CARTESIAN_POINT('Ctrl Pts',(-0.272356650780918,3.21129583100458,
14.6431748970083));
#14173=CARTESIAN_POINT('Ctrl Pts',(-0.0853272305184408,3.2258763190808,
14.6314213156921));
#14174=CARTESIAN_POINT('Ctrl Pts',(0.0805460206602419,3.22599689259224,
14.6206393536959));
#14175=CARTESIAN_POINT('Ctrl Pts',(0.503473688447166,3.1936627652405,14.5923356825053));
#14176=CARTESIAN_POINT('Ctrl Pts',(0.757954184321514,3.14300323557174,14.5744755283569));
#14177=CARTESIAN_POINT('Ctrl Pts',(1.05171302553985,3.0467320410251,14.554318903552));
#14178=CARTESIAN_POINT('Ctrl Pts',(1.09940831273505,3.02984792670845,14.5510649552143));
#14179=CARTESIAN_POINT('Ctrl Pts',(1.15725380517517,3.00782462571468,14.5471582234709));
#14180=CARTESIAN_POINT('Ctrl Pts',(1.16779723625433,3.00374682232084,14.5464477858425));
#14181=CARTESIAN_POINT('Ctrl Pts',(1.18430019639621,2.99726406911535,14.5453386036452));
#14182=CARTESIAN_POINT('Ctrl Pts',(1.1902742387872,2.99489667491003,14.5449376639284));
#14183=CARTESIAN_POINT('Ctrl Pts',(1.2014349441305,2.99043523968144,14.5441897731953));
#14184=CARTESIAN_POINT('Ctrl Pts',(1.2066231782339,2.98834558812232,14.5438425749318));
#14185=CARTESIAN_POINT('Ctrl Pts',(1.21847190045648,2.9835374206574,14.5430507033294));
#14186=CARTESIAN_POINT('Ctrl Pts',(1.22512873213765,2.98081010879967,14.5426065688496));
#14187=CARTESIAN_POINT('Ctrl Pts',(1.24562891452724,2.97233088484343,14.5412409873636));
#14188=CARTESIAN_POINT('Ctrl Pts',(1.25944154235226,2.96650455978889,14.5403239331994));
#14189=CARTESIAN_POINT('Ctrl Pts',(1.40021749197162,2.90596314659321,14.5310037639977));
#14190=CARTESIAN_POINT('Ctrl Pts',(1.52359270871539,2.84322105364998,14.5230524076603));
#14191=CARTESIAN_POINT('Ctrl Pts',(1.81102563186235,2.67294592726262,14.5041794323046));
#14192=CARTESIAN_POINT('Ctrl Pts',(1.9700354429281,2.55801005983356,14.4934182845393));
#14193=CARTESIAN_POINT('Ctrl Pts',(2.18656143945151,2.3692674185386,14.4770617588059));
#14194=CARTESIAN_POINT('Ctrl Pts',(2.25289793568172,2.30628012515123,14.4717826406863));
#14195=CARTESIAN_POINT('Ctrl Pts',(2.3553176227157,2.20039081953556,14.4630948484355));
#14196=CARTESIAN_POINT('Ctrl Pts',(2.39311833593905,2.1592185907574,14.4597587935222));
#14197=CARTESIAN_POINT('Ctrl Pts',(2.44109605235173,2.104153476444,14.4553391724874));
#14198=CARTESIAN_POINT('Ctrl Pts',(2.45226060736853,2.09113119748398,14.4542969714381));
#14199=CARTESIAN_POINT('Ctrl Pts',(2.47031432354651,2.06973001926472,14.4525887181388));
#14200=CARTESIAN_POINT('Ctrl Pts',(2.4772661710729,2.06140425993392,14.4519252542121));
#14201=CARTESIAN_POINT('Ctrl Pts',(2.49060011213333,2.0452702368466,14.4506415993182));
#14202=CARTESIAN_POINT('Ctrl Pts',(2.49698785343683,2.03746678902714,14.4500216492459));
#14203=CARTESIAN_POINT('Ctrl Pts',(2.51159516002398,2.01945021786906,14.4485923179534));
#14204=CARTESIAN_POINT('Ctrl Pts',(2.5197891995872,2.00921671598342,14.447781919577));
#14205=CARTESIAN_POINT('Ctrl Pts',(2.54153746830639,1.98171310447695,14.4456076349857));
#14206=CARTESIAN_POINT('Ctrl Pts',(2.55497786207329,1.96435424937896,14.4442392442077));
#14207=CARTESIAN_POINT('Ctrl Pts',(2.66861553936937,1.81444680034196,14.4324533520043));
#14208=CARTESIAN_POINT('Ctrl Pts',(2.75858503908641,1.67449078483124,14.4216371797868));
#14209=CARTESIAN_POINT('Ctrl Pts',(2.96069130823641,1.29925766384464,14.3931936983065));
#14210=CARTESIAN_POINT('Ctrl Pts',(3.05584877054075,1.05619525443937,14.375223223154));
#14211=CARTESIAN_POINT('Ctrl Pts',(3.13293175692409,0.75712231556495,14.3551072395965));
#14212=CARTESIAN_POINT('Ctrl Pts',(3.1440301257356,0.709627208834215,14.3519729341825));
#14213=CARTESIAN_POINT('Ctrl Pts',(3.15634241069869,0.650957041462287,14.3481898157189));
#14214=CARTESIAN_POINT('Ctrl Pts',(3.15858104788213,0.640006449990388,14.347487481503));
#14215=CARTESIAN_POINT('Ctrl Pts',(3.16201150077367,0.622769431052952,14.3463881211525));
#14216=CARTESIAN_POINT('Ctrl Pts',(3.16324161783913,0.616490846762013,14.3459889622682));
#14217=CARTESIAN_POINT('Ctrl Pts',(3.16551294518215,0.604712073078155,14.345242588961));
#14218=CARTESIAN_POINT('Ctrl Pts',(3.16655851047992,0.599212898481066,14.344895138132));
#14219=CARTESIAN_POINT('Ctrl Pts',(3.16892310176718,0.586597237913914,14.3441003339719));
#14220=CARTESIAN_POINT('Ctrl Pts',(3.17023248466124,0.57947902468446,14.343653534667));
#14221=CARTESIAN_POINT('Ctrl Pts',(3.17360635588108,0.560783866688975,14.3424842743218));
#14222=CARTESIAN_POINT('Ctrl Pts',(3.17563150121193,0.549199804760954,14.3417639941961));
#14223=CARTESIAN_POINT('Ctrl Pts',(3.18900098468622,0.470177468897702,14.3368776879659));
#14224=CARTESIAN_POINT('Ctrl Pts',(3.19826062185061,0.402398617924862,14.3328213043519));
#14225=CARTESIAN_POINT('Ctrl Pts',(3.21684428002505,0.224251511214762,14.3223912062999));
#14226=CARTESIAN_POINT('Ctrl Pts',(3.2226499711397,0.113605529013144,14.3161424827816));
#14227=CARTESIAN_POINT('Ctrl Pts',(3.22299534989345,-0.273689037745909,
14.2944381621487));
#14228=CARTESIAN_POINT('Ctrl Pts',(3.18764473413559,-0.549099614211858,
14.2791890572757));
#14229=CARTESIAN_POINT('Ctrl Pts',(3.10884493051252,-0.849933776056677,
14.2606250515512));
#14230=CARTESIAN_POINT('Ctrl Pts',(3.09958271938353,-0.883114405255533,
14.2585524761388));
#14231=CARTESIAN_POINT('Ctrl Pts',(3.08603519401101,-0.928805076754244,
14.2556611436774));
#14232=CARTESIAN_POINT('Ctrl Pts',(3.08220190956416,-0.941447539609258,
14.2548571375493));
#14233=CARTESIAN_POINT('Ctrl Pts',(3.07547746808638,-0.963143931143572,
14.253470330583));
#14234=CARTESIAN_POINT('Ctrl Pts',(3.07262377140076,-0.972209362825783,
14.2528887652637));
#14235=CARTESIAN_POINT('Ctrl Pts',(3.0666559576345,-0.990878768031159,14.2516866607862));
#14236=CARTESIAN_POINT('Ctrl Pts',(3.06353672878398,-1.00048098588582,14.251065958442));
#14237=CARTESIAN_POINT('Ctrl Pts',(3.05616870473473,-1.02280511766972,14.249617163114));
#14238=CARTESIAN_POINT('Ctrl Pts',(3.0518855303556,-1.03551540857386,14.2487879392545));
#14239=CARTESIAN_POINT('Ctrl Pts',(3.03789943316742,-1.07617846807766,14.2461208861781));
#14240=CARTESIAN_POINT('Ctrl Pts',(3.02789106684941,-1.10402384674811,14.2442729442098));
#14241=CARTESIAN_POINT('Ctrl Pts',(2.97572489536693,-1.24311349402467,14.2349308282727));
#14242=CARTESIAN_POINT('Ctrl Pts',(2.92781828379777,-1.35208881722406,14.2272454491624));
#14243=CARTESIAN_POINT('Ctrl Pts',(2.76831963433682,-1.66645801582727,14.2039853799899));
#14244=CARTESIAN_POINT('Ctrl Pts',(2.64030524265051,-1.86264539643857,14.1879612020676));
#14245=CARTESIAN_POINT('Ctrl Pts',(2.47296104969265,-2.06676210755497,14.1703051787076));
#14246=CARTESIAN_POINT('Ctrl Pts',(2.45335248969851,-2.09000086301943,14.1682801521482));
#14247=CARTESIAN_POINT('Ctrl Pts',(2.41701406412699,-2.13185049537101,14.1646106264563));
#14248=CARTESIAN_POINT('Ctrl Pts',(2.40039070634963,-2.15055063593615,14.1629623828965));
#14249=CARTESIAN_POINT('Ctrl Pts',(2.34532669873475,-2.21105985284406,14.1576058036567));
#14250=CARTESIAN_POINT('Ctrl Pts',(2.3059960170692,-2.25204935512446,14.1539400791037));
#14251=CARTESIAN_POINT('Ctrl Pts',(2.2576932531644,-2.29979615008754,14.1496473403914));
#14252=CARTESIAN_POINT('Ctrl Pts',(2.24974622524655,-2.3075708196659,14.1489476063431));
#14253=CARTESIAN_POINT('Ctrl Pts',(2.23669897287542,-2.32020362770557,14.1478096559964));
#14254=CARTESIAN_POINT('Ctrl Pts',(2.23162285122013,-2.32508636859612,14.1473695828788));
#14255=CARTESIAN_POINT('Ctrl Pts',(2.22249613133527,-2.33380797223854,14.1465831549406));
#14256=CARTESIAN_POINT('Ctrl Pts',(2.21845154903182,-2.33765297493322,14.1462363267225));
#14257=CARTESIAN_POINT('Ctrl Pts',(2.20965136206051,-2.34597550766676,14.145485352874));
#14258=CARTESIAN_POINT('Ctrl Pts',(2.20489214134958,-2.35044907862963,14.1450815110214));
#14259=CARTESIAN_POINT('Ctrl Pts',(2.19150605257617,-2.36295529536825,14.143951935974));
#14260=CARTESIAN_POINT('Ctrl Pts',(2.18284856247672,-2.37095522304369,14.1432286706289));
#14261=CARTESIAN_POINT('Ctrl Pts',(2.13115289384639,-2.41820127563144,14.1389515972645));
#14262=CARTESIAN_POINT('Ctrl Pts',(2.08709807058008,-2.45632503810693,14.1354771312879));
#14263=CARTESIAN_POINT('Ctrl Pts',(1.84658336666752,-2.65331337390348,14.1172456147136));
#14264=CARTESIAN_POINT('Ctrl Pts',(1.63297405866927,-2.78986807681687,14.1035328353902));
#14265=CARTESIAN_POINT('Ctrl Pts',(1.2588326929012,-2.97120411423322,14.0800435652225));
#14266=CARTESIAN_POINT('Ctrl Pts',(1.10690998547183,-3.03108125812217,14.0706436644758));
#14267=CARTESIAN_POINT('Ctrl Pts',(0.930203326758145,-3.0856634037397,14.0595196947244));
#14268=CARTESIAN_POINT('Ctrl Pts',(0.909220502564736,-3.09191120696827,
14.0581961468508));
#14269=CARTESIAN_POINT('Ctrl Pts',(0.875590912336023,-3.1015527596343,14.0560699568057));
#14270=CARTESIAN_POINT('Ctrl Pts',(0.862984064630332,-3.10508413135876,
14.0552718091158));
#14271=CARTESIAN_POINT('Ctrl Pts',(0.840631727694044,-3.11119872439373,
14.0538545893563));
#14272=CARTESIAN_POINT('Ctrl Pts',(0.830894921563278,-3.11381322977578,
14.0532365451839));
#14273=CARTESIAN_POINT('Ctrl Pts',(0.810650124066179,-3.11914760037152,
14.0519499948551));
#14274=CARTESIAN_POINT('Ctrl Pts',(0.800140352792831,-3.12186014865646,
14.051281259878));
#14275=CARTESIAN_POINT('Ctrl Pts',(0.772953131985983,-3.12873080395834,
14.0495490714257));
#14276=CARTESIAN_POINT('Ctrl Pts',(0.756255926453349,-3.13280863493769,
14.0484830347467));
#14277=CARTESIAN_POINT('Ctrl Pts',(0.684822972502983,-3.14964981285136,
14.0439124609492));
#14278=CARTESIAN_POINT('Ctrl Pts',(0.629793767883843,-3.16111303426801,
14.0403664257195));
#14279=CARTESIAN_POINT('Ctrl Pts',(0.483802916525641,-3.18756136045126,
14.0308870724698));
#14280=CARTESIAN_POINT('Ctrl Pts',(0.392454608034174,-3.20009211266829,
14.0248816930956));
#14281=CARTESIAN_POINT('Ctrl Pts',(0.061812681645723,-3.23107811296798,
14.0029101681072));
#14282=CARTESIAN_POINT('Ctrl Pts',(-0.17880385919135,-3.22671678130447,
13.9864151868103));
#14283=CARTESIAN_POINT('Ctrl Pts',(-0.449124598487464,-3.19146897361022,
13.9682630291823));
#14284=CARTESIAN_POINT('Ctrl Pts',(-0.481488776943131,-3.18674689824832,
13.9660974044244));
#14285=CARTESIAN_POINT('Ctrl Pts',(-0.576888542331726,-3.17134107187992,
13.9597462659715));
#14286=CARTESIAN_POINT('Ctrl Pts',(-0.639688666443664,-3.15927274637982,
13.9556073485603));
#14287=CARTESIAN_POINT('Ctrl Pts',(-0.713345063924788,-3.14283141511242,
13.9508346094893));
#14288=CARTESIAN_POINT('Ctrl Pts',(-0.724583947499703,-3.14025931993832,
13.9501086301054));
#14289=CARTESIAN_POINT('Ctrl Pts',(-0.742787878807237,-3.13599029225939,
13.9489366974488));
#14290=CARTESIAN_POINT('Ctrl Pts',(-0.749761375311988,-3.13433036364961,
13.9484887018967));
#14291=CARTESIAN_POINT('Ctrl Pts',(-0.762163854812354,-3.13133439256682,
13.9476936880605));
#14292=CARTESIAN_POINT('Ctrl Pts',(-0.767594945071087,-3.13000747948518,
13.94734615211));
#14293=CARTESIAN_POINT('Ctrl Pts',(-0.779277423167552,-3.12712100345797,
13.9465999023303));
#14294=CARTESIAN_POINT('Ctrl Pts',(-0.785527577890505,-3.12555683016938,
13.9462014587759));
#14295=CARTESIAN_POINT('Ctrl Pts',(-0.802805350278876,-3.12117776837382,
13.9451021249343));
#14296=CARTESIAN_POINT('Ctrl Pts',(-0.813822939122415,-3.11832315916913,
13.9444034939246));
#14297=CARTESIAN_POINT('Ctrl Pts',(-0.874823074406389,-3.10217297163409,
13.9405475117798));
#14298=CARTESIAN_POINT('Ctrl Pts',(-0.924498214031703,-3.08773320005452,
13.937452402517));
#14299=CARTESIAN_POINT('Ctrl Pts',(-1.14658871042072,-3.0173340724577,13.9237293053963));
#14300=CARTESIAN_POINT('Ctrl Pts',(-1.31432418387146,-2.94812382759616,
13.9136660899074));
#14301=CARTESIAN_POINT('Ctrl Pts',(-1.47525547426939,-2.86526418470238,
13.9035519756546));
#14302=CARTESIAN_POINT('',(3.22274997771073,0.000379032282113146,14.0611576755349));
#14303=CARTESIAN_POINT('Ctrl Pts',(-1.4752554049854,-2.86526422037504,13.6541509617524));
#14304=CARTESIAN_POINT('Ctrl Pts',(-1.45982376353312,-2.87320960017575,
13.6551971576971));
#14305=CARTESIAN_POINT('Ctrl Pts',(-1.44432835518962,-2.88103009647269,
13.6562476163241));
#14306=CARTESIAN_POINT('Ctrl Pts',(-1.4170239894115,-2.89453490501609,13.6580988942635));
#14307=CARTESIAN_POINT('Ctrl Pts',(-1.40524210014484,-2.90027307937424,
13.6588978115895));
#14308=CARTESIAN_POINT('Ctrl Pts',(-1.38433572830802,-2.91029788498968,
13.6603157484364));
#14309=CARTESIAN_POINT('Ctrl Pts',(-1.37522546321132,-2.91461388690045,
13.6609337349139));
#14310=CARTESIAN_POINT('Ctrl Pts',(-1.35627470346765,-2.92348320634336,
13.6622195171418));
#14311=CARTESIAN_POINT('Ctrl Pts',(-1.34643119226503,-2.92802974181157,
13.6628875383409));
#14312=CARTESIAN_POINT('Ctrl Pts',(-1.32096183568928,-2.93963797498741,
13.6646164838761));
#14313=CARTESIAN_POINT('Ctrl Pts',(-1.30530239145358,-2.9466247205715,13.6656799747465));
#14314=CARTESIAN_POINT('Ctrl Pts',(-1.2383868216666,-2.97584223705724,13.6702270081124));
#14315=CARTESIAN_POINT('Ctrl Pts',(-1.18661557317988,-2.99686199064071,
13.6737515265658));
#14316=CARTESIAN_POINT('Ctrl Pts',(-1.04876452882735,-3.04869916675506,
13.6831594136804));
#14317=CARTESIAN_POINT('Ctrl Pts',(-0.961879264632453,-3.07721618416813,
13.6891135132665));
#14318=CARTESIAN_POINT('Ctrl Pts',(-0.635926831564798,-3.16904457231667,
13.7115101920212));
#14319=CARTESIAN_POINT('Ctrl Pts',(-0.391049363940187,-3.20847489434767,
13.728528198626));
#14320=CARTESIAN_POINT('Ctrl Pts',(-0.055584648732851,-3.2234881789726,
13.7508405620566));
#14321=CARTESIAN_POINT('Ctrl Pts',(0.0330512780081772,-3.22379844303205,
13.756632164867));
#14322=CARTESIAN_POINT('Ctrl Pts',(0.135393188527221,-3.21993430046902,
13.7631183166994));
#14323=CARTESIAN_POINT('Ctrl Pts',(0.14918785022229,-3.21932465219847,13.7639883378338));
#14324=CARTESIAN_POINT('Ctrl Pts',(0.170018421978332,-3.21826987477703,
13.7652952614974));
#14325=CARTESIAN_POINT('Ctrl Pts',(0.177057280142272,-3.21789029839468,
13.7657357021501));
#14326=CARTESIAN_POINT('Ctrl Pts',(0.189664973434262,-3.21716892429825,
13.7665224136363));
#14327=CARTESIAN_POINT('Ctrl Pts',(0.195234195864137,-3.2168357589289,13.7668691604721));
#14328=CARTESIAN_POINT('Ctrl Pts',(0.207312981135927,-3.21608169047428,
13.7676195246972));
#14329=CARTESIAN_POINT('Ctrl Pts',(0.213822119996184,-3.215655487569,13.7680228408706));
#14330=CARTESIAN_POINT('Ctrl Pts',(0.23205669507289,-3.21440591932724,13.7691498586185));
#14331=CARTESIAN_POINT('Ctrl Pts',(0.243779128463169,-3.21353815449199,
13.7698711092424));
#14332=CARTESIAN_POINT('Ctrl Pts',(0.313038872103603,-3.20802996619662,
13.7741145054594));
#14333=CARTESIAN_POINT('Ctrl Pts',(0.370451841367153,-3.20190817967215,
13.7775587474066));
#14334=CARTESIAN_POINT('Ctrl Pts',(0.678346550880745,-3.16068457878031,
13.7957821042646));
#14335=CARTESIAN_POINT('Ctrl Pts',(0.924220157790897,-3.09772893879346,
13.8095093798324));
#14336=CARTESIAN_POINT('Ctrl Pts',(1.31258679528047,-2.94786460392411,13.8330256491715));
#14337=CARTESIAN_POINT('Ctrl Pts',(1.46024347612413,-2.87758031166909,13.8424380530076));
#14338=CARTESIAN_POINT('Ctrl Pts',(1.62264206521815,-2.78455026812397,13.8536947430961));
#14339=CARTESIAN_POINT('Ctrl Pts',(1.64322372968842,-2.7724543629574,13.8551385783413));
#14340=CARTESIAN_POINT('Ctrl Pts',(1.67421290905569,-2.75377563913955,13.857339627389));
#14341=CARTESIAN_POINT('Ctrl Pts',(1.68472049829767,-2.74735981836555,13.8580907309451));
#14342=CARTESIAN_POINT('Ctrl Pts',(1.70348624584461,-2.73575351715161,13.8594408738137));
#14343=CARTESIAN_POINT('Ctrl Pts',(1.71175813015563,-2.73058543116863,13.8600390805903));
#14344=CARTESIAN_POINT('Ctrl Pts',(1.72918327505788,-2.71958830018016,13.861305796142));
#14345=CARTESIAN_POINT('Ctrl Pts',(1.73833079324856,-2.71375042512134,13.861974628567));
#14346=CARTESIAN_POINT('Ctrl Pts',(1.75698799115922,-2.70171050606463,13.8633467652585));
#14347=CARTESIAN_POINT('Ctrl Pts',(1.7664947218345,-2.69550419255371,13.8640502234756));
#14348=CARTESIAN_POINT('Ctrl Pts',(1.80788925330062,-2.66816741189918,13.8671322131751));
#14349=CARTESIAN_POINT('Ctrl Pts',(1.83943111113826,-2.64652108889642,13.8695301401313));
#14350=CARTESIAN_POINT('Ctrl Pts',(2.02866635102685,-2.51163677532622,13.8842267992039));
#14351=CARTESIAN_POINT('Ctrl Pts',(2.17622227767912,-2.38491938456082,13.8970548275079));
#14352=CARTESIAN_POINT('Ctrl Pts',(2.48139659603935,-2.07081125580598,13.926570628857));
#14353=CARTESIAN_POINT('Ctrl Pts',(2.63093736718886,-1.87717116696135,13.9433275916306));
#14354=CARTESIAN_POINT('Ctrl Pts',(2.76847376049459,-1.64989211498185,13.9602949064087));
#14355=CARTESIAN_POINT('Ctrl Pts',(2.77954981427248,-1.63116334069773,13.961674257012));
#14356=CARTESIAN_POINT('Ctrl Pts',(2.79474728215645,-1.60486119752892,13.9635836997103));
#14357=CARTESIAN_POINT('Ctrl Pts',(2.79902898643129,-1.59738178642921,13.9641235866283));
#14358=CARTESIAN_POINT('Ctrl Pts',(2.80587143709609,-1.58531719837751,13.9649893685728));
#14359=CARTESIAN_POINT('Ctrl Pts',(2.80845103302877,-1.58074284341465,13.9653164658657));
#14360=CARTESIAN_POINT('Ctrl Pts',(2.81383409731772,-1.57114237285293,13.9660004849408));
#14361=CARTESIAN_POINT('Ctrl Pts',(2.81663529691228,-1.56611503021123,13.966357253297));
#14362=CARTESIAN_POINT('Ctrl Pts',(2.82341324021639,-1.55387357734788,13.9672225866999));
#14363=CARTESIAN_POINT('Ctrl Pts',(2.82737585531618,-1.54665160773086,13.9677302485261));
#14364=CARTESIAN_POINT('Ctrl Pts',(2.84132103826209,-1.52100344819781,13.9695233672761));
#14365=CARTESIAN_POINT('Ctrl Pts',(2.85115177575193,-1.50249470443291,13.9707995040502));
#14366=CARTESIAN_POINT('Ctrl Pts',(2.90966592200513,-1.38968494900232,13.9784778413112));
#14367=CARTESIAN_POINT('Ctrl Pts',(2.9538524016105,-1.29311278492101,13.9846326068678));
#14368=CARTESIAN_POINT('Ctrl Pts',(3.10422249771436,-0.916321586715868,
14.0077257341535));
#14369=CARTESIAN_POINT('Ctrl Pts',(3.1759194378451,-0.624008555973554,14.0239106002063));
#14370=CARTESIAN_POINT('Ctrl Pts',(3.2095745976177,-0.292998520352483,14.0434338250568));
#14371=CARTESIAN_POINT('Ctrl Pts',(3.21241945013261,-0.259958446686835,
14.0453934257377));
#14372=CARTESIAN_POINT('Ctrl Pts',(3.21744224503166,-0.188788817954243,
14.0496422973067));
#14373=CARTESIAN_POINT('Ctrl Pts',(3.21945326264819,-0.150652978737051,
14.0519361699742));
#14374=CARTESIAN_POINT('Ctrl Pts',(3.22130937779569,-0.0975098971026946,
14.0551601209091));
#14375=CARTESIAN_POINT('Ctrl Pts',(3.22172809385986,-0.0825249349214185,
14.0560722133335));
#14376=CARTESIAN_POINT('Ctrl Pts',(3.22224020211305,-0.05809365901413,14.0575644079765));
#14377=CARTESIAN_POINT('Ctrl Pts',(3.22239663702435,-0.0486487822809514,
14.0581425244156));
#14378=CARTESIAN_POINT('Ctrl Pts',(3.22261096818201,-0.0310308194195748,
14.0592232949781));
#14379=CARTESIAN_POINT('Ctrl Pts',(3.22267930108349,-0.0228579177843625,
14.0597256166059));
#14380=CARTESIAN_POINT('Ctrl Pts',(3.22273942344462,-0.00966359763668823,
14.0605381352299));
#14381=CARTESIAN_POINT('Ctrl Pts',(3.22275056827357,-0.00464227186255321,
14.0608477205496));
#14382=CARTESIAN_POINT('Ctrl Pts',(3.22274997771073,0.000379032282113146,
14.0611576755349));
#14383=CARTESIAN_POINT('Ctrl Pts',(3.22274997776876,0.000378538572947885,
14.0611576450592));
#14384=CARTESIAN_POINT('Ctrl Pts',(3.22274967767412,0.00293344333988479,
14.0613153541692));
#14385=CARTESIAN_POINT('Ctrl Pts',(3.2227463393961,0.00548834244600403,
14.0614731589751));
#14386=CARTESIAN_POINT('Ctrl Pts',(3.22272011115962,0.0159974016700903,
14.0621226539904));
#14387=CARTESIAN_POINT('Ctrl Pts',(3.22267081155901,0.0239514139831863,
14.0626151740574));
#14388=CARTESIAN_POINT('Ctrl Pts',(3.22236074946736,0.0552693998518561,
14.0645581486519));
#14389=CARTESIAN_POINT('Ctrl Pts',(3.22187535249879,0.0786299738390946,
14.0660156360751));
#14390=CARTESIAN_POINT('Ctrl Pts',(3.21596486344505,0.265313456636337,14.0777306166039));
#14391=CARTESIAN_POINT('Ctrl Pts',(3.19837964774811,0.427988739170791,14.0883715564805));
#14392=CARTESIAN_POINT('Ctrl Pts',(3.12133389613864,0.842733806174139,14.1165211074734));
#14393=CARTESIAN_POINT('Ctrl Pts',(3.04372936911141,1.09024465136447,14.134375414665));
#14394=CARTESIAN_POINT('Ctrl Pts',(2.91659558013825,1.3719127657331,14.1545251651779));
#14395=CARTESIAN_POINT('Ctrl Pts',(2.89471000241654,1.41750805826156,14.1577778018182));
#14396=CARTESIAN_POINT('Ctrl Pts',(2.86663067066838,1.47264179479184,14.1616830093862));
#14397=CARTESIAN_POINT('Ctrl Pts',(2.86144929842948,1.48268445032994,14.1623931916541));
#14398=CARTESIAN_POINT('Ctrl Pts',(2.85323982849152,1.49839290816322,14.1635019783022));
#14399=CARTESIAN_POINT('Ctrl Pts',(2.85024749107995,1.50407714809727,14.1639027762969));
#14400=CARTESIAN_POINT('Ctrl Pts',(2.84461879340147,1.5146922940599,14.1646504021283));
#14401=CARTESIAN_POINT('Ctrl Pts',(2.84198662628928,1.51962523078707,14.1649974770479));
#14402=CARTESIAN_POINT('Ctrl Pts',(2.83593977804495,1.53088694848938,14.1657890589076));
#14403=CARTESIAN_POINT('Ctrl Pts',(2.83251674978123,1.53721115606326,14.1662330274233));
#14404=CARTESIAN_POINT('Ctrl Pts',(2.82189581728083,1.55667790226928,14.1675980636627));
#14405=CARTESIAN_POINT('Ctrl Pts',(2.81462727726891,1.56978196103171,14.1685147422189));
#14406=CARTESIAN_POINT('Ctrl Pts',(2.73953452960236,1.70296413552254,14.17781378473));
#14407=CARTESIAN_POINT('Ctrl Pts',(2.66415133460978,1.81863788532363,14.1857466282412));
#14408=CARTESIAN_POINT('Ctrl Pts',(2.46668193772717,2.08289206122173,14.2043843394804));
#14409=CARTESIAN_POINT('Ctrl Pts',(2.33828081305552,2.22607353727253,14.2149384095779));
#14410=CARTESIAN_POINT('Ctrl Pts',(2.10380002167754,2.4447285822077,14.2331719308684));
#14411=CARTESIAN_POINT('Ctrl Pts',(2.00453894653988,2.52675493511236,14.2406292615811));
#14412=CARTESIAN_POINT('Ctrl Pts',(1.87573095370823,2.62082104910029,14.2501777467641));
#14413=CARTESIAN_POINT('Ctrl Pts',(1.8505539091607,2.63865869543472,14.2520380388337));
#14414=CARTESIAN_POINT('Ctrl Pts',(1.81412882041287,2.66368770722529,14.2547226532618));
#14415=CARTESIAN_POINT('Ctrl Pts',(1.80308567992886,2.67117532204798,14.2555356789102));
#14416=CARTESIAN_POINT('Ctrl Pts',(1.79171128914603,2.67878486194621,14.2563722827108));
#14417=CARTESIAN_POINT('Ctrl Pts',(1.79142605682764,2.67897561824745,14.2563932614628));
#14418=CARTESIAN_POINT('Ctrl Pts',(1.79086399036416,2.67935138445536,14.2564346002612));
#14419=CARTESIAN_POINT('Ctrl Pts',(1.79058715799431,2.67953639702685,14.2564549602074));
#14420=CARTESIAN_POINT('Ctrl Pts',(1.79004070155057,2.679901482222,14.256495148996));
#14421=CARTESIAN_POINT('Ctrl Pts',(1.78977107896822,2.68008155706354,14.2565149777539));
#14422=CARTESIAN_POINT('Ctrl Pts',(1.78923786019216,2.68043756550878,14.2565541911621));
#14423=CARTESIAN_POINT('Ctrl Pts',(1.78897426520726,2.68061350092879,14.2565735757441));
#14424=CARTESIAN_POINT('Ctrl Pts',(1.78845191054901,2.68096203309556,14.2566119884529));
#14425=CARTESIAN_POINT('Ctrl Pts',(1.78819315182996,2.68113463126986,14.2566310165257));
#14426=CARTESIAN_POINT('Ctrl Pts',(1.78767924896271,2.68147730912529,14.2566688060328));
#14427=CARTESIAN_POINT('Ctrl Pts',(1.78742410552117,2.6816473898571,14.256687567427));
#14428=CARTESIAN_POINT('Ctrl Pts',(1.78691615751997,2.68198588750361,14.2567249174172));
#14429=CARTESIAN_POINT('Ctrl Pts',(1.78666335340878,2.68215430509888,14.2567435059877));
#14430=CARTESIAN_POINT('Ctrl Pts',(1.78615872123296,2.68249038704563,14.2567806105619));
#14431=CARTESIAN_POINT('Ctrl Pts',(1.78590689336921,2.68265805168027,14.2567991265538));
#14432=CARTESIAN_POINT('Ctrl Pts',(1.78540272170402,2.68299362200167,14.2568361956802));
#14433=CARTESIAN_POINT('Ctrl Pts',(1.78515037781527,2.68316152755582,14.2568547488195));
#14434=CARTESIAN_POINT('Ctrl Pts',(1.78464349618142,2.68349869526269,14.2568920156013));
#14435=CARTESIAN_POINT('Ctrl Pts',(1.78438895802694,2.68366795681035,14.2569107292671));
#14436=CARTESIAN_POINT('Ctrl Pts',(1.78387574486745,2.68400912551326,14.2569484599295));
#14437=CARTESIAN_POINT('Ctrl Pts',(1.7836170690936,2.68418103148851,14.2569674769696));
#14438=CARTESIAN_POINT('Ctrl Pts',(1.78309325856536,2.68452902667538,14.2570059850556));
#14439=CARTESIAN_POINT('Ctrl Pts',(1.78282812257556,2.68470511400368,14.2570254761715));
#14440=CARTESIAN_POINT('Ctrl Pts',(1.78228851931199,2.68506337075063,14.2570651434974));
#14441=CARTESIAN_POINT('Ctrl Pts',(1.78201405018803,2.68524553736718,14.2570853198126));
#14442=CARTESIAN_POINT('Ctrl Pts',(1.78145209037566,2.68561838897635,14.2571266287138));
#14443=CARTESIAN_POINT('Ctrl Pts',(1.78116459699617,2.68580906989292,14.2571477614529));
#14444=CARTESIAN_POINT('Ctrl Pts',(1.78057163875083,2.68620221429373,14.257191346914));
#14445=CARTESIAN_POINT('Ctrl Pts',(1.78026616996209,2.68640467184091,14.2572137998592));
#14446=CARTESIAN_POINT('Ctrl Pts',(1.77963027441382,2.68682597240014,14.2572605390548));
#14447=CARTESIAN_POINT('Ctrl Pts',(1.77929984182474,2.68704480655914,14.2572848256371));
#14448=CARTESIAN_POINT('Ctrl Pts',(1.77860351060529,2.68750577805424,14.2573360041327));
#14449=CARTESIAN_POINT('Ctrl Pts',(1.77823760290523,2.68774790161316,14.2573628965627));
#14450=CARTESIAN_POINT('Ctrl Pts',(1.77753738876963,2.68821103238402,14.2574143573316));
#14451=CARTESIAN_POINT('Ctrl Pts',(1.7772030905083,2.68843205199474,14.2574389252041));
#14452=CARTESIAN_POINT('Ctrl Pts',(1.76889133356015,2.6939251004238,14.2580497467428));
#14453=CARTESIAN_POINT('Ctrl Pts',(1.76089056103802,2.69916161530606,14.2586373305727));
#14454=CARTESIAN_POINT('Ctrl Pts',(1.7425349770877,2.71105901903736,14.2599845675654));
#14455=CARTESIAN_POINT('Ctrl Pts',(1.73216511028682,2.71769629926261,14.2607450927187));
#14456=CARTESIAN_POINT('Ctrl Pts',(1.70157491656341,2.73702948652854,14.262987005587));
#14457=CARTESIAN_POINT('Ctrl Pts',(1.68125158263003,2.74956008720793,14.2644744802464));
#14458=CARTESIAN_POINT('Ctrl Pts',(1.52087563804502,2.84599895277093,14.2761992751412));
#14459=CARTESIAN_POINT('Ctrl Pts',(1.37479103207176,2.91936771099399,14.2868195595402));
#14460=CARTESIAN_POINT('Ctrl Pts',(0.989893130140116,3.07736235920731,14.3145656525276));
#14461=CARTESIAN_POINT('Ctrl Pts',(0.745515525725842,3.14551251764869,14.3320153658719));
#14462=CARTESIAN_POINT('Ctrl Pts',(0.438517603884532,3.19330045863065,14.352358259319));
#14463=CARTESIAN_POINT('Ctrl Pts',(0.38111102855807,3.20065944456107,14.3560920916717));
#14464=CARTESIAN_POINT('Ctrl Pts',(0.311830560277556,3.20764985856982,14.3604898297074));
#14465=CARTESIAN_POINT('Ctrl Pts',(0.3001211205991,3.20876662232385,14.3612293977294));
#14466=CARTESIAN_POINT('Ctrl Pts',(0.281907049715131,3.21040317563946,14.3623737490723));
#14467=CARTESIAN_POINT('Ctrl Pts',(0.275406654434022,3.21096734821765,14.3627809584953));
#14468=CARTESIAN_POINT('Ctrl Pts',(0.263344929312413,3.21197729389303,14.3635342750501));
#14469=CARTESIAN_POINT('Ctrl Pts',(0.257784206398508,3.21242836370809,14.363880667718));
#14470=CARTESIAN_POINT('Ctrl Pts',(0.245197175918996,3.21341649379329,14.364662726967));
#14471=CARTESIAN_POINT('Ctrl Pts',(0.238170279239326,3.2139449494316,14.3650979052464));
#14472=CARTESIAN_POINT('Ctrl Pts',(0.21738041540565,3.21543988710894,14.3663813851237));
#14473=CARTESIAN_POINT('Ctrl Pts',(0.203612705605847,3.21634105693527,14.3672261068646));
#14474=CARTESIAN_POINT('Ctrl Pts',(0.101702784767804,3.22235460624036,14.3734428661398));
#14475=CARTESIAN_POINT('Ctrl Pts',(0.0133808674177226,3.22393186355365,
14.378632135278));
#14476=CARTESIAN_POINT('Ctrl Pts',(-0.322468548617493,3.21612402209149,
14.3979816956495));
#14477=CARTESIAN_POINT('Ctrl Pts',(-0.568555215608009,3.18185471359297,
14.4114285204181));
#14478=CARTESIAN_POINT('Ctrl Pts',(-0.896724692867139,3.09682835423077,
14.430733669533));
#14479=CARTESIAN_POINT('Ctrl Pts',(-0.984127790872031,3.07017126912715,
14.4360073642664));
#14480=CARTESIAN_POINT('Ctrl Pts',(-1.12294659424284,3.02129550969271,14.444686821237));
#14481=CARTESIAN_POINT('Ctrl Pts',(-1.17512338168107,3.00138635958863,14.4480201349785));
#14482=CARTESIAN_POINT('Ctrl Pts',(-1.24260787253953,2.97360675920239,14.452436406297));
#14483=CARTESIAN_POINT('Ctrl Pts',(-1.25840876374391,2.96695447368759,14.4534780712834));
#14484=CARTESIAN_POINT('Ctrl Pts',(-1.28411432411955,2.95588997021927,14.4551855154937));
#14485=CARTESIAN_POINT('Ctrl Pts',(-1.29405126398141,2.95155322416806,14.4558487094634));
#14486=CARTESIAN_POINT('Ctrl Pts',(-1.31318518372179,2.94308747178516,14.4571318902334));
#14487=CARTESIAN_POINT('Ctrl Pts',(-1.32238505641324,2.9389652859832,14.4577516365763));
#14488=CARTESIAN_POINT('Ctrl Pts',(-1.34350092750508,2.92938468015524,14.4591805661273));
#14489=CARTESIAN_POINT('Ctrl Pts',(-1.35540321002592,2.92389662550317,14.4599907662541));
#14490=CARTESIAN_POINT('Ctrl Pts',(-1.38714894233019,2.9090234122377,14.4621646653525));
#14491=CARTESIAN_POINT('Ctrl Pts',(-1.40693026423603,2.89950799175033,14.4635328682284));
#14492=CARTESIAN_POINT('Ctrl Pts',(-1.57359812406625,2.8172285434943,14.475178387118));
#14493=CARTESIAN_POINT('Ctrl Pts',(-1.71481027312923,2.73356886690281,14.4858432045254));
#14494=CARTESIAN_POINT('Ctrl Pts',(-2.05720231681463,2.49371949561247,14.5137262555303));
#14495=CARTESIAN_POINT('Ctrl Pts',(-2.24738180071733,2.32378755176123,14.531271085042));
#14496=CARTESIAN_POINT('Ctrl Pts',(-2.45272261528797,2.09127019667595,14.5515617733742));
#14497=CARTESIAN_POINT('Ctrl Pts',(-2.48872559651583,2.04829320970447,14.5551759596538));
#14498=CARTESIAN_POINT('Ctrl Pts',(-2.53084003124578,1.99526993740475,14.5594518888165));
#14499=CARTESIAN_POINT('Ctrl Pts',(-2.53803906593545,1.9861045029021,14.5601845930571));
#14500=CARTESIAN_POINT('Ctrl Pts',(-2.54917634667188,1.97176565095079,14.5613206451771));
#14501=CARTESIAN_POINT('Ctrl Pts',(-2.55314883893586,1.96661913870326,14.5617263639716));
#14502=CARTESIAN_POINT('Ctrl Pts',(-2.56050278894569,1.95703198301917,14.5624783279329));
#14503=CARTESIAN_POINT('Ctrl Pts',(-2.5638882517552,1.95259461946905,14.5628248497679));
#14504=CARTESIAN_POINT('Ctrl Pts',(-2.57154120141764,1.94250959255976,14.5636089888774));
#14505=CARTESIAN_POINT('Ctrl Pts',(-2.57580160959158,1.93685666430392,14.5640461067692));
#14506=CARTESIAN_POINT('Ctrl Pts',(-2.58840031243995,1.92002496697108,14.5653406352771));
#14507=CARTESIAN_POINT('Ctrl Pts',(-2.59668483577818,1.90880589143384,14.5661943737113));
#14508=CARTESIAN_POINT('Ctrl Pts',(-2.6594050999744,1.82270473820819,14.5726800545787));
#14509=CARTESIAN_POINT('Ctrl Pts',(-2.71066981118429,1.74555454775614,14.5781108556848));
#14510=CARTESIAN_POINT('Ctrl Pts',(-2.88372455055585,1.45906327039345,14.5973486673834));
#14511=CARTESIAN_POINT('Ctrl Pts',(-2.98515738935376,1.23837841286995,14.610512716537));
#14512=CARTESIAN_POINT('Ctrl Pts',(-3.08970278440933,0.921040255274114,
14.6295336777268));
#14513=CARTESIAN_POINT('Ctrl Pts',(-3.11472910001279,0.832489728804896,
14.6348427867794));
#14514=CARTESIAN_POINT('Ctrl Pts',(-3.14887122121812,0.688387228352557,
14.6435751939299));
#14515=CARTESIAN_POINT('Ctrl Pts',(-3.16038015163296,0.633453758486885,
14.6469248801916));
#14516=CARTESIAN_POINT('Ctrl Pts',(-3.17353024451126,0.561354013047729,
14.6513598175218));
#14517=CARTESIAN_POINT('Ctrl Pts',(-3.17647673730421,0.544433706151925,
14.6524033311317));
#14518=CARTESIAN_POINT('Ctrl Pts',(-3.18106351312561,0.516788337810951,
14.6541130432923));
#14519=CARTESIAN_POINT('Ctrl Pts',(-3.18278515616924,0.506076976114933,
14.654776643302));
#14520=CARTESIAN_POINT('Ctrl Pts',(-3.18600183430004,0.485398244349972,
14.6560600741534));
#14521=CARTESIAN_POINT('Ctrl Pts',(-3.18750426204822,0.475432139766166,
14.6566796616597));
#14522=CARTESIAN_POINT('Ctrl Pts',(-3.19085062436683,0.452505502345633,
14.6581074569641));
#14523=CARTESIAN_POINT('Ctrl Pts',(-3.19266237796002,0.439540520208768,
14.6589166764253));
#14524=CARTESIAN_POINT('Ctrl Pts',(-3.19729339174301,0.404860489739731,
14.6610862347029));
#14525=CARTESIAN_POINT('Ctrl Pts',(-3.19997037114034,0.38312743915562,14.6624510492313));
#14526=CARTESIAN_POINT('Ctrl Pts',(-3.22076449645263,0.198851535730365,
14.6740693715794));
#14527=CARTESIAN_POINT('Ctrl Pts',(-3.22670300391755,0.0351993286825831,
14.6847085972871));
#14528=CARTESIAN_POINT('Ctrl Pts',(-3.21012794740424,-0.38122106731115,
14.7125020350797));
#14529=CARTESIAN_POINT('Ctrl Pts',(-3.17026651407814,-0.632183657607774,
14.7299806505244));
#14530=CARTESIAN_POINT('Ctrl Pts',(-3.08586703458046,-0.93103492043124,
14.7503072021715));
#14531=CARTESIAN_POINT('Ctrl Pts',(-3.06882334321127,-0.985761445944426,
14.754004220341));
#14532=CARTESIAN_POINT('Ctrl Pts',(-3.04654275455866,-1.0511100746245,14.7583645226158));
#14533=CARTESIAN_POINT('Ctrl Pts',(-3.04269688772852,-1.0621915099075,14.7591020077218));
#14534=CARTESIAN_POINT('Ctrl Pts',(-3.03662001351166,-1.07939748723584,
14.7602438410658));
#14535=CARTESIAN_POINT('Ctrl Pts',(-3.03443083007812,-1.08553654068747,
14.7606505986015));
#14536=CARTESIAN_POINT('Ctrl Pts',(-3.03033294353346,-1.09691884263039,
14.7614035033416));
#14537=CARTESIAN_POINT('Ctrl Pts',(-3.02842926557617,-1.10216372654799,
14.7617499333983));
#14538=CARTESIAN_POINT('Ctrl Pts',(-3.02408727241414,-1.11403030536733,
14.7625326151189));
#14539=CARTESIAN_POINT('Ctrl Pts',(-3.02164083193596,-1.12064893587091,
14.762968375156));
#14540=CARTESIAN_POINT('Ctrl Pts',(-3.01433117168504,-1.14022661541805,
14.7642551641995));
#14541=CARTESIAN_POINT('Ctrl Pts',(-3.00940610863046,-1.15316262356423,
14.765102585819));
#14542=CARTESIAN_POINT('Ctrl Pts',(-2.97200491269003,-1.24952766217803,
14.7713970211322));
#14543=CARTESIAN_POINT('Ctrl Pts',(-2.93614507618829,-1.331610990725,14.7766560568186));
#14544=CARTESIAN_POINT('Ctrl Pts',(-2.78913018677072,-1.63321026300772,
14.7959697020759));
#14545=CARTESIAN_POINT('Ctrl Pts',(-2.65638802951668,-1.8412603762879,14.8093319711001));
#14546=CARTESIAN_POINT('Ctrl Pts',(-2.44352295430689,-2.10325870578603,
14.8285534639843));
#14547=CARTESIAN_POINT('Ctrl Pts',(-2.38278591884533,-2.17182664258112,
14.833839428391));
#14548=CARTESIAN_POINT('Ctrl Pts',(-2.28037603687493,-2.2779665469539,14.8425372349247));
#14549=CARTESIAN_POINT('Ctrl Pts',(-2.24049707040061,-2.31720063105109,
14.8458762266778));
#14550=CARTESIAN_POINT('Ctrl Pts',(-2.18708133822446,-2.36708408603244,
14.8502989720815));
#14551=CARTESIAN_POINT('Ctrl Pts',(-2.17445049053268,-2.3786922661156,14.851341279142));
#14552=CARTESIAN_POINT('Ctrl Pts',(-2.15368481318203,-2.39747302175114,
14.8530495110448));
#14553=CARTESIAN_POINT('Ctrl Pts',(-2.14560528662977,-2.40470645069119,
14.853712846021));
#14554=CARTESIAN_POINT('Ctrl Pts',(-2.12994536816959,-2.41858469040365,
14.8549961134002));
#14555=CARTESIAN_POINT('Ctrl Pts',(-2.12236999604031,-2.42523499320478,
14.8556158043454));
#14556=CARTESIAN_POINT('Ctrl Pts',(-2.10487760822538,-2.44044656941355,
14.857044338872));
#14557=CARTESIAN_POINT('Ctrl Pts',(-2.09493938888231,-2.44898308539132,
14.8578541975418));
#14558=CARTESIAN_POINT('Ctrl Pts',(-2.0682254935597,-2.47164760616838,14.8600265848763));
#14559=CARTESIAN_POINT('Ctrl Pts',(-2.05135741377376,-2.48566516325797,
14.8613936076172));
#14560=CARTESIAN_POINT('Ctrl Pts',(-1.90613576389792,-2.60386091174171,
14.8731248309722));
#14561=CARTESIAN_POINT('Ctrl Pts',(-1.7701052656151,-2.69817669660086,14.88388347364));
#14562=CARTESIAN_POINT('Ctrl Pts',(-1.57745449062304,-2.8108915892576,14.8987759855522));
#14563=CARTESIAN_POINT('Ctrl Pts',(-1.52669994797171,-2.83877667198752,
14.9026674496955));
#14564=CARTESIAN_POINT('Ctrl Pts',(-1.47525516809595,-2.86526434234368,
14.9065719799118));
#14565=CARTESIAN_POINT('Origin',(0.,0.,4.68922655072688));
#14566=CARTESIAN_POINT('',(-1.47525540582449,-2.86526421994301,16.4055744628637));
#14567=CARTESIAN_POINT('',(-1.47525540483048,-2.8652642204548,16.1601692104994));
#14568=CARTESIAN_POINT('',(-1.47525540501186,-2.86526422036142,4.68922655072688));
#14569=CARTESIAN_POINT('',(3.22274959861812,-0.00160844855869799,15.5583907367487));
#14570=CARTESIAN_POINT('Ctrl Pts',(-1.47525540582449,-2.86526421994301,
16.4055744628637));
#14571=CARTESIAN_POINT('Ctrl Pts',(-1.68834631514222,-2.75554885278246,
16.3897071016039));
#14572=CARTESIAN_POINT('Ctrl Pts',(-1.88851797500529,-2.62241399723029,
16.3732267052815));
#14573=CARTESIAN_POINT('Ctrl Pts',(-2.1430559897236,-2.40873765580771,16.3511110036867));
#14574=CARTESIAN_POINT('Ctrl Pts',(-2.2114400298354,-2.34611221874768,16.3450431196542));
#14575=CARTESIAN_POINT('Ctrl Pts',(-2.28690899564965,-2.27076187177162,
16.3382878637327));
#14576=CARTESIAN_POINT('Ctrl Pts',(-2.29671869530835,-2.2608395528794,16.3374086103913));
#14577=CARTESIAN_POINT('Ctrl Pts',(-2.31140963825781,-2.24578565136435,
16.3360904939948));
#14578=CARTESIAN_POINT('Ctrl Pts',(-2.31633876358725,-2.24070132821915,
16.335648005267));
#14579=CARTESIAN_POINT('Ctrl Pts',(-2.32512429014357,-2.23157921030102,
16.3348589787052));
#14580=CARTESIAN_POINT('Ctrl Pts',(-2.32898698045568,-2.22754761630584,
16.3345119539501));
#14581=CARTESIAN_POINT('Ctrl Pts',(-2.33732623917017,-2.21879830282613,
16.3337625085123));
#14582=CARTESIAN_POINT('Ctrl Pts',(-2.34179899734263,-2.21407707967633,
16.3333603810583));
#14583=CARTESIAN_POINT('Ctrl Pts',(-2.35424955504378,-2.20085494830625,
16.3322404356902));
#14584=CARTESIAN_POINT('Ctrl Pts',(-2.36219566037684,-2.19232414179238,
16.3315250183069));
#14585=CARTESIAN_POINT('Ctrl Pts',(-2.40808490567337,-2.14251904577547,
16.3273882913274));
#14586=CARTESIAN_POINT('Ctrl Pts',(-2.44499469297349,-2.10030059973463,
16.3240403803592));
#14587=CARTESIAN_POINT('Ctrl Pts',(-2.64306072726742,-1.86144465891646,
16.3058174478728));
#14588=CARTESIAN_POINT('Ctrl Pts',(-2.78162516580758,-1.64722039289585,
16.292022116168));
#14589=CARTESIAN_POINT('Ctrl Pts',(-2.96573209890492,-1.27177356115637,
16.2684027065213));
#14590=CARTESIAN_POINT('Ctrl Pts',(-3.02654866310058,-1.11936036130739,
16.2589591227187));
#14591=CARTESIAN_POINT('Ctrl Pts',(-3.0820557571412,-0.942088044346691,
16.2477862955936));
#14592=CARTESIAN_POINT('Ctrl Pts',(-3.08838896622197,-0.921114070263639,
16.2464617905686));
#14593=CARTESIAN_POINT('Ctrl Pts',(-3.09816550623526,-0.887501878986326,
16.2443343534264));
#14594=CARTESIAN_POINT('Ctrl Pts',(-3.10174656412547,-0.874904185164823,
16.2435359242277));
#14595=CARTESIAN_POINT('Ctrl Pts',(-3.10794838331993,-0.852570270231802,
16.2421183787465));
#14596=CARTESIAN_POINT('Ctrl Pts',(-3.11060044349003,-0.842842865755071,
16.2415002919381));
#14597=CARTESIAN_POINT('Ctrl Pts',(-3.11601215284392,-0.822619958170176,
16.2402138265674));
#14598=CARTESIAN_POINT('Ctrl Pts',(-3.11876451857431,-0.81212265411104,
16.2395452200479));
#14599=CARTESIAN_POINT('Ctrl Pts',(-3.12573672914095,-0.784972973761023,
16.2378137379133));
#14600=CARTESIAN_POINT('Ctrl Pts',(-3.12987649818459,-0.768300564316399,
16.2367482830876));
#14601=CARTESIAN_POINT('Ctrl Pts',(-3.14697067769129,-0.697024046431928,
16.2321835827143));
#14602=CARTESIAN_POINT('Ctrl Pts',(-3.15863026063162,-0.642122422332045,
16.2286429715399));
#14603=CARTESIAN_POINT('Ctrl Pts',(-3.18560120036819,-0.496509859543548,
16.2191817992671));
#14604=CARTESIAN_POINT('Ctrl Pts',(-3.19847177631633,-0.40540451341519,
16.2131895199814));
#14605=CARTESIAN_POINT('Ctrl Pts',(-3.2310090566347,-0.0729175667754314,
16.1910887371651));
#14606=CARTESIAN_POINT('Ctrl Pts',(-3.22735998951859,0.169909127581393,
16.1744379425507));
#14607=CARTESIAN_POINT('Ctrl Pts',(-3.18477945000895,0.501867914894173,
16.1521669799668));
#14608=CARTESIAN_POINT('Ctrl Pts',(-3.16904459237215,0.593170626451046,
16.1461044033647));
#14609=CARTESIAN_POINT('Ctrl Pts',(-3.14643791796135,0.697309536097229,
16.1393542976587));
#14610=CARTESIAN_POINT('Ctrl Pts',(-3.14339003982371,0.710922805101249,
16.1384752088278));
#14611=CARTESIAN_POINT('Ctrl Pts',(-3.13866194822679,0.731415664773641,
16.1371572901847));
#14612=CARTESIAN_POINT('Ctrl Pts',(-3.13704734464756,0.738310002395416,
16.1367148362775));
#14613=CARTESIAN_POINT('Ctrl Pts',(-3.13411897744876,0.750631048640793,
16.1359258472998));
#14614=CARTESIAN_POINT('Ctrl Pts',(-3.13281382641785,0.756059697756088,
16.1355788255027));
#14615=CARTESIAN_POINT('Ctrl Pts',(-3.12995779253087,0.767804714171637,
16.1348293586037));
#14616=CARTESIAN_POINT('Ctrl Pts',(-3.12840190013486,0.774119767947654,
16.1344272068802));
#14617=CARTESIAN_POINT('Ctrl Pts',(-3.12400331372911,0.791742893487019,
16.1333071253659));
#14618=CARTESIAN_POINT('Ctrl Pts',(-3.12111831924455,0.803040447635769,
16.1325915970517));
#14619=CARTESIAN_POINT('Ctrl Pts',(-3.10399810666504,0.868596515740998,
16.1284529287458));
#14620=CARTESIAN_POINT('Ctrl Pts',(-3.08840856759553,0.922495288734444,
16.1251032679254));
#14621=CARTESIAN_POINT('Ctrl Pts',(-2.99443819224608,1.21822607160023,16.1068802469312));
#14622=CARTESIAN_POINT('Ctrl Pts',(-2.88905845907002,1.4505527951818,16.09308607898));
#14623=CARTESIAN_POINT('Ctrl Pts',(-2.67263700545135,1.80830937920154,16.0694684747699));
#14624=CARTESIAN_POINT('Ctrl Pts',(-2.57725778054361,1.94182987495263,16.0600254745735));
#14625=CARTESIAN_POINT('Ctrl Pts',(-2.45809350713611,2.08431616465558,16.0488533003112));
#14626=CARTESIAN_POINT('Ctrl Pts',(-2.44386739788618,2.10097826483533,16.0475288080214));
#14627=CARTESIAN_POINT('Ctrl Pts',(-2.42086760298079,2.12736671414123,16.0454013874718));
#14628=CARTESIAN_POINT('Ctrl Pts',(-2.41220243310124,2.13718705343997,16.0446029620182));
#14629=CARTESIAN_POINT('Ctrl Pts',(-2.39676092841285,2.15447354843376,16.0431854208708));
#14630=CARTESIAN_POINT('Ctrl Pts',(-2.39000892405974,2.16196127581243,16.0425673346301));
#14631=CARTESIAN_POINT('Ctrl Pts',(-2.37591671578696,2.17744232816478,16.0412808681316));
#14632=CARTESIAN_POINT('Ctrl Pts',(-2.36857106060516,2.18543049742853,16.0406122599051));
#14633=CARTESIAN_POINT('Ctrl Pts',(-2.34949349781975,2.20596758302776,16.0388807683847));
#14634=CARTESIAN_POINT('Ctrl Pts',(-2.33770146348104,2.21845994394444,16.0378153058269));
#14635=CARTESIAN_POINT('Ctrl Pts',(-2.28696234881986,2.27135869215398,16.0332505274538));
#14636=CARTESIAN_POINT('Ctrl Pts',(-2.24706522913268,2.31083627944824,16.0297098442537));
#14637=CARTESIAN_POINT('Ctrl Pts',(-2.13911159763896,2.41221456214176,16.0202484306416));
#14638=CARTESIAN_POINT('Ctrl Pts',(-2.06940423957531,2.47227447686804,16.0142559774932));
#14639=CARTESIAN_POINT('Ctrl Pts',(-1.80723586196336,2.67929502855329,15.9921567990691));
#14640=CARTESIAN_POINT('Ctrl Pts',(-1.60096405729656,2.80742275405419,15.9755079529812));
#14641=CARTESIAN_POINT('Ctrl Pts',(-1.29863867972593,2.95097160053913,15.9532370945625));
#14642=CARTESIAN_POINT('Ctrl Pts',(-1.21328965092433,2.98707674896513,15.9471729641674));
#14643=CARTESIAN_POINT('Ctrl Pts',(-1.11342568548895,3.02433387828785,15.9404213920042));
#14644=CARTESIAN_POINT('Ctrl Pts',(-1.10032387213833,3.02912521323038,15.9395422946014));
#14645=CARTESIAN_POINT('Ctrl Pts',(-1.08052535662699,3.03622012608023,15.9382243656541));
#14646=CARTESIAN_POINT('Ctrl Pts',(-1.0738516984519,3.03858688082716,15.9377819099325));
#14647=CARTESIAN_POINT('Ctrl Pts',(-1.06190188947173,3.04278049046413,15.9369929189964));
#14648=CARTESIAN_POINT('Ctrl Pts',(-1.05662875970516,3.04461564105465,15.9366458970453));
#14649=CARTESIAN_POINT('Ctrl Pts',(-1.04520277810696,3.04855884222297,15.935896431265));
#14650=CARTESIAN_POINT('Ctrl Pts',(-1.03904832468023,3.05066196793472,15.9354942808065));
#14651=CARTESIAN_POINT('Ctrl Pts',(-1.02184283421211,3.05648339330068,15.9343742063884));
#14652=CARTESIAN_POINT('Ctrl Pts',(-1.01077779045486,3.06016041725948,15.9336586838561));
#14653=CARTESIAN_POINT('Ctrl Pts',(-0.946366892727751,3.08117732067997,
15.9295201167653));
#14654=CARTESIAN_POINT('Ctrl Pts',(-0.892591959911847,3.09718330987246,
15.9261705471776));
#14655=CARTESIAN_POINT('Ctrl Pts',(-0.592975555588708,3.17791054502726,
15.9079475308191));
#14656=CARTESIAN_POINT('Ctrl Pts',(-0.340543308574817,3.21477729250494,
15.8941533022085));
#14657=CARTESIAN_POINT('Ctrl Pts',(0.0774326007228325,3.22598446194281,
15.870535603872));
#14658=CARTESIAN_POINT('Ctrl Pts',(0.241320837740447,3.21787590909853,15.8610925732337));
#14659=CARTESIAN_POINT('Ctrl Pts',(0.425605468836167,3.19459818278516,15.8499203649169));
#14660=CARTESIAN_POINT('Ctrl Pts',(0.447312713613298,3.19163106647518,15.8485958719627));
#14661=CARTESIAN_POINT('Ctrl Pts',(0.481944959607074,3.18653701431389,15.8464684505476));
#14662=CARTESIAN_POINT('Ctrl Pts',(0.494890411856844,3.18455217573653,15.8456700248987));
#14663=CARTESIAN_POINT('Ctrl Pts',(0.517779777362965,3.18089976595167,15.8442524835251));
#14664=CARTESIAN_POINT('Ctrl Pts',(0.527728695034615,3.17926432365178,15.8436343972548));
#14665=CARTESIAN_POINT('Ctrl Pts',(0.548369791740922,3.17577170217175,15.8423479308152));
#14666=CARTESIAN_POINT('Ctrl Pts',(0.559060578125948,3.17390715021434,15.8416793226778));
#14667=CARTESIAN_POINT('Ctrl Pts',(0.586649850824553,3.1689516604034,15.839947831647));
#14668=CARTESIAN_POINT('Ctrl Pts',(0.603533238405973,3.1657795698952,15.8388823694926));
#14669=CARTESIAN_POINT('Ctrl Pts',(0.675461159189337,3.15166928931439,15.8343175951885));
#14670=CARTESIAN_POINT('Ctrl Pts',(0.730237513473711,3.13942982430677,15.8307769157458));
#14671=CARTESIAN_POINT('Ctrl Pts',(0.873873755451342,3.10337270656353,15.8213155147237));
#14672=CARTESIAN_POINT('Ctrl Pts',(0.96207676678163,3.07717130916081,15.8153230706453));
#14673=CARTESIAN_POINT('Ctrl Pts',(1.18657921008579,2.99988476433525,15.7996156278636));
#14674=CARTESIAN_POINT('Ctrl Pts',(1.32075392492261,2.9432775479278,15.789774303263));
#14675=CARTESIAN_POINT('Ctrl Pts',(1.61878358001441,2.79304754868328,15.7671825403333));
#14676=CARTESIAN_POINT('Ctrl Pts',(1.7791985632143,2.69370450917543,15.7544651746456));
#14677=CARTESIAN_POINT('Ctrl Pts',(1.94175790024126,2.57214077514126,15.7415997014587));
#14678=CARTESIAN_POINT('Ctrl Pts',(1.95342308186026,2.56329284176574,15.7406767354938));
#14679=CARTESIAN_POINT('Ctrl Pts',(1.97067508270864,2.55002118535784,15.7393126175928));
#14680=CARTESIAN_POINT('Ctrl Pts',(1.97630798928483,2.54565808018037,15.7388673647797));
#14681=CARTESIAN_POINT('Ctrl Pts',(1.98633197584778,2.53784043194077,15.7380753435445));
#14682=CARTESIAN_POINT('Ctrl Pts',(1.99072857456762,2.53439312662783,15.7377280727559));
#14683=CARTESIAN_POINT('Ctrl Pts',(1.9951335648479,2.53092070626502,15.7373802610597));
#14684=CARTESIAN_POINT('Ctrl Pts',(1.99515083707017,2.53090709041678,15.7373788972716));
#14685=CARTESIAN_POINT('Ctrl Pts',(1.99518510569134,2.53088007558554,15.7373761914777));
#14686=CARTESIAN_POINT('Ctrl Pts',(1.99520210208371,2.53086667661676,15.7373748494722));
#14687=CARTESIAN_POINT('Ctrl Pts',(1.9952358245205,2.53084009125501,15.7373721868109));
#14688=CARTESIAN_POINT('Ctrl Pts',(1.99525255057485,2.53082690486295,15.7373708661543));
#14689=CARTESIAN_POINT('Ctrl Pts',(1.99528573758302,2.53080074054383,15.7373682457761));
#14690=CARTESIAN_POINT('Ctrl Pts',(1.99530219859447,2.53078776257976,15.7373669460499));
#14691=CARTESIAN_POINT('Ctrl Pts',(1.9953348608891,2.53076201090627,15.7373643671084));
#14692=CARTESIAN_POINT('Ctrl Pts',(1.99535106212959,2.53074923723864,15.7373630878964));
#14693=CARTESIAN_POINT('Ctrl Pts',(1.99538320984656,2.53072389026832,15.737360549591));
#14694=CARTESIAN_POINT('Ctrl Pts',(1.99539915636008,2.53071131694428,15.7373592904947));
#14695=CARTESIAN_POINT('Ctrl Pts',(2.0004341331456,2.52674131903528,15.7369617419573));
#14696=CARTESIAN_POINT('Ctrl Pts',(2.00544143099379,2.52276893173033,15.7365665288906));
#14697=CARTESIAN_POINT('Ctrl Pts',(2.01911267217375,2.51185684321436,15.7354878017362));
#14698=CARTESIAN_POINT('Ctrl Pts',(2.02775272687349,2.50488715729205,15.7348064004234));
#14699=CARTESIAN_POINT('Ctrl Pts',(2.04712329807086,2.48909556354318,15.7332790593965));
#14700=CARTESIAN_POINT('Ctrl Pts',(2.05783320464941,2.48024858413226,15.7324348271544));
#14701=CARTESIAN_POINT('Ctrl Pts',(2.09093348659294,2.45254390910229,15.7298251367465));
#14702=CARTESIAN_POINT('Ctrl Pts',(2.11312498442638,2.43344969074064,15.7280748141098));
#14703=CARTESIAN_POINT('Ctrl Pts',(2.19903686834224,2.35746695244925,15.721281771039));
#14704=CARTESIAN_POINT('Ctrl Pts',(2.26074943910409,2.29835324778644,15.7163646434504));
#14705=CARTESIAN_POINT('Ctrl Pts',(2.46445226745962,2.08707449693093,15.6997039356266));
#14706=CARTESIAN_POINT('Ctrl Pts',(2.5940175084814,1.92366368301244,15.6883031830026));
#14707=CARTESIAN_POINT('Ctrl Pts',(2.78241709293188,1.63206084422852,15.6685552412657));
#14708=CARTESIAN_POINT('Ctrl Pts',(2.85025277870055,1.51046997480914,15.6604775115245));
#14709=CARTESIAN_POINT('Ctrl Pts',(2.9191744353878,1.36564717326451,15.6508258111849));
#14710=CARTESIAN_POINT('Ctrl Pts',(2.92813966916638,1.34631706164547,15.6495371693472));
#14711=CARTESIAN_POINT('Ctrl Pts',(2.94223215709115,1.3151252550413,15.6474565014156));
#14712=CARTESIAN_POINT('Ctrl Pts',(2.94748099658353,1.30331894400933,15.6466686671447));
#14713=CARTESIAN_POINT('Ctrl Pts',(2.95668837845431,1.28226850298116,15.64526332467));
#14714=CARTESIAN_POINT('Ctrl Pts',(2.96067493846058,1.27303675758182,15.6446467867505));
#14715=CARTESIAN_POINT('Ctrl Pts',(2.96890532592276,1.25372973484051,15.6433568487929));
#14716=CARTESIAN_POINT('Ctrl Pts',(2.97314121574874,1.24365123278802,15.6426831873608));
#14717=CARTESIAN_POINT('Ctrl Pts',(2.98404041537881,1.21734469598425,15.6409239470946));
#14718=CARTESIAN_POINT('Ctrl Pts',(2.99062257811499,1.20108362952207,15.6398356304403));
#14719=CARTESIAN_POINT('Ctrl Pts',(3.01895604927355,1.1294094242253,15.635034270957));
#14720=CARTESIAN_POINT('Ctrl Pts',(3.03930119437825,1.0734564562034,15.631274343199));
#14721=CARTESIAN_POINT('Ctrl Pts',(3.08962533327696,0.922129779437808,15.6210674946168));
#14722=CARTESIAN_POINT('Ctrl Pts',(3.1167342229732,0.825876891313651,15.6145339986356));
#14723=CARTESIAN_POINT('Ctrl Pts',(3.19488793012977,0.489101728728742,15.5915790097839));
#14724=CARTESIAN_POINT('Ctrl Pts',(3.22287224785179,0.244136288781952,15.574647590367));
#14725=CARTESIAN_POINT('Ctrl Pts',(3.22274959861812,-0.00160844855869799,
15.5583907367487));
#14726=CARTESIAN_POINT('Ctrl Pts',(3.22274959627015,-0.00161314617362317,
15.5583904259856));
#14727=CARTESIAN_POINT('Ctrl Pts',(3.2227108806265,-0.0789594071645176,
15.5532737099094));
#14728=CARTESIAN_POINT('Ctrl Pts',(3.21988768448667,-0.156287636072416,
15.5482375533698));
#14729=CARTESIAN_POINT('Ctrl Pts',(3.21357695463654,-0.243178797591008,
15.5427212586633));
#14730=CARTESIAN_POINT('Ctrl Pts',(3.21282594566517,-0.252907531430216,
15.542105655882));
#14731=CARTESIAN_POINT('Ctrl Pts',(3.21150074981319,-0.269114833295441,
15.5410836570118));
#14732=CARTESIAN_POINT('Ctrl Pts',(3.21095112233921,-0.275595267067559,
15.5406759600701));
#14733=CARTESIAN_POINT('Ctrl Pts',(3.20991860236183,-0.287346732048848,
15.5399384224973));
#14734=CARTESIAN_POINT('Ctrl Pts',(3.209442336118,-0.292618301374302,15.5396082184293));
#14735=CARTESIAN_POINT('Ctrl Pts',(3.20843766540564,-0.303440937409622,
15.538931664499));
#14736=CARTESIAN_POINT('Ctrl Pts',(3.20790784723639,-0.308991747094943,
15.5385854096936));
#14737=CARTESIAN_POINT('Ctrl Pts',(3.20668325815074,-0.321478827744767,
15.5378081289579));
#14738=CARTESIAN_POINT('Ctrl Pts',(3.20598038983315,-0.328414215522219,
15.5373775643518));
#14739=CARTESIAN_POINT('Ctrl Pts',(3.20412279489459,-0.346169136152987,
15.5362780967607));
#14740=CARTESIAN_POINT('Ctrl Pts',(3.20293575601009,-0.356985302614786,
15.5356109721792));
#14741=CARTESIAN_POINT('Ctrl Pts',(3.19562998028578,-0.420582770401667,
15.5317029614291));
#14742=CARTESIAN_POINT('Ctrl Pts',(3.18826105332776,-0.473215647350341,
15.5285278329405));
#14743=CARTESIAN_POINT('Ctrl Pts',(3.17271221829946,-0.567269456737749,
15.5229217967447));
#14744=CARTESIAN_POINT('Ctrl Pts',(3.16501408194424,-0.608755771289282,
15.5204729487845));
#14745=CARTESIAN_POINT('Ctrl Pts',(3.1094337632759,-0.878629214621431,15.5046311665702));
#14746=CARTESIAN_POINT('Ctrl Pts',(3.03768038320479,-1.10139801172867,15.4919202563381));
#14747=CARTESIAN_POINT('Ctrl Pts',(2.90246880253642,-1.40407349179623,15.4731002291654));
#14748=CARTESIAN_POINT('Ctrl Pts',(2.85837451762567,-1.49179099612132,15.4674519833554));
#14749=CARTESIAN_POINT('Ctrl Pts',(2.78158821541533,-1.62859993871312,15.4582142128571));
#14750=CARTESIAN_POINT('Ctrl Pts',(2.75143186929814,-1.67904519594636,15.4547099616558));
#14751=CARTESIAN_POINT('Ctrl Pts',(2.71054796602091,-1.74337380881597,15.4500988674831));
#14752=CARTESIAN_POINT('Ctrl Pts',(2.70106166564937,-1.75803537309816,15.4490380825559));
#14753=CARTESIAN_POINT('Ctrl Pts',(2.68545328500086,-1.78173436594796,15.4473070207924));
#14754=CARTESIAN_POINT('Ctrl Pts',(2.67940353976657,-1.79081918773906,15.4466394670953));
#14755=CARTESIAN_POINT('Ctrl Pts',(2.66768869893312,-1.80821895724985,15.4453531998768));
#14756=CARTESIAN_POINT('Ctrl Pts',(2.66203057786545,-1.81653846384249,15.4447347558582));
#14757=CARTESIAN_POINT('Ctrl Pts',(2.64899643833406,-1.8355117377106,15.4433164037156));
#14758=CARTESIAN_POINT('Ctrl Pts',(2.64159497334884,-1.84614773473744,15.4425155293757));
#14759=CARTESIAN_POINT('Ctrl Pts',(2.62178031364328,-1.87425852015152,15.4403832752994));
#14760=CARTESIAN_POINT('Ctrl Pts',(2.6092567417693,-1.89165436405438,15.4390476603869));
#14761=CARTESIAN_POINT('Ctrl Pts',(2.5114539465005,-2.02468792196624,15.4287070273024));
#14762=CARTESIAN_POINT('Ctrl Pts',(2.41871275476403,-2.13461486975569,15.4194074157961));
#14763=CARTESIAN_POINT('Ctrl Pts',(2.17454436311254,-2.38761862145462,15.3960933350424));
#14764=CARTESIAN_POINT('Ctrl Pts',(2.0159867692261,-2.52292555332484,15.3818635396957));
#14765=CARTESIAN_POINT('Ctrl Pts',(1.7782498882188,-2.6889920233804,15.3624143870174));
#14766=CARTESIAN_POINT('Ctrl Pts',(1.70920548017092,-2.73339884891466,15.3569677881199));
#14767=CARTESIAN_POINT('Ctrl Pts',(1.61398892275687,-2.78961825197405,15.3497924053245));
#14768=CARTESIAN_POINT('Ctrl Pts',(1.58924891428097,-2.80378641186404,15.3479574960491));
#14769=CARTESIAN_POINT('Ctrl Pts',(1.55240655941075,-2.82424099841315,15.3452717844471));
#14770=CARTESIAN_POINT('Ctrl Pts',(1.54044775669879,-2.8307815292763,15.3444072036568));
#14771=CARTESIAN_POINT('Ctrl Pts',(1.51874519240997,-2.8424728773377,15.3428516232039));
#14772=CARTESIAN_POINT('Ctrl Pts',(1.5090158884109,-2.84764992137354,15.3421590950795));
#14773=CARTESIAN_POINT('Ctrl Pts',(1.49365846007077,-2.85572092674836,15.3410737897865));
#14774=CARTESIAN_POINT('Ctrl Pts',(1.4880481502379,-2.85864833636796,15.3406789462423));
#14775=CARTESIAN_POINT('Ctrl Pts',(1.48241445003584,-2.86156687168075,15.3402841217297));
#14776=CARTESIAN_POINT('Ctrl Pts',(1.48239970282712,-2.86157451131959,15.340283088218));
#14777=CARTESIAN_POINT('Ctrl Pts',(1.48237012412448,-2.8615898339703,15.3402810153106));
#14778=CARTESIAN_POINT('Ctrl Pts',(1.48235529270574,-2.86159751694159,15.3402799759204));
#14779=CARTESIAN_POINT('Ctrl Pts',(1.48232554508341,-2.86161292651109,15.3402778912213));
#14780=CARTESIAN_POINT('Ctrl Pts',(1.48231062880247,-2.86162065314769,15.3402768459072));
#14781=CARTESIAN_POINT('Ctrl Pts',(1.48228071093834,-2.86163615031079,15.3402747493245));
#14782=CARTESIAN_POINT('Ctrl Pts',(1.48226570923642,-2.86164392089709,15.3402736980477));
#14783=CARTESIAN_POINT('Ctrl Pts',(1.48223561981647,-2.86165950632426,15.3402715894902));
#14784=CARTESIAN_POINT('Ctrl Pts',(1.48222053217063,-2.86166732112601,15.3402705322146));
#14785=CARTESIAN_POINT('Ctrl Pts',(1.47723877439722,-2.86424762397113,15.3399214365737));
#14786=CARTESIAN_POINT('Ctrl Pts',(1.47226548688608,-2.86680714118089,15.3395742367904));
#14787=CARTESIAN_POINT('Ctrl Pts',(1.46088028386158,-2.87262912900951,15.3387823468855));
#14788=CARTESIAN_POINT('Ctrl Pts',(1.45446410261801,-2.87588308058095,15.338338195718));
#14789=CARTESIAN_POINT('Ctrl Pts',(1.43464353227989,-2.8858517389273,15.3369725118349));
#14790=CARTESIAN_POINT('Ctrl Pts',(1.42120291669234,-2.8924945312867,15.3360553729145));
#14791=CARTESIAN_POINT('Ctrl Pts',(1.28251169207302,-2.95984015026915,15.3266783291994));
#14792=CARTESIAN_POINT('Ctrl Pts',(1.15348307675403,-3.0124702134183,15.3186763870398));
#14793=CARTESIAN_POINT('Ctrl Pts',(0.837420529166947,-3.11809063574651,
15.2998557413592));
#14794=CARTESIAN_POINT('Ctrl Pts',(0.648225825811683,-3.1628415811601,15.2891887790513));
#14795=CARTESIAN_POINT('Ctrl Pts',(0.365094209550788,-3.20332406525421,
15.2729064436606));
#14796=CARTESIAN_POINT('Ctrl Pts',(0.273525426161436,-3.21243844413027,
15.2675972366621));
#14797=CARTESIAN_POINT('Ctrl Pts',(0.125662006465762,-3.22078818815127,
15.2588644583289));
#14798=CARTESIAN_POINT('Ctrl Pts',(0.0695567355263464,-3.22248797921902,
15.2555144952301));
#14799=CARTESIAN_POINT('Ctrl Pts',(-0.00374093713873998,-3.2227936162913,
15.2510790177485));
#14800=CARTESIAN_POINT('Ctrl Pts',(-0.0209200323831022,-3.22272788523748,
15.2500352465334));
#14801=CARTESIAN_POINT('Ctrl Pts',(-0.0489490639656499,-3.222396518736,
15.2483250669003));
#14802=CARTESIAN_POINT('Ctrl Pts',(-0.0597997776225279,-3.22221341888856,
15.2476612580956));
#14803=CARTESIAN_POINT('Ctrl Pts',(-0.080729277895057,-3.22175449125052,
15.2463773907639));
#14804=CARTESIAN_POINT('Ctrl Pts',(-0.0908081146579377,-3.22148616337669,
15.245757575577));
#14805=CARTESIAN_POINT('Ctrl Pts',(-0.113975566794437,-3.2207605704684,
15.2443292075589));
#14806=CARTESIAN_POINT('Ctrl Pts',(-0.127062918792827,-3.22027080982937,
15.2435196420365));
#14807=CARTESIAN_POINT('Ctrl Pts',(-0.162034273671959,-3.21874858092409,
15.2413490439872));
#14808=CARTESIAN_POINT('Ctrl Pts',(-0.183911044277697,-3.21757272218581,
15.2399835308476));
#14809=CARTESIAN_POINT('Ctrl Pts',(-0.369290110272627,-3.20571200294866,
15.2283455044269));
#14810=CARTESIAN_POINT('Ctrl Pts',(-0.531744731673002,-3.18279711704283,
15.21768579272));
#14811=CARTESIAN_POINT('Ctrl Pts',(-0.93998526669209,-3.09308113977407,
15.1898078442972));
#14812=CARTESIAN_POINT('Ctrl Pts',(-1.1808989702315,-3.00935143336284,15.1722623424249));
#14813=CARTESIAN_POINT('Ctrl Pts',(-1.4315227045649,-2.88746631098736,15.1540319917307));
#14814=CARTESIAN_POINT('Ctrl Pts',(-1.45345287857575,-2.87648981511593,
15.1524378008715));
#14815=CARTESIAN_POINT('Ctrl Pts',(-1.47525540626678,-2.86526421971528,
15.1508554073139));
#14816=CARTESIAN_POINT('Ctrl Pts',(-1.47525516809596,-2.86526434234368,
14.9065719799118));
#14817=CARTESIAN_POINT('Ctrl Pts',(-1.29829935559395,-2.95637460154743,
14.9200024838139));
#14818=CARTESIAN_POINT('Ctrl Pts',(-1.11317899372009,-3.0309507378844,14.933618121696));
#14819=CARTESIAN_POINT('Ctrl Pts',(-0.872313497822718,-3.1028859111795,
14.9500235892702));
#14820=CARTESIAN_POINT('Ctrl Pts',(-0.822036044264079,-3.11658295187011,
14.9533771319594));
#14821=CARTESIAN_POINT('Ctrl Pts',(-0.760373262704522,-3.131785450141,14.9573862220262));
#14822=CARTESIAN_POINT('Ctrl Pts',(-0.74928660001373,-3.13445644483712,
14.9581029764629));
#14823=CARTESIAN_POINT('Ctrl Pts',(-0.731910804305216,-3.13854515546142,
14.9592197245901));
#14824=CARTESIAN_POINT('Ctrl Pts',(-0.725631327811673,-3.14000291339942,
14.9596219630351));
#14825=CARTESIAN_POINT('Ctrl Pts',(-0.713900357826821,-3.14268914597708,
14.9603708374818));
#14826=CARTESIAN_POINT('Ctrl Pts',(-0.70845010232837,-3.14392227039492,
14.9607177292793));
#14827=CARTESIAN_POINT('Ctrl Pts',(-0.69601200923213,-3.14670241147349,
14.961507035731));
#14828=CARTESIAN_POINT('Ctrl Pts',(-0.689022221665945,-3.14824032814369,
14.9619489238048));
#14829=CARTESIAN_POINT('Ctrl Pts',(-0.670791855128358,-3.15218781219111,
14.9630972052505));
#14830=CARTESIAN_POINT('Ctrl Pts',(-0.659543288671677,-3.15456056777864,
14.9638015417738));
#14831=CARTESIAN_POINT('Ctrl Pts',(-0.586215240507551,-3.16961890466432,
14.9683672618144));
#14832=CARTESIAN_POINT('Ctrl Pts',(-0.523781173969791,-3.18053247477559,
14.9721346739348));
#14833=CARTESIAN_POINT('Ctrl Pts',(-0.428153420034432,-3.19435561081672,
14.9777785230944));
#14834=CARTESIAN_POINT('Ctrl Pts',(-0.395172938464891,-3.19860306908241,
14.9797022413641));
#14835=CARTESIAN_POINT('Ctrl Pts',(-0.123656983611868,-3.22930704116125,
14.9953948875432));
#14836=CARTESIAN_POINT('Ctrl Pts',(0.117090623299411,-3.22955367009755,
15.0084506593329));
#14837=CARTESIAN_POINT('Ctrl Pts',(0.44725348127025,-3.19289485256166,15.0273604278498));
#14838=CARTESIAN_POINT('Ctrl Pts',(0.538377760853058,-3.1787986189893,15.0326799729067));
#14839=CARTESIAN_POINT('Ctrl Pts',(0.683889636977428,-3.1498525607941,15.0414279761806));
#14840=CARTESIAN_POINT('Ctrl Pts',(0.738712252789463,-3.13744797860229,
15.0447824777654));
#14841=CARTESIAN_POINT('Ctrl Pts',(0.809835523821491,-3.11938764433208,
15.0492229038057));
#14842=CARTESIAN_POINT('Ctrl Pts',(0.826456555975406,-3.11502526387012,
15.0502669594897));
#14843=CARTESIAN_POINT('Ctrl Pts',(0.853514687341974,-3.10769174506031,
15.0519773367249));
#14844=CARTESIAN_POINT('Ctrl Pts',(0.863973210121691,-3.10480041088996,
15.0526410558339));
#14845=CARTESIAN_POINT('Ctrl Pts',(0.884116817806534,-3.0991219049677,15.0539245604343));
#14846=CARTESIAN_POINT('Ctrl Pts',(0.893803834905607,-3.09634200798374,
15.0545441017475));
#14847=CARTESIAN_POINT('Ctrl Pts',(0.916039227573804,-3.08984804654203,
15.0559715662417));
#14848=CARTESIAN_POINT('Ctrl Pts',(0.928578274402576,-3.08610291425306,
15.0567804995527));
#14849=CARTESIAN_POINT('Ctrl Pts',(0.962021814020893,-3.07589180458655,
15.0589487917748));
#14850=CARTESIAN_POINT('Ctrl Pts',(0.982883561545557,-3.06928920606619,
15.0603126181913));
#14851=CARTESIAN_POINT('Ctrl Pts',(1.15835274523631,-3.01178204994397,15.0718811047408));
#14852=CARTESIAN_POINT('Ctrl Pts',(1.30894244894143,-2.94945206014198,15.0824676666502));
#14853=CARTESIAN_POINT('Ctrl Pts',(1.67886041512723,-2.76241591858958,15.1101061793388));
#14854=CARTESIAN_POINT('Ctrl Pts',(1.88945805837219,-2.62287187205253,15.1274798689264));
#14855=CARTESIAN_POINT('Ctrl Pts',(2.12697498939373,-2.42190379463283,15.1478678258756));
#14856=CARTESIAN_POINT('Ctrl Pts',(2.17122233063687,-2.3823172012437,15.1517004821305));
#14857=CARTESIAN_POINT('Ctrl Pts',(2.22296249058293,-2.33338717496466,15.1561985241871));
#14858=CARTESIAN_POINT('Ctrl Pts',(2.23152615756828,-2.32519869284261,15.1569435603175));
#14859=CARTESIAN_POINT('Ctrl Pts',(2.24474895184221,-2.31241486807031,15.1580945197551));
#14860=CARTESIAN_POINT('Ctrl Pts',(2.24943946488151,-2.30785235110682,15.158502913516));
#14861=CARTESIAN_POINT('Ctrl Pts',(2.25810219319246,-2.2993745137522,15.1592573165035));
#14862=CARTESIAN_POINT('Ctrl Pts',(2.26207810609292,-2.29546320208016,15.1596036182839));
#14863=CARTESIAN_POINT('Ctrl Pts',(2.2710369494876,-2.28660404204402,15.160384078404));
#14864=CARTESIAN_POINT('Ctrl Pts',(2.27601386131793,-2.28165023093473,15.1608177570211));
#14865=CARTESIAN_POINT('Ctrl Pts',(2.29064004655196,-2.26699645659335,15.1620927248841));
#14866=CARTESIAN_POINT('Ctrl Pts',(2.30024392973773,-2.25725112386673,15.1629305046071));
#14867=CARTESIAN_POINT('Ctrl Pts',(2.36923969762895,-2.18634151118276,15.1689563304573));
#14868=CARTESIAN_POINT('Ctrl Pts',(2.42625149953874,-2.12289716652257,15.1739740825614));
#14869=CARTESIAN_POINT('Ctrl Pts',(2.64222566154837,-1.8624713134061,15.1934912494333));
#14870=CARTESIAN_POINT('Ctrl Pts',(2.78026869082285,-1.64932662340076,15.2072150144334));
#14871=CARTESIAN_POINT('Ctrl Pts',(2.93164122561744,-1.3415226797346,15.2267615279927));
#14872=CARTESIAN_POINT('Ctrl Pts',(2.96792671304666,-1.25921109209833,15.2319565669585));
#14873=CARTESIAN_POINT('Ctrl Pts',(3.02086127032029,-1.12408338171395,15.2405182810778));
#14874=CARTESIAN_POINT('Ctrl Pts',(3.03967535737743,-1.07216576834807,15.2438150545095));
#14875=CARTESIAN_POINT('Ctrl Pts',(3.06254886754779,-1.00359530998725,15.2481896447958));
#14876=CARTESIAN_POINT('Ctrl Pts',(3.06782305692954,-0.987355450817952,
15.2492271529717));
#14877=CARTESIAN_POINT('Ctrl Pts',(3.07623019802983,-0.960751035278142,
15.2509294982839));
#14878=CARTESIAN_POINT('Ctrl Pts',(3.07944045195426,-0.950411111783789,
15.2515917799493));
#14879=CARTESIAN_POINT('Ctrl Pts',(3.08554078223212,-0.930407108938799,
15.2528744065484));
#14880=CARTESIAN_POINT('Ctrl Pts',(3.08843771305024,-0.920745239519761,
15.2534945175237));
#14881=CARTESIAN_POINT('Ctrl Pts',(3.09500452235835,-0.898463849059415,
15.2549260324065));
#14882=CARTESIAN_POINT('Ctrl Pts',(3.09864264230274,-0.885835226531199,
15.2557384652094));
#14883=CARTESIAN_POINT('Ctrl Pts',(3.10818395560056,-0.851937370650033,
15.2579222581628));
#14884=CARTESIAN_POINT('Ctrl Pts',(3.11394596423509,-0.830629446884494,
15.2592981867979));
#14885=CARTESIAN_POINT('Ctrl Pts',(3.16288271534347,-0.641991930012578,
15.2715095081236));
#14886=CARTESIAN_POINT('Ctrl Pts',(3.19274570335591,-0.471527825870998,
15.2827776785713));
#14887=CARTESIAN_POINT('Ctrl Pts',(3.21818505364414,-0.198988189110471,
15.3010763308054));
#14888=CARTESIAN_POINT('Ctrl Pts',(3.22283890548999,-0.0980786939093705,
15.3079064951729));
#14889=CARTESIAN_POINT('Ctrl Pts',(3.22258736202469,0.183491806723148,15.3269679301503));
#14890=CARTESIAN_POINT('Ctrl Pts',(3.20724313318432,0.363789740046964,15.3391893359958));
#14891=CARTESIAN_POINT('Ctrl Pts',(3.1727669624573,0.565917522094113,15.3523170495701));
#14892=CARTESIAN_POINT('Ctrl Pts',(3.16839154439129,0.589921982582755,15.3538664215946));
#14893=CARTESIAN_POINT('Ctrl Pts',(3.16202291668154,0.622744132860431,15.3559695345655));
#14894=CARTESIAN_POINT('Ctrl Pts',(3.16026474166081,0.631605848524153,15.3565358138219));
#14895=CARTESIAN_POINT('Ctrl Pts',(3.15740969311579,0.64568569841765,15.3574329553973));
#14896=CARTESIAN_POINT('Ctrl Pts',(3.15633711019876,0.650908625761379,15.357765183688));
#14897=CARTESIAN_POINT('Ctrl Pts',(3.15409268895684,0.661701799929635,15.35845052617));
#14898=CARTESIAN_POINT('Ctrl Pts',(3.15291905402558,0.667271610174321,15.3588035257909));
#14899=CARTESIAN_POINT('Ctrl Pts',(3.15008150469355,0.680563349111567,15.3596443734835));
#14900=CARTESIAN_POINT('Ctrl Pts',(3.14840393111076,0.688282389750243,15.3601314406247));
#14901=CARTESIAN_POINT('Ctrl Pts',(3.1426210158562,0.714427808008232,15.3617772136713));
#14902=CARTESIAN_POINT('Ctrl Pts',(3.13838206541777,0.732824667304999,15.3629285142256));
#14903=CARTESIAN_POINT('Ctrl Pts',(3.11372949269161,0.835676615343761,15.3693328080026));
#14904=CARTESIAN_POINT('Ctrl Pts',(3.09006683023854,0.919323945272005,15.3744191545012));
#14905=CARTESIAN_POINT('Ctrl Pts',(2.99287163818115,1.21646724982702,15.3923770665024));
#14906=CARTESIAN_POINT('Ctrl Pts',(2.90034430817645,1.42305548734032,15.4046934005287));
#14907=CARTESIAN_POINT('Ctrl Pts',(2.71127995477215,1.74865833806095,15.426035671086));
#14908=CARTESIAN_POINT('Ctrl Pts',(2.62653350528946,1.87354160518883,15.4347585829232));
#14909=CARTESIAN_POINT('Ctrl Pts',(2.5200063902329,2.00901780520061,15.4451270220551));
#14910=CARTESIAN_POINT('Ctrl Pts',(2.50647583767706,2.02587353718917,15.4464339558098));
#14911=CARTESIAN_POINT('Ctrl Pts',(2.48453227643423,2.05265344040299,15.4485383481939));
#14912=CARTESIAN_POINT('Ctrl Pts',(2.47622680021474,2.06266517039267,15.4493314567514));
#14913=CARTESIAN_POINT('Ctrl Pts',(2.46138735199161,2.08033439386671,15.4507426841233));
#14914=CARTESIAN_POINT('Ctrl Pts',(2.45487765215542,2.08801211589994,15.4513598023895));
#14915=CARTESIAN_POINT('Ctrl Pts',(2.44125352746493,2.10392900893504,15.4526473947996));
#14916=CARTESIAN_POINT('Ctrl Pts',(2.43413312286338,2.11216287144763,15.4533181123987));
#14917=CARTESIAN_POINT('Ctrl Pts',(2.41556145657357,2.13342005910516,15.4550618759026));
#14918=CARTESIAN_POINT('Ctrl Pts',(2.40404666331769,2.14638717866029,15.456137572424));
#14919=CARTESIAN_POINT('Ctrl Pts',(2.35379660027261,2.20206348717016,15.4608089817069));
#14920=CARTESIAN_POINT('Ctrl Pts',(2.31402570509347,2.24381959628616,15.4644485105213));
#14921=CARTESIAN_POINT('Ctrl Pts',(2.20543048901519,2.3518764086763,15.4742439138608));
#14922=CARTESIAN_POINT('Ctrl Pts',(2.13474513109526,2.41621743724114,15.4804779808176));
#14923=CARTESIAN_POINT('Ctrl Pts',(1.95208527064258,2.56820385871222,15.4962241804197));
#14924=CARTESIAN_POINT('Ctrl Pts',(1.83697361706025,2.65176004065423,15.5058415686161));
#14925=CARTESIAN_POINT('Ctrl Pts',(1.5591531104243,2.82662841058469,15.5280611769739));
#14926=CARTESIAN_POINT('Ctrl Pts',(1.3932548539505,2.91198280314926,15.5406286829045));
#14927=CARTESIAN_POINT('Ctrl Pts',(1.20732307380647,2.98809365086722,15.5533627456282));
#14928=CARTESIAN_POINT('Ctrl Pts',(1.19371161897893,2.99355729205417,15.5542873673402));
#14929=CARTESIAN_POINT('Ctrl Pts',(1.17342952121593,3.00153819536411,15.5556533565314));
#14930=CARTESIAN_POINT('Ctrl Pts',(1.16678728527009,3.00412646417263,15.5560988423265));
#14931=CARTESIAN_POINT('Ctrl Pts',(1.15492540928409,3.00870338504555,15.5568910086825));
#14932=CARTESIAN_POINT('Ctrl Pts',(1.1497091489723,3.01070052223715,15.5572381934432));
#14933=CARTESIAN_POINT('Ctrl Pts',(1.13844333497434,3.01498028865391,15.557985490875));
#14934=CARTESIAN_POINT('Ctrl Pts',(1.13239211397071,3.01725827032956,15.5583853238786));
#14935=CARTESIAN_POINT('Ctrl Pts',(1.11556693076002,3.02353436335561,15.5594928136228));
#14936=CARTESIAN_POINT('Ctrl Pts',(1.10477825144893,3.02749312927487,15.560198154615));
#14937=CARTESIAN_POINT('Ctrl Pts',(1.04369248128592,3.04953774004932,15.5641659427037));
#14938=CARTESIAN_POINT('Ctrl Pts',(0.992969491682906,3.06642899561575,15.5673618124813));
#14939=CARTESIAN_POINT('Ctrl Pts',(0.696910994248216,3.15690173020031,15.5855746910391));
#14940=CARTESIAN_POINT('Ctrl Pts',(0.443902654072817,3.20229491667954,15.5994687165154));
#14941=CARTESIAN_POINT('Ctrl Pts',(0.0235701095507269,3.22687877549539,
15.6232457044706));
#14942=CARTESIAN_POINT('Ctrl Pts',(-0.141500873429374,3.22385934761599,
15.6327437279834));
#14943=CARTESIAN_POINT('Ctrl Pts',(-0.32742865069139,3.20614857736987,15.6439771753053));
#14944=CARTESIAN_POINT('Ctrl Pts',(-0.349231582890425,3.20384698239396,
15.645302562535));
#14945=CARTESIAN_POINT('Ctrl Pts',(-0.384020645301622,3.19981519546685,
15.6474310076476));
#14946=CARTESIAN_POINT('Ctrl Pts',(-0.39702289179336,3.19822794006303,15.6482295539525));
#14947=CARTESIAN_POINT('Ctrl Pts',(-0.420013019274603,3.19527905387204,
15.6496470612445));
#14948=CARTESIAN_POINT('Ctrl Pts',(-0.430004923536417,3.19394973826159,
15.6502649912669));
#14949=CARTESIAN_POINT('Ctrl Pts',(-0.450734269057387,3.19109288578607,
15.6515508841718));
#14950=CARTESIAN_POINT('Ctrl Pts',(-0.461470550694857,3.18955798085794,
15.6522190736363));
#14951=CARTESIAN_POINT('Ctrl Pts',(-0.489173110943545,3.18545470527882,
15.6539489445611));
#14952=CARTESIAN_POINT('Ctrl Pts',(-0.506126823327988,3.18280499437272,
15.6550131977779));
#14953=CARTESIAN_POINT('Ctrl Pts',(-0.578295537855609,3.17093448886617,
15.6595679005907));
#14954=CARTESIAN_POINT('Ctrl Pts',(-0.633283649195949,3.16041175280476,
15.6630994983137));
#14955=CARTESIAN_POINT('Ctrl Pts',(-0.777517851192644,3.12889529467526,
15.672531069072));
#14956=CARTESIAN_POINT('Ctrl Pts',(-0.866185523354872,3.10551765598511,
15.6785022167234));
#14957=CARTESIAN_POINT('Ctrl Pts',(-1.18798919520071,3.00581833787166,15.7007860758781));
#14958=CARTESIAN_POINT('Ctrl Pts',(-1.4131737711651,2.90674848371405,15.7176609816698));
#14959=CARTESIAN_POINT('Ctrl Pts',(-1.70275000060226,2.73767771385391,15.7399541547865));
#14960=CARTESIAN_POINT('Ctrl Pts',(-1.77863327340503,2.68899679121665,15.7458483020379));
#14961=CARTESIAN_POINT('Ctrl Pts',(-1.86372628726903,2.62922689040783,15.7524344408872));
#14962=CARTESIAN_POINT('Ctrl Pts',(-1.87501828518518,2.6211860219332,15.7533079203244));
#14963=CARTESIAN_POINT('Ctrl Pts',(-1.89198315206013,2.60893985493122,15.7546190042539));
#14964=CARTESIAN_POINT('Ctrl Pts',(-1.8976944874296,2.60478848449593,15.7550601797469));
#14965=CARTESIAN_POINT('Ctrl Pts',(-1.90789502347874,2.59732271356847,15.7558476810571));
#14966=CARTESIAN_POINT('Ctrl Pts',(-1.91238928470421,2.59401540557045,15.7561944869903));
#14967=CARTESIAN_POINT('Ctrl Pts',(-1.92211180495464,2.58682164226112,15.7569443831182));
#14968=CARTESIAN_POINT('Ctrl Pts',(-1.92733686119527,2.58293101434563,15.757347175317));
#14969=CARTESIAN_POINT('Ctrl Pts',(-1.94192483542134,2.57199975281724,15.7584712490166));
#14970=CARTESIAN_POINT('Ctrl Pts',(-1.95126132753185,2.56492378764273,15.7591901001729));
#14971=CARTESIAN_POINT('Ctrl Pts',(-2.00584067779629,2.52308854842995,15.7633903640214));
#14972=CARTESIAN_POINT('Ctrl Pts',(-2.05019576566972,2.48718131586969,15.766795707816));
#14973=CARTESIAN_POINT('Ctrl Pts',(-2.2862224661448,2.28550076884227,15.7850162812929));
#14974=CARTESIAN_POINT('Ctrl Pts',(-2.45879921188954,2.09872822355117,15.7987688288909));
#14975=CARTESIAN_POINT('Ctrl Pts',(-2.70387232571146,1.76124059799048,15.8223291000407));
#14976=CARTESIAN_POINT('Ctrl Pts',(-2.78978619625217,1.62172024955394,15.8317592270355));
#14977=CARTESIAN_POINT('Ctrl Pts',(-2.8747619970212,1.45682552061323,15.8429167063826));
#14978=CARTESIAN_POINT('Ctrl Pts',(-2.8845948042191,1.43725777654506,15.8442406181248));
#14979=CARTESIAN_POINT('Ctrl Pts',(-2.8999858395167,1.40583465695759,15.846367140896));
#14980=CARTESIAN_POINT('Ctrl Pts',(-2.9056726763958,1.39404276900303,15.8471652533616));
#14981=CARTESIAN_POINT('Ctrl Pts',(-2.91561019502526,1.37311191689143,15.8485822585399));
#14982=CARTESIAN_POINT('Ctrl Pts',(-2.91989017239619,1.36398699521775,15.8492001227182));
#14983=CARTESIAN_POINT('Ctrl Pts',(-2.92868799083181,1.34499885034228,15.8504861458784));
#14984=CARTESIAN_POINT('Ctrl Pts',(-2.93319896703917,1.33513260398243,15.8511545327703));
#14985=CARTESIAN_POINT('Ctrl Pts',(-2.94472211309302,1.30958931635942,15.8528854893365));
#14986=CARTESIAN_POINT('Ctrl Pts',(-2.95165887018737,1.2938788183222,15.853950636899));
#14987=CARTESIAN_POINT('Ctrl Pts',(-2.98072193289662,1.22660610482275,15.8585143536885));
#14988=CARTESIAN_POINT('Ctrl Pts',(-3.00162409149051,1.17452882147131,15.8620542738914));
#14989=CARTESIAN_POINT('Ctrl Pts',(-3.05316937879825,1.03572727249111,15.8715137155713));
#14990=CARTESIAN_POINT('Ctrl Pts',(-3.08147630686023,0.948195910633212,
15.8775049358458));
#14991=CARTESIAN_POINT('Ctrl Pts',(-3.17066090111398,0.625937041287872,
15.8996251215533));
#14992=CARTESIAN_POINT('Ctrl Pts',(-3.20874665667649,0.385768970806537,
15.9162982716766));
#14993=CARTESIAN_POINT('Ctrl Pts',(-3.22366332413373,0.0513683403728577,
15.9385707444958));
#14994=CARTESIAN_POINT('Ctrl Pts',(-3.22381211465226,-0.0410223082529205,
15.9446158687836));
#14995=CARTESIAN_POINT('Ctrl Pts',(-3.21941550923888,-0.147226390992114,
15.9513488147855));
#14996=CARTESIAN_POINT('Ctrl Pts',(-3.21874865074398,-0.16114890996879,
15.9522271498805));
#14997=CARTESIAN_POINT('Ctrl Pts',(-3.21760704438148,-0.182133335606764,
15.9535440725008));
#14998=CARTESIAN_POINT('Ctrl Pts',(-3.21719933644135,-0.189198509149784,
15.9539862774193));
#14999=CARTESIAN_POINT('Ctrl Pts',(-3.21642846261519,-0.201833242083144,
15.9547748879391));
#15000=CARTESIAN_POINT('Ctrl Pts',(-3.2160740993547,-0.207403234703026,
15.955121779415));
#15001=CARTESIAN_POINT('Ctrl Pts',(-3.21527554960807,-0.219460667715434,
15.955871032363));
#15002=CARTESIAN_POINT('Ctrl Pts',(-3.21482619985199,-0.225947673348353,
15.9562731003021));
#15003=CARTESIAN_POINT('Ctrl Pts',(-3.21351626641155,-0.244062948751036,
15.9573931084661));
#15004=CARTESIAN_POINT('Ctrl Pts',(-3.21261219507871,-0.255688113063449,
15.9581086466714));
#15005=CARTESIAN_POINT('Ctrl Pts',(-3.20698828117226,-0.32325808286155,
15.9622503003687));
#15006=CARTESIAN_POINT('Ctrl Pts',(-3.20086994652675,-0.379080593150567,
15.9656028030611));
#15007=CARTESIAN_POINT('Ctrl Pts',(-3.1590247127134,-0.686461573874854,
15.9838202624834));
#15008=CARTESIAN_POINT('Ctrl Pts',(-3.09510251850728,-0.933292194484601,
15.9976076342173));
#15009=CARTESIAN_POINT('Ctrl Pts',(-2.94331132836656,-1.3228453379133,16.0212223361923));
#15010=CARTESIAN_POINT('Ctrl Pts',(-2.8722180485136,-1.4708345890606,16.0306703779535));
#15011=CARTESIAN_POINT('Ctrl Pts',(-2.77921972874936,-1.63172764995896,
16.0418478970592));
#15012=CARTESIAN_POINT('Ctrl Pts',(-2.76806455602381,-1.65058050445976,
16.0431721998444));
#15013=CARTESIAN_POINT('Ctrl Pts',(-2.74993609937473,-1.6805179117041,16.045299232101));
#15014=CARTESIAN_POINT('Ctrl Pts',(-2.74308582498165,-1.69167643213656,
16.0460974595615));
#15015=CARTESIAN_POINT('Ctrl Pts',(-2.73084233864018,-1.7113501316738,16.0475145978139));
#15016=CARTESIAN_POINT('Ctrl Pts',(-2.72547678991981,-1.71988238424385,
16.0481324794272));
#15017=CARTESIAN_POINT('Ctrl Pts',(-2.71425358809905,-1.73754501999016,
16.0494184679731));
#15018=CARTESIAN_POINT('Ctrl Pts',(-2.70838969121832,-1.74667126640836,
16.0500868024634));
#15019=CARTESIAN_POINT('Ctrl Pts',(-2.69312560497364,-1.77016576818989,
16.0518174708897));
#15020=CARTESIAN_POINT('Ctrl Pts',(-2.68365655786252,-1.78448867524749,
16.0528823810858));
#15021=CARTESIAN_POINT('Ctrl Pts',(-2.64277638724699,-1.84526282291843,
16.0574437037481));
#15022=CARTESIAN_POINT('Ctrl Pts',(-2.61027182183478,-1.89096332523365,
16.0609814132607));
#15023=CARTESIAN_POINT('Ctrl Pts',(-2.5214034177145,-2.00924974839013,16.0704334486528));
#15024=CARTESIAN_POINT('Ctrl Pts',(-2.46310191021845,-2.08030916168714,
16.0764193338204));
#15025=CARTESIAN_POINT('Ctrl Pts',(-2.23967647796577,-2.33004858550497,
16.098586514666));
#15026=CARTESIAN_POINT('Ctrl Pts',(-2.05752235845153,-2.49236109717652,
16.1153170513016));
#15027=CARTESIAN_POINT('Ctrl Pts',(-1.78395280315852,-2.68552376252843,
16.1375948117975));
#15028=CARTESIAN_POINT('Ctrl Pts',(-1.70681720881273,-2.73519722936382,
16.1435963659005));
#15029=CARTESIAN_POINT('Ctrl Pts',(-1.61564947927401,-2.78854585619781,
16.1502869944425));
#15030=CARTESIAN_POINT('Ctrl Pts',(-1.60359263998892,-2.79549671675951,
16.1511639570257));
#15031=CARTESIAN_POINT('Ctrl Pts',(-1.58534117400641,-2.80586188916755,
16.1524792295715));
#15032=CARTESIAN_POINT('Ctrl Pts',(-1.57917989842218,-2.80933416128601,
16.1529211437864));
#15033=CARTESIAN_POINT('Ctrl Pts',(-1.56813622670317,-2.8155101639498,16.1537094407496));
#15034=CARTESIAN_POINT('Ctrl Pts',(-1.56325820898956,-2.81822151052739,
16.1540563077467));
#15035=CARTESIAN_POINT('Ctrl Pts',(-1.55267842112873,-2.82406614806578,
16.1548057408546));
#15036=CARTESIAN_POINT('Ctrl Pts',(-1.54697421625504,-2.82719484013737,
16.1552080121776));
#15037=CARTESIAN_POINT('Ctrl Pts',(-1.53100694205595,-2.83588991654829,
16.1563291615641));
#15038=CARTESIAN_POINT('Ctrl Pts',(-1.52072291767915,-2.84141790181805,
16.1570456296722));
#15039=CARTESIAN_POINT('Ctrl Pts',(-1.4987287032758,-2.85308686598192,16.1585664433318));
#15040=CARTESIAN_POINT('Ctrl Pts',(-1.48701064947239,-2.85921172865691,
16.1593698163877));
#15041=CARTESIAN_POINT('Ctrl Pts',(-1.47525540483048,-2.8652642204548,16.1601692104994));
#15042=CARTESIAN_POINT('Origin',(0.,0.,4.68922655072688));
#15043=CARTESIAN_POINT('',(-1.47525542042047,-2.86526421242789,17.6559915606006));
#15044=CARTESIAN_POINT('',(-1.47525540448703,-2.86526422063163,17.4058265726261));
#15045=CARTESIAN_POINT('',(-1.47525540501186,-2.86526422036142,4.68922655072688));
#15046=CARTESIAN_POINT('Ctrl Pts',(-1.47525542042047,-2.86526421242789,
17.6559915606006));
#15047=CARTESIAN_POINT('Ctrl Pts',(-1.50921165810786,-2.84778096481389,
17.6537750309423));
#15048=CARTESIAN_POINT('Ctrl Pts',(-1.54285734213704,-2.82969397413309,
17.6515415727465));
#15049=CARTESIAN_POINT('Ctrl Pts',(-1.62480603952861,-2.78374410403791,
17.646000501543));
#15050=CARTESIAN_POINT('Ctrl Pts',(-1.67271742503822,-2.75522081740872,
17.6426722865387));
#15051=CARTESIAN_POINT('Ctrl Pts',(-1.73435661497109,-2.71632443089516,
17.6382616055638));
#15052=CARTESIAN_POINT('Ctrl Pts',(-1.74877696519889,-2.70706305617555,
17.6372202923261));
#15053=CARTESIAN_POINT('Ctrl Pts',(-1.77219919325204,-2.69175503315924,
17.6355131281553));
#15054=CARTESIAN_POINT('Ctrl Pts',(-1.7812457537505,-2.68577711273711,17.6348498591701));
#15055=CARTESIAN_POINT('Ctrl Pts',(-1.79864828132301,-2.6741510137598,17.6335663236865));
#15056=CARTESIAN_POINT('Ctrl Pts',(-1.80700825145836,-2.66850903310619,
17.6329462966981));
#15057=CARTESIAN_POINT('Ctrl Pts',(-1.82617989108537,-2.65543906609416,
17.6315164177203));
#15058=CARTESIAN_POINT('Ctrl Pts',(-1.83697291319907,-2.64798416466915,
17.6307055460363));
#15059=CARTESIAN_POINT('Ctrl Pts',(-1.86572839785879,-2.6278619093799,17.6285291654409));
#15060=CARTESIAN_POINT('Ctrl Pts',(-1.88360703757233,-2.61507651105942,
17.6271591383215));
#15061=CARTESIAN_POINT('Ctrl Pts',(-2.03494700546774,-2.50449287652071,
17.6154152396306));
#15062=CARTESIAN_POINT('Ctrl Pts',(-2.16080388928503,-2.39674891031488,
17.6046462416823));
#15063=CARTESIAN_POINT('Ctrl Pts',(-2.46047210908902,-2.09734577721614,
17.5763805141774));
#15064=CARTESIAN_POINT('Ctrl Pts',(-2.62052426332478,-1.89357626754913,
17.5585461374716));
#15065=CARTESIAN_POINT('Ctrl Pts',(-2.78103111943354,-1.62929019396027,
17.5383793224932));
#15066=CARTESIAN_POINT('Ctrl Pts',(-2.80647773859535,-1.58505647276577,
17.5350967508596));
#15067=CARTESIAN_POINT('Ctrl Pts',(-2.83628163111878,-1.53027857913858,
17.5311605179076));
#15068=CARTESIAN_POINT('Ctrl Pts',(-2.8416459504201,-1.52029415649738,17.5304481923698));
#15069=CARTESIAN_POINT('Ctrl Pts',(-2.84997203293764,-1.50459906639595,
17.529336722765));
#15070=CARTESIAN_POINT('Ctrl Pts',(-2.85296949990192,-1.49890759337402,
17.5289353689053));
#15071=CARTESIAN_POINT('Ctrl Pts',(-2.85854106015948,-1.48825127055043,
17.5281871210898));
#15072=CARTESIAN_POINT('Ctrl Pts',(-2.8611192425356,-1.4832887505504,17.5278399773761));
#15073=CARTESIAN_POINT('Ctrl Pts',(-2.86697987309817,-1.47193599624572,
17.527048768643));
#15074=CARTESIAN_POINT('Ctrl Pts',(-2.87025387466152,-1.46554149280782,
17.5266052390386));
#15075=CARTESIAN_POINT('Ctrl Pts',(-2.88027067095304,-1.44581521036791,
17.5252433661779));
#15076=CARTESIAN_POINT('Ctrl Pts',(-2.88694227941604,-1.43244722616778,
17.5243293813019));
#15077=CARTESIAN_POINT('Ctrl Pts',(-2.94984664937029,-1.30418022979127,
17.515640029013));
#15078=CARTESIAN_POINT('Ctrl Pts',(-2.99929145139667,-1.186060789108,17.5082507005718));
#15079=CARTESIAN_POINT('Ctrl Pts',(-3.10606658832164,-0.881202469696688,
17.4899458601504));
#15080=CARTESIAN_POINT('Ctrl Pts',(-3.15369916777444,-0.691629844502033,
17.4792325375991));
#15081=CARTESIAN_POINT('Ctrl Pts',(-3.19918615115247,-0.401345476656031,
17.4625559673734));
#15082=CARTESIAN_POINT('Ctrl Pts',(-3.20998075155483,-0.303136109167712,
17.4568734339982));
#15083=CARTESIAN_POINT('Ctrl Pts',(-3.21999659180236,-0.145683515958993,
17.4475847842714));
#15084=CARTESIAN_POINT('Ctrl Pts',(-3.22212452373348,-0.0866869307072219,
17.4440651748651));
#15085=CARTESIAN_POINT('Ctrl Pts',(-3.22278138940034,-0.0101780825974663,
17.4394366268578));
#15086=CARTESIAN_POINT('Ctrl Pts',(-3.22278916282771,0.00731234864302059,
17.4383741879552));
#15087=CARTESIAN_POINT('Ctrl Pts',(-3.2225705180606,0.0357223442217228,
17.4366410953533));
#15088=CARTESIAN_POINT('Ctrl Pts',(-3.22243096348964,0.0466423697049451,
17.4359731769186));
#15089=CARTESIAN_POINT('Ctrl Pts',(-3.22205623909723,0.067619118490116,
17.4346866672659));
#15090=CARTESIAN_POINT('Ctrl Pts',(-3.22182948141615,0.0776758785427716,
17.4340683480629));
#15091=CARTESIAN_POINT('Ctrl Pts',(-3.22120325256674,0.100671440888486,
17.4326509300296));
#15092=CARTESIAN_POINT('Ctrl Pts',(-3.22077290153226,0.113609164482866,
17.4318508693236));
#15093=CARTESIAN_POINT('Ctrl Pts',(-3.21942469995066,0.147917965458351,
17.4297221931728));
#15094=CARTESIAN_POINT('Ctrl Pts',(-3.21837201330022,0.169282815227498,
17.4283893651131));
#15095=CARTESIAN_POINT('Ctrl Pts',(-3.20870195811495,0.332471987942826,
17.4181518634995));
#15096=CARTESIAN_POINT('Ctrl Pts',(-3.19092777737306,0.473577916294351,
17.4089593489613));
#15097=CARTESIAN_POINT('Ctrl Pts',(-3.12470239215704,0.815370413700592,
17.3858862865471));
#15098=CARTESIAN_POINT('Ctrl Pts',(-3.06617979775527,1.01347193703297,17.3717912585527));
#15099=CARTESIAN_POINT('Ctrl Pts',(-2.9575366076154,1.28306250278939,17.3522809492271));
#15100=CARTESIAN_POINT('Ctrl Pts',(-2.92284145821654,1.36024703184216,17.3466605664948));
#15101=CARTESIAN_POINT('Ctrl Pts',(-2.86564318331968,1.47516871159003,17.3383257400908));
#15102=CARTESIAN_POINT('Ctrl Pts',(-2.84534172006683,1.51395658115092,17.3355188041328));
#15103=CARTESIAN_POINT('Ctrl Pts',(-2.81905402971866,1.56178376732926,17.3320765641349));
#15104=CARTESIAN_POINT('Ctrl Pts',(-2.81380530123187,1.57122051060876,17.331398310369));
#15105=CARTESIAN_POINT('Ctrl Pts',(-2.80541236291031,1.58613331841402,17.3303281693956));
#15106=CARTESIAN_POINT('Ctrl Pts',(-2.80229937544328,1.59162672815316,17.3299343304625));
#15107=CARTESIAN_POINT('Ctrl Pts',(-2.79638800600752,1.60198726618452,17.3291922998867));
#15108=CARTESIAN_POINT('Ctrl Pts',(-2.79359308624969,1.60685616969134,17.3288439047019));
#15109=CARTESIAN_POINT('Ctrl Pts',(-2.78715679745384,1.61800098682562,17.3280471329418));
#15110=CARTESIAN_POINT('Ctrl Pts',(-2.78350695036536,1.62427191893873,17.3275993121445));
#15111=CARTESIAN_POINT('Ctrl Pts',(-2.77372284889367,1.64095249985227,17.3264093159857));
#15112=CARTESIAN_POINT('Ctrl Pts',(-2.76755111091637,1.65134018552999,17.325669507383));
#15113=CARTESIAN_POINT('Ctrl Pts',(-2.72262064223818,1.72600345866916,17.3203592256973));
#15114=CARTESIAN_POINT('Ctrl Pts',(-2.68168200504866,1.78894792710155,17.3159210424777));
#15115=CARTESIAN_POINT('Ctrl Pts',(-2.62555670430001,1.8689793856393,17.3102510468129));
#15116=CARTESIAN_POINT('Ctrl Pts',(-2.6123385216607,1.8874107759113,17.3089433107318));
#15117=CARTESIAN_POINT('Ctrl Pts',(-2.4584914079385,2.0972219026021,17.2940161264704));
#15118=CARTESIAN_POINT('Ctrl Pts',(-2.29731330288381,2.27263780219091,17.281088912887));
#15119=CARTESIAN_POINT('Ctrl Pts',(-2.01352783553751,2.52015006664786,17.2596555093744));
#15120=CARTESIAN_POINT('Ctrl Pts',(-1.90294799208682,2.60465593818988,17.2515737842408));
#15121=CARTESIAN_POINT('Ctrl Pts',(-1.76859530644773,2.69419592124285,17.2418482914132));
#15122=CARTESIAN_POINT('Ctrl Pts',(-1.74979498380323,2.70644388367541,17.2404896232876));
#15123=CARTESIAN_POINT('Ctrl Pts',(-1.72074526909365,2.72493987269632,17.2383929657998));
#15124=CARTESIAN_POINT('Ctrl Pts',(-1.71058606534811,2.7313287787849,17.2376602317155));
#15125=CARTESIAN_POINT('Ctrl Pts',(-1.69202028194145,2.74286019332181,17.2363219761966));
#15126=CARTESIAN_POINT('Ctrl Pts',(-1.6836253143024,2.74802119209754,17.235717148532));
#15127=CARTESIAN_POINT('Ctrl Pts',(-1.66527474077098,2.75918697636374,17.2343956337175));
#15128=CARTESIAN_POINT('Ctrl Pts',(-1.65531007612173,2.76517653667787,17.2336783978784));
#15129=CARTESIAN_POINT('Ctrl Pts',(-1.6279948535519,2.78139461082274,17.2317131866269));
#15130=CARTESIAN_POINT('Ctrl Pts',(-1.61058069675148,2.79151446599061,17.2304612762955));
#15131=CARTESIAN_POINT('Ctrl Pts',(-1.52252644242169,2.84158705472261,17.2241348761914));
#15132=CARTESIAN_POINT('Ctrl Pts',(-1.45049526646545,2.87902159332317,17.2189709655042));
#15133=CARTESIAN_POINT('Ctrl Pts',(-1.34046502149274,2.93102644078837,17.2110937631221));
#15134=CARTESIAN_POINT('Ctrl Pts',(-1.30347428291919,2.94766298141163,17.2084475437418));
#15135=CARTESIAN_POINT('Ctrl Pts',(-1.06322567157239,3.05030790325585,17.1912788387716));
#15136=CARTESIAN_POINT('Ctrl Pts',(-0.851911904511612,3.11593582546824,
17.1762035513759));
#15137=CARTESIAN_POINT('Ctrl Pts',(-0.544461007892324,3.177785214158,17.1551002312699));
#15138=CARTESIAN_POINT('Ctrl Pts',(-0.452582595593248,3.19216667970799,
17.1489036808425));
#15139=CARTESIAN_POINT('Ctrl Pts',(-0.313933301531223,3.2077611523098,17.1398285019107));
#15140=CARTESIAN_POINT('Ctrl Pts',(-0.267551193009791,3.21196242587454,
17.1368386985903));
#15141=CARTESIAN_POINT('Ctrl Pts',(-0.210102238954865,3.215912926075,17.1332055500954));
#15142=CARTESIAN_POINT('Ctrl Pts',(-0.199108918942868,3.21661227778708,
17.132513483837));
#15143=CARTESIAN_POINT('Ctrl Pts',(-0.181760687197741,3.21762662419329,
17.1314265770773));
#15144=CARTESIAN_POINT('Ctrl Pts',(-0.17540818032777,3.21797918142222,17.1310296818193));
#15145=CARTESIAN_POINT('Ctrl Pts',(-0.163458183963159,3.21860690221043,
17.1302851928531));
#15146=CARTESIAN_POINT('Ctrl Pts',(-0.157861088935017,3.21888627415952,
17.12993737663));
#15147=CARTESIAN_POINT('Ctrl Pts',(-0.14509619672751,3.21949004293042,17.1291461212268));
#15148=CARTESIAN_POINT('Ctrl Pts',(-0.137928035903201,3.21980510312202,
17.1287032104826));
#15149=CARTESIAN_POINT('Ctrl Pts',(-0.118959966937395,3.22057534158232,
17.1275348179507));
#15150=CARTESIAN_POINT('Ctrl Pts',(-0.107158378421279,3.22098961445206,
17.1268115687951));
#15151=CARTESIAN_POINT('Ctrl Pts',(-0.026006712394669,3.22339177771076,
17.1218620924443));
#15152=CARTESIAN_POINT('Ctrl Pts',(0.0433951599804932,3.22320482494652,
17.1177487467012));
#15153=CARTESIAN_POINT('Ctrl Pts',(0.355820978909821,3.21226845548931,17.099555329279));
#15154=CARTESIAN_POINT('Ctrl Pts',(0.597171840884709,3.17626872740986,17.0863307876468));
#15155=CARTESIAN_POINT('Ctrl Pts',(0.987807694218107,3.07185619275385,17.0634639638808));
#15156=CARTESIAN_POINT('Ctrl Pts',(1.14006782402883,3.0186585980268,17.0541658570101));
#15157=CARTESIAN_POINT('Ctrl Pts',(1.30888366047899,2.94507640245219,17.0430789357183));
#15158=CARTESIAN_POINT('Ctrl Pts',(1.32996475254857,2.9356166587567,17.0416803375862));
#15159=CARTESIAN_POINT('Ctrl Pts',(1.36196532970585,2.92084156095532,17.0395349133715));
#15160=CARTESIAN_POINT('Ctrl Pts',(1.37295979951491,2.91568968960838,17.0387937367698));
#15161=CARTESIAN_POINT('Ctrl Pts',(1.39204620469512,2.90661414655783,17.0374998388999));
#15162=CARTESIAN_POINT('Ctrl Pts',(1.40015136684782,2.90271848105921,17.0369480971851));
#15163=CARTESIAN_POINT('Ctrl Pts',(1.41831904797964,2.89389256911169,17.035706187806));
#15164=CARTESIAN_POINT('Ctrl Pts',(1.42837233382647,2.88894368139962,17.0350153732124));
#15165=CARTESIAN_POINT('Ctrl Pts',(1.45520064148423,2.87556275432808,17.0331621189701));
#15166=CARTESIAN_POINT('Ctrl Pts',(1.47192793466289,2.86703648252909,17.0319963778376));
#15167=CARTESIAN_POINT('Ctrl Pts',(1.54550256256333,2.82872027923607,17.0268227116797));
#15168=CARTESIAN_POINT('Ctrl Pts',(1.60152381998685,2.7973839728918,17.0227602685077));
#15169=CARTESIAN_POINT('Ctrl Pts',(1.90310394336902,2.61666167352433,17.0001901289475));
#15170=CARTESIAN_POINT('Ctrl Pts',(2.12873870261501,2.43662435203665,16.9805290442317));
#15171=CARTESIAN_POINT('Ctrl Pts',(2.38876069951904,2.16513093684089,16.9552634206903));
#15172=CARTESIAN_POINT('Ctrl Pts',(2.44739132564443,2.0986299279193,16.9493658372258));
#15173=CARTESIAN_POINT('Ctrl Pts',(2.53163781628203,1.99473425611013,16.9406733700638));
#15174=CARTESIAN_POINT('Ctrl Pts',(2.55932780593585,1.95908051387269,16.9377771682714));
#15175=CARTESIAN_POINT('Ctrl Pts',(2.59276825906274,1.91410272883475,16.9342415753543));
#15176=CARTESIAN_POINT('Ctrl Pts',(2.59923092654805,1.90531758514843,16.9335564597362));
#15177=CARTESIAN_POINT('Ctrl Pts',(2.60937871736071,1.89137527795711,16.9324779879709));
#15178=CARTESIAN_POINT('Ctrl Pts',(2.61309336649433,1.88623985545633,16.9320826291837));
#15179=CARTESIAN_POINT('Ctrl Pts',(2.62006678447413,1.87653911971586,16.9313393889866));
#15180=CARTESIAN_POINT('Ctrl Pts',(2.6233287445076,1.87197631439385,16.9309912945672));
#15181=CARTESIAN_POINT('Ctrl Pts',(2.63075943273545,1.86152475757216,16.9301973231937));
#15182=CARTESIAN_POINT('Ctrl Pts',(2.6349203050381,1.85563051399314,16.9297519881763));
#15183=CARTESIAN_POINT('Ctrl Pts',(2.64591648616228,1.83994189012584,16.9285729450347));
#15184=CARTESIAN_POINT('Ctrl Pts',(2.65271727762095,1.83012329258641,16.9278415351989));
#15185=CARTESIAN_POINT('Ctrl Pts',(2.70021824940439,1.76072297793753,16.9227155046396));
#15186=CARTESIAN_POINT('Ctrl Pts',(2.73896533401916,1.69982194942384,16.9184430712695));
#15187=CARTESIAN_POINT('Ctrl Pts',(2.80298315968369,1.59131980829472,16.9111233753168));
#15188=CARTESIAN_POINT('Ctrl Pts',(2.82916429582719,1.54429374231854,16.9080420985591));
#15189=CARTESIAN_POINT('Ctrl Pts',(2.98126386827609,1.2542318805005,16.8894538170206));
#15190=CARTESIAN_POINT('Ctrl Pts',(3.07697113863817,0.996636710725971,16.8745896734974));
#15191=CARTESIAN_POINT('Ctrl Pts',(3.15717528132441,0.651780297650595,16.8539645961918));
#15192=CARTESIAN_POINT('Ctrl Pts',(3.17244190741893,0.572873499747483,16.8492078053616));
#15193=CARTESIAN_POINT('Ctrl Pts',(3.18771176427329,0.474327952594113,16.8431855916211));
#15194=CARTESIAN_POINT('Ctrl Pts',(3.19050699188346,0.455146578607034,16.8420096573013));
#15195=CARTESIAN_POINT('Ctrl Pts',(3.19466292338349,0.424705737273957,16.840137071327));
#15196=CARTESIAN_POINT('Ctrl Pts',(3.19613755120719,0.413462097282861,16.8394440375476));
#15197=CARTESIAN_POINT('Ctrl Pts',(3.19879740286055,0.392316440802751,16.8381379880616));
#15198=CARTESIAN_POINT('Ctrl Pts',(3.1999960687612,0.382416226932203,16.8375254062753));
#15199=CARTESIAN_POINT('Ctrl Pts',(3.20258382452611,0.360178500039765,16.8361468942325));
#15200=CARTESIAN_POINT('Ctrl Pts',(3.20394760362646,0.347838254504404,16.8353801726675));
#15201=CARTESIAN_POINT('Ctrl Pts',(3.20723671537485,0.316414442758496,16.8334231636811));
#15202=CARTESIAN_POINT('Ctrl Pts',(3.20906302850927,0.297321209146729,16.8322297717533));
#15203=CARTESIAN_POINT('Ctrl Pts',(3.21879813030046,0.184973265233389,16.825181414043));
#15204=CARTESIAN_POINT('Ctrl Pts',(3.2228114076694,0.0914343725930345,16.8192049733415));
#15205=CARTESIAN_POINT('Ctrl Pts',(3.22260812845615,-0.214784973016233,
16.7992750104845));
#15206=CARTESIAN_POINT('Ctrl Pts',(3.20142070169844,-0.426873293043364,
16.7848545867541));
#15207=CARTESIAN_POINT('Ctrl Pts',(3.14466363018619,-0.709141254119123,
16.7653867776616));
#15208=CARTESIAN_POINT('Ctrl Pts',(3.12723119551926,-0.782442633742294,
16.7603109160857));
#15209=CARTESIAN_POINT('Ctrl Pts',(3.08246402247786,-0.945122803139734,
16.7490798027811));
#15210=CARTESIAN_POINT('Ctrl Pts',(3.05377633826291,-1.0340673037172,16.7429625965153));
#15211=CARTESIAN_POINT('Ctrl Pts',(3.01639764875923,-1.13475024536133,16.7361595076663));
#15212=CARTESIAN_POINT('Ctrl Pts',(3.01144810236233,-1.14782108284193,16.7352787420029));
#15213=CARTESIAN_POINT('Ctrl Pts',(3.00386100814568,-1.16747026642313,16.7339588078486));
#15214=CARTESIAN_POINT('Ctrl Pts',(3.00128661400922,-1.17407258808337,16.7335159991656));
#15215=CARTESIAN_POINT('Ctrl Pts',(2.99664480372383,-1.18586199078019,16.7327266270898));
#15216=CARTESIAN_POINT('Ctrl Pts',(2.994585671692,-1.19105222276095,16.7323795749864));
#15217=CARTESIAN_POINT('Ctrl Pts',(2.99010039539854,-1.20227261251952,16.7316303259829));
#15218=CARTESIAN_POINT('Ctrl Pts',(2.98766950228245,-1.20830077227111,16.731228420937));
#15219=CARTESIAN_POINT('Ctrl Pts',(2.98083399334295,-1.22510480547928,16.7301097230026));
#15220=CARTESIAN_POINT('Ctrl Pts',(2.97638915115945,-1.23586435775854,16.7293953219864));
#15221=CARTESIAN_POINT('Ctrl Pts',(2.95030605206727,-1.29804630177713,16.7252763266109));
#15222=CARTESIAN_POINT('Ctrl Pts',(2.92739229284414,-1.3489274397247,16.7219443973797));
#15223=CARTESIAN_POINT('Ctrl Pts',(2.79270535319926,-1.62838794226926,16.7037222334393));
#15224=CARTESIAN_POINT('Ctrl Pts',(2.65548091987462,-1.84371881742028,16.6899162435718));
#15225=CARTESIAN_POINT('Ctrl Pts',(2.39050750452443,-2.16759787712622,16.6662803365066));
#15226=CARTESIAN_POINT('Ctrl Pts',(2.27715285048547,-2.28638822658571,16.6568314493054));
#15227=CARTESIAN_POINT('Ctrl Pts',(2.13897211640319,-2.41068370876049,16.6456526892656));
#15228=CARTESIAN_POINT('Ctrl Pts',(2.12253309517528,-2.42517027897028,16.6443280685748));
#15229=CARTESIAN_POINT('Ctrl Pts',(2.09603375881475,-2.44804648361993,16.6422004807328));
#15230=CARTESIAN_POINT('Ctrl Pts',(2.08606761600122,-2.4565445238338,16.6414020175203));
#15231=CARTESIAN_POINT('Ctrl Pts',(2.06833821282144,-2.47147653402482,16.6399844326777));
#15232=CARTESIAN_POINT('Ctrl Pts',(2.0605959955818,-2.47793530185423,16.6393663407125));
#15233=CARTESIAN_POINT('Ctrl Pts',(2.04445811625709,-2.49127002506281,16.6380798855811));
#15234=CARTESIAN_POINT('Ctrl Pts',(2.03605778832255,-2.49814010914216,16.637411294562));
#15235=CARTESIAN_POINT('Ctrl Pts',(2.01427129230644,-2.51577498835048,16.6356798976594));
#15236=CARTESIAN_POINT('Ctrl Pts',(2.00083360134933,-2.52647531401277,16.6346145130469));
#15237=CARTESIAN_POINT('Ctrl Pts',(1.94313984177235,-2.57166743200128,16.6300505209162));
#15238=CARTESIAN_POINT('Ctrl Pts',(1.89807482783409,-2.6051059738277,16.6265105637313));
#15239=CARTESIAN_POINT('Ctrl Pts',(1.77691277894382,-2.69019585431608,16.6170515827017));
#15240=CARTESIAN_POINT('Ctrl Pts',(1.69944239467667,-2.73979301818201,16.6110608819657));
#15241=CARTESIAN_POINT('Ctrl Pts',(1.41044876229291,-2.90783245691427,16.5889456641452));
#15242=CARTESIAN_POINT('Ctrl Pts',(1.18788350038471,-3.00562359257762,16.5722773199921));
#15243=CARTESIAN_POINT('Ctrl Pts',(0.868239499374581,-3.10496619403906,
16.5500048248778));
#15244=CARTESIAN_POINT('Ctrl Pts',(0.778857058608428,-3.12858434900363,
16.5439556650797));
#15245=CARTESIAN_POINT('Ctrl Pts',(0.674953456053866,-3.15130922163454,
16.5372185813917));
#15246=CARTESIAN_POINT('Ctrl Pts',(0.661312650448159,-3.15419998939371,
16.5363399099712));
#15247=CARTESIAN_POINT('Ctrl Pts',(0.640718269620989,-3.15842488895197,
16.5350224931006));
#15248=CARTESIAN_POINT('Ctrl Pts',(0.633778565353956,-3.15982474396101,
16.5345801275577));
#15249=CARTESIAN_POINT('Ctrl Pts',(0.621357640402885,-3.16228768733928,
16.5337912339403));
#15250=CARTESIAN_POINT('Ctrl Pts',(0.615878236837986,-3.16335940635113,
16.5334442196338));
#15251=CARTESIAN_POINT('Ctrl Pts',(0.604008851983841,-3.16564893537518,
16.532694698199));
#15252=CARTESIAN_POINT('Ctrl Pts',(0.597617979686703,-3.16686163692679,
16.53229248483));
#15253=CARTESIAN_POINT('Ctrl Pts',(0.579756922009294,-3.17019487309247,
16.5311720574755));
#15254=CARTESIAN_POINT('Ctrl Pts',(0.568278693667798,-3.17227252265931,
16.5304562473701));
#15255=CARTESIAN_POINT('Ctrl Pts',(0.50146281119351,-3.18399243146146,16.5263126422797));
#15256=CARTESIAN_POINT('Ctrl Pts',(0.445888178102348,-3.19224957912384,
16.5229585314978));
#15257=CARTESIAN_POINT('Ctrl Pts',(0.137848799652848,-3.22981480221689,
16.5047352815579));
#15258=CARTESIAN_POINT('Ctrl Pts',(-0.117201385939855,-3.23063416120516,
16.4909440702368));
#15259=CARTESIAN_POINT('Ctrl Pts',(-0.532481629441486,-3.18267588268512,
16.467331056565));
#15260=CARTESIAN_POINT('Ctrl Pts',(-0.69355263211336,-3.1514975435824,16.4578895431112));
#15261=CARTESIAN_POINT('Ctrl Pts',(-0.872672789207635,-3.10242481668773,
16.4467190320074));
#15262=CARTESIAN_POINT('Ctrl Pts',(-0.893742568843931,-3.09642079255297,
16.4453945721666));
#15263=CARTESIAN_POINT('Ctrl Pts',(-0.927307059073515,-3.08648516951426,
16.4432671938948));
#15264=CARTESIAN_POINT('Ctrl Pts',(-0.939842088555001,-3.08269134427579,
16.4424687779838));
#15265=CARTESIAN_POINT('Ctrl Pts',(-0.961985670613258,-3.07584180150738,
16.4410512478789));
#15266=CARTESIAN_POINT('Ctrl Pts',(-0.971603716089313,-3.07281718193215,
16.4404331630847));
#15267=CARTESIAN_POINT('Ctrl Pts',(-0.991544377574944,-3.06644339286394,
16.4391466937124));
#15268=CARTESIAN_POINT('Ctrl Pts',(-1.00186457298129,-3.06308712039533,
16.4384780811364));
#15269=CARTESIAN_POINT('Ctrl Pts',(-1.0284773699044,-3.05428338306084,16.4367465656993));
#15270=CARTESIAN_POINT('Ctrl Pts',(-1.04474355742657,-3.04875770851709,
16.4356810834392));
#15271=CARTESIAN_POINT('Ctrl Pts',(-1.11395954859859,-3.02462585090819,
16.4311161063053));
#15272=CARTESIAN_POINT('Ctrl Pts',(-1.16645996777307,-3.00476919553406,
16.4275752395669));
#15273=CARTESIAN_POINT('Ctrl Pts',(-1.30357001872479,-2.94877668389805,
16.4181132109558));
#15274=CARTESIAN_POINT('Ctrl Pts',(-1.38719240977922,-2.91037341551829,
16.4121203147534));
#15275=CARTESIAN_POINT('Ctrl Pts',(-1.4711211693975,-2.86739001021449,16.4058821692644));
#15276=CARTESIAN_POINT('Ctrl Pts',(-1.47318889494024,-2.86632821653081,
16.4057283412007));
#15277=CARTESIAN_POINT('Ctrl Pts',(-1.47525540582449,-2.86526421994301,
16.4055744628637));
#15278=CARTESIAN_POINT('',(3.22275033525038,-0.00163969519989214,16.5668203720521));
#15279=CARTESIAN_POINT('Ctrl Pts',(-1.47525540483048,-2.8652642204548,16.1601692104994));
#15280=CARTESIAN_POINT('Ctrl Pts',(-1.43687104683692,-2.88502740012483,
16.1627794692134));
#15281=CARTESIAN_POINT('Ctrl Pts',(-1.3980901546135,-2.90401894906659,16.1653473167563));
#15282=CARTESIAN_POINT('Ctrl Pts',(-1.12873292759281,-3.02927932580612,
16.1827891100192));
#15283=CARTESIAN_POINT('Ctrl Pts',(-0.886665609477366,-3.10876543091489,
16.1965667153266));
#15284=CARTESIAN_POINT('Ctrl Pts',(-0.477124986012638,-3.19144535740846,
16.2201662265951));
#15285=CARTESIAN_POINT('Ctrl Pts',(-0.314274748655967,-3.21157168066685,
16.2296093263575));
#15286=CARTESIAN_POINT('Ctrl Pts',(-0.128733243122897,-3.22025233440821,
16.2407813169308));
#15287=CARTESIAN_POINT('Ctrl Pts',(-0.106843794828839,-3.221052888788,16.2421055119719));
#15288=CARTESIAN_POINT('Ctrl Pts',(-0.0718598700768303,-3.22197534867514,
16.2442324038511));
#15289=CARTESIAN_POINT('Ctrl Pts',(-0.058769620933428,-3.2222406974205,
16.2450305996282));
#15290=CARTESIAN_POINT('Ctrl Pts',(-0.0356002168597041,-3.22256912642433,
16.2464477012146));
#15291=CARTESIAN_POINT('Ctrl Pts',(-0.0255216432503605,-3.22266470363948,
16.247065578023));
#15292=CARTESIAN_POINT('Ctrl Pts',(-0.00459498457945542,-3.22276498182738,
16.2483515760995));
#15293=CARTESIAN_POINT('Ctrl Pts',(0.00625299345351246,-3.22276219064357,
16.2490199250224));
#15294=CARTESIAN_POINT('Ctrl Pts',(0.0342714343567632,-3.22261351632145,
16.2507506728098));
#15295=CARTESIAN_POINT('Ctrl Pts',(0.0514409461521228,-3.22238517521654,
16.2518156483829));
#15296=CARTESIAN_POINT('Ctrl Pts',(0.124678870817259,-3.22082569541067,
16.2563776303249));
#15297=CARTESIAN_POINT('Ctrl Pts',(0.180706401248717,-3.21816835169966,
16.2599159485872));
#15298=CARTESIAN_POINT('Ctrl Pts',(0.328288357972361,-3.20730268125544,
16.2693700232073));
#15299=CARTESIAN_POINT('Ctrl Pts',(0.419605168472895,-3.19663772081945,
16.2753573772499));
#15300=CARTESIAN_POINT('Ctrl Pts',(0.732533005896538,-3.14645113731676,
16.2963229025158));
#15301=CARTESIAN_POINT('Ctrl Pts',(0.950381880099279,-3.08763995407859,
16.3117528192285));
#15302=CARTESIAN_POINT('Ctrl Pts',(1.26200287906145,-2.96738100942387,16.3340991567899));
#15303=CARTESIAN_POINT('Ctrl Pts',(1.36165997201076,-2.92299310424172,16.3412789833713));
#15304=CARTESIAN_POINT('Ctrl Pts',(1.47188941530423,-2.86703188287969,16.3491137187671));
#15305=CARTESIAN_POINT('Ctrl Pts',(1.48484926595644,-2.86034140350533,16.3500330990949));
#15306=CARTESIAN_POINT('Ctrl Pts',(1.50406111575195,-2.85025758626339,16.3513928700871));
#15307=CARTESIAN_POINT('Ctrl Pts',(1.51034780889227,-2.84693126830408,16.3518373257058));
#15308=CARTESIAN_POINT('Ctrl Pts',(1.52131197242031,-2.8410835397242,16.3526115206454));
#15309=CARTESIAN_POINT('Ctrl Pts',(1.52599426051185,-2.83857135113489,16.3529418373027));
#15310=CARTESIAN_POINT('Ctrl Pts',(1.53068607837468,-2.83603908511265,16.3532725124688));
#15311=CARTESIAN_POINT('Ctrl Pts',(1.53070173753393,-2.83603063339014,16.353273616109));
#15312=CARTESIAN_POINT('Ctrl Pts',(1.5307329656665,-2.8360137782872,16.3532758170264));
#15313=CARTESIAN_POINT('Ctrl Pts',(1.53074853461697,-2.83600537492104,16.3532769143019));
#15314=CARTESIAN_POINT('Ctrl Pts',(1.53077958267836,-2.83598861634959,16.3532791025145));
#15315=CARTESIAN_POINT('Ctrl Pts',(1.53079506192688,-2.83598026107194,16.3532801934613));
#15316=CARTESIAN_POINT('Ctrl Pts',(1.53082593144913,-2.83596359821645,16.3532823690773));
#15317=CARTESIAN_POINT('Ctrl Pts',(1.53084132168351,-2.83595529066171,16.3532834537439));
#15318=CARTESIAN_POINT('Ctrl Pts',(1.53087201368719,-2.83593872298251,16.3532856168355));
#15319=CARTESIAN_POINT('Ctrl Pts',(1.53088731545902,-2.83593046285854,16.3532866952608));
#15320=CARTESIAN_POINT('Ctrl Pts',(1.53091783138174,-2.83591398959072,16.3532888459296));
#15321=CARTESIAN_POINT('Ctrl Pts',(1.53093304540083,-2.83590577651985,16.3532899181639));
#15322=CARTESIAN_POINT('Ctrl Pts',(1.53096338620605,-2.83588939715427,16.353292056478));
#15323=CARTESIAN_POINT('Ctrl Pts',(1.53097851303759,-2.83588123083685,16.3532931225611));
#15324=CARTESIAN_POINT('Ctrl Pts',(1.53100867997104,-2.83586494471184,16.3532952486084));
#15325=CARTESIAN_POINT('Ctrl Pts',(1.53102372018676,-2.83585682484459,16.3532963085808));
#15326=CARTESIAN_POINT('Ctrl Pts',(1.53105371439077,-2.83584063135414,16.3532984224422));
#15327=CARTESIAN_POINT('Ctrl Pts',(1.53106866848527,-2.83583255767536,16.3532994763388));
#15328=CARTESIAN_POINT('Ctrl Pts',(1.53109849149694,-2.83581645600016,16.3533015781228));
#15329=CARTESIAN_POINT('Ctrl Pts',(1.53111336021842,-2.83580842811114,16.3533026259965));
#15330=CARTESIAN_POINT('Ctrl Pts',(1.53114301285289,-2.83579241782153,16.3533047157608));
#15331=CARTESIAN_POINT('Ctrl Pts',(1.53115779674775,-2.83578443543244,16.3533057576501));
#15332=CARTESIAN_POINT('Ctrl Pts',(1.53118728021493,-2.83576851588544,16.3533078354801));
#15333=CARTESIAN_POINT('Ctrl Pts',(1.53120197983383,-2.83576057870407,16.3533088714241));
#15334=CARTESIAN_POINT('Ctrl Pts',(1.53123129531061,-2.83574474927439,16.353310937403));
#15335=CARTESIAN_POINT('Ctrl Pts',(1.53124591119265,-2.83573685701472,16.3533119674396));
#15336=CARTESIAN_POINT('Ctrl Pts',(1.53682950105994,-2.83272178368782,16.3537054630562));
#15337=CARTESIAN_POINT('Ctrl Pts',(1.54238966099265,-2.82969817372801,16.3540968724826));
#15338=CARTESIAN_POINT('Ctrl Pts',(1.55762976570956,-2.82135235315607,16.3551686091725));
#15339=CARTESIAN_POINT('Ctrl Pts',(1.56729141753032,-2.81599666343596,16.3558468319111));
#15340=CARTESIAN_POINT('Ctrl Pts',(1.58883856721532,-2.80390730354497,16.3573570883197));
#15341=CARTESIAN_POINT('Ctrl Pts',(1.60070924679475,-2.79714749009512,16.3581875384262));
#15342=CARTESIAN_POINT('Ctrl Pts',(1.63729797896763,-2.7760026604277,16.3607434618559));
#15343=CARTESIAN_POINT('Ctrl Pts',(1.66186846708456,-2.761363568712,16.3624545084569));
#15344=CARTESIAN_POINT('Ctrl Pts',(1.75651595199861,-2.70325163888702,16.3690377287852));
#15345=CARTESIAN_POINT('Ctrl Pts',(1.82511340845321,-2.65741993017932,16.3737924216299));
#15346=CARTESIAN_POINT('Ctrl Pts',(2.05998852297692,-2.48710364194464,16.3902861241016));
#15347=CARTESIAN_POINT('Ctrl Pts',(2.21592198644761,-2.34924063633112,16.4016626171965));
#15348=CARTESIAN_POINT('Ctrl Pts',(2.45530598079615,-2.09240603702729,16.4216072249065));
#15349=CARTESIAN_POINT('Ctrl Pts',(2.54597600075533,-1.98108280903499,16.4299252482917));
#15350=CARTESIAN_POINT('Ctrl Pts',(2.64131637295379,-1.84662511776808,16.4398433183095));
#15351=CARTESIAN_POINT('Ctrl Pts',(2.6535330550398,-1.82902673557182,16.4411388312144));
#15352=CARTESIAN_POINT('Ctrl Pts',(2.67285273508388,-1.80059533942263,16.4432283258975));
#15353=CARTESIAN_POINT('Ctrl Pts',(2.68006758409419,-1.78983883542452,16.4440180561888));
#15354=CARTESIAN_POINT('Ctrl Pts',(2.69276934051706,-1.77065298569718,16.4454253974699));
#15355=CARTESIAN_POINT('Ctrl Pts',(2.69828202754467,-1.76224084993321,16.4460420267629));
#15356=CARTESIAN_POINT('Ctrl Pts',(2.70969322140597,-1.7446487528916,16.4473307506324));
#15357=CARTESIAN_POINT('Ctrl Pts',(2.71558465479897,-1.73546437676793,16.4480030994042));
#15358=CARTESIAN_POINT('Ctrl Pts',(2.73078119955417,-1.71150706268432,16.4497558170423));
#15359=CARTESIAN_POINT('Ctrl Pts',(2.74001301052073,-1.6966882649136,16.4508388878112));
#15360=CARTESIAN_POINT('Ctrl Pts',(2.77979075792723,-1.63166611568644,16.4555871164191));
#15361=CARTESIAN_POINT('Ctrl Pts',(2.80907907613,-1.58071027775321,16.4592978957305));
#15362=CARTESIAN_POINT('Ctrl Pts',(2.88352119985531,-1.44258655895846,16.4693363625426));
#15363=CARTESIAN_POINT('Ctrl Pts',(2.92611063056265,-1.35411375008128,16.4757471439615));
#15364=CARTESIAN_POINT('Ctrl Pts',(3.06391328047553,-1.03087016547231,16.4990597496202));
#15365=CARTESIAN_POINT('Ctrl Pts',(3.13541675305209,-0.787024284961098,
16.5165261265935));
#15366=CARTESIAN_POINT('Ctrl Pts',(3.18445545964444,-0.497023538812584,
16.5359450691231));
#15367=CARTESIAN_POINT('Ctrl Pts',(3.19050456194766,-0.456585047758886,
16.5386209337383));
#15368=CARTESIAN_POINT('Ctrl Pts',(3.1960840269909,-0.413726841812239,16.5414159981397));
#15369=CARTESIAN_POINT('Ctrl Pts',(3.19638274399409,-0.411412641009479,
16.5415667964687));
#15370=CARTESIAN_POINT('Ctrl Pts',(3.20115105907343,-0.374153186569202,
16.5439926559566));
#15371=CARTESIAN_POINT('Ctrl Pts',(3.20505008346649,-0.339135540654309,
16.5462435908722));
#15372=CARTESIAN_POINT('Ctrl Pts',(3.20935959247385,-0.293662450607269,
16.5491230990537));
#15373=CARTESIAN_POINT('Ctrl Pts',(3.21029438425512,-0.283260661268862,
16.5497788305413));
#15374=CARTESIAN_POINT('Ctrl Pts',(3.21170639950285,-0.266642882345015,
16.5508215212418));
#15375=CARTESIAN_POINT('Ctrl Pts',(3.21221617008981,-0.260429839870924,
16.5512102692218));
#15376=CARTESIAN_POINT('Ctrl Pts',(3.21313455567376,-0.248823517618891,
16.5519343835033));
#15377=CARTESIAN_POINT('Ctrl Pts',(3.21354761655315,-0.24343075461257,16.5522699883894));
#15378=CARTESIAN_POINT('Ctrl Pts',(3.21435419241754,-0.232540457540709,
16.5529460392689));
#15379=CARTESIAN_POINT('Ctrl Pts',(3.21474717991929,-0.227042967240717,
16.5532864527513));
#15380=CARTESIAN_POINT('Ctrl Pts',(3.21562329551595,-0.214328488851954,
16.5540718183898));
#15381=CARTESIAN_POINT('Ctrl Pts',(3.21609623615602,-0.207110796221044,
16.5545162096624));
#15382=CARTESIAN_POINT('Ctrl Pts',(3.21725953382586,-0.188391644555414,
16.555665147561));
#15383=CARTESIAN_POINT('Ctrl Pts',(3.21791252461293,-0.176887853196649,
16.5563677062927));
#15384=CARTESIAN_POINT('Ctrl Pts',(3.22130600496964,-0.110846681959428,
16.560382052572));
#15385=CARTESIAN_POINT('Ctrl Pts',(3.2227218728278,-0.0562472651967042,
16.5636269405585));
#15386=CARTESIAN_POINT('Ctrl Pts',(3.22274958507906,-0.00163535095755876,
16.566821929544));
#15387=CARTESIAN_POINT('Ctrl Pts',(3.22274958283323,-0.00163977079054786,
16.5668216709681));
#15388=CARTESIAN_POINT('Ctrl Pts',(3.22288814644766,0.270688430919775,16.5827538418433));
#15389=CARTESIAN_POINT('Ctrl Pts',(3.18850939682181,0.541974969374395,16.5974513663888));
#15390=CARTESIAN_POINT('Ctrl Pts',(3.08809762302721,0.930840433051183,16.6202876628461));
#15391=CARTESIAN_POINT('Ctrl Pts',(3.04830463274175,1.05387104005822,16.6277746802112));
#15392=CARTESIAN_POINT('Ctrl Pts',(2.98997229446664,1.20297111761028,16.6373589726579));
#15393=CARTESIAN_POINT('Ctrl Pts',(2.97829202777991,1.23160477738666,16.6392233522321));
#15394=CARTESIAN_POINT('Ctrl Pts',(2.96086451649715,1.27262925477499,16.6419308410272));
#15395=CARTESIAN_POINT('Ctrl Pts',(2.95544749745275,1.28515912865734,16.6427627112954));
#15396=CARTESIAN_POINT('Ctrl Pts',(2.94587150754634,1.30692818317578,16.6442167661536));
#15397=CARTESIAN_POINT('Ctrl Pts',(2.94174823916291,1.31618293128753,16.6448377190982));
#15398=CARTESIAN_POINT('Ctrl Pts',(2.93370147243649,1.33401732961844,16.6460397857353));
#15399=CARTESIAN_POINT('Ctrl Pts',(2.92978380167953,1.34259950748036,16.6466206933161));
#15400=CARTESIAN_POINT('Ctrl Pts',(2.9203987414935,1.36292203759306,16.6480021741428));
#15401=CARTESIAN_POINT('Ctrl Pts',(2.91489818520797,1.37464680986191,16.6488038912345));
#15402=CARTESIAN_POINT('Ctrl Pts',(2.89518579790013,1.41601463294798,16.6516493938714));
#15403=CARTESIAN_POINT('Ctrl Pts',(2.88059162063208,1.44547225188051,16.6537064492311));
#15404=CARTESIAN_POINT('Ctrl Pts',(2.73215068373254,1.73391377962631,16.6741613660526));
#15405=CARTESIAN_POINT('Ctrl Pts',(2.5642196789729,1.97378066319265,16.693868316739));
#15406=CARTESIAN_POINT('Ctrl Pts',(2.32448742503514,2.2330893803528,16.7177379500803));
#15407=CARTESIAN_POINT('Ctrl Pts',(2.28127683380092,2.27721461059814,16.721898405702));
#15408=CARTESIAN_POINT('Ctrl Pts',(2.18591679230329,2.36915297582539,16.7307428112625));
#15409=CARTESIAN_POINT('Ctrl Pts',(2.13340425776605,2.41654829093347,16.7354128732634));
#15410=CARTESIAN_POINT('Ctrl Pts',(2.05965937535194,2.47882765166308,16.7416591764931));
#15411=CARTESIAN_POINT('Ctrl Pts',(2.03974730264462,2.4952383256033,16.7433161442429));
#15412=CARTESIAN_POINT('Ctrl Pts',(2.00975030533848,2.51936149037709,16.7457658830477));
#15413=CARTESIAN_POINT('Ctrl Pts',(1.99981391127771,2.52725601024126,16.7465698926828));
#15414=CARTESIAN_POINT('Ctrl Pts',(1.9817218795823,2.54145671300817,16.7480199704008));
#15415=CARTESIAN_POINT('Ctrl Pts',(1.97358217538157,2.54778280784465,16.7486673490659));
#15416=CARTESIAN_POINT('Ctrl Pts',(1.96048994660291,2.55785756180521,16.7497004143879));
#15417=CARTESIAN_POINT('Ctrl Pts',(1.95555677755493,2.56163108751508,16.7500878232504));
#15418=CARTESIAN_POINT('Ctrl Pts',(1.94635097190083,2.56863078685379,16.7508072795294));
#15419=CARTESIAN_POINT('Ctrl Pts',(1.94208125593679,2.57186053680696,16.7511395734207));
#15420=CARTESIAN_POINT('Ctrl Pts',(1.93205945300254,2.57940216122241,16.751916295475));
#15421=CARTESIAN_POINT('Ctrl Pts',(1.92630097741154,2.58370543716582,16.752360117959));
#15422=CARTESIAN_POINT('Ctrl Pts',(1.90850490193338,2.59691177487318,16.7537242583509));
#15423=CARTESIAN_POINT('Ctrl Pts',(1.89641941853812,2.60575039791774,16.7546401954249));
#15424=CARTESIAN_POINT('Ctrl Pts',(1.77361459680134,2.69425578553216,16.7638469879843));
#15425=CARTESIAN_POINT('Ctrl Pts',(1.65799018864464,2.7669118244583,16.7716981789034));
#15426=CARTESIAN_POINT('Ctrl Pts',(1.36500026586766,2.92603679283878,16.7905433398609));
#15427=CARTESIAN_POINT('Ctrl Pts',(1.18365312646038,3.00397801547755,16.8013658001541));
#15428=CARTESIAN_POINT('Ctrl Pts',(0.90892086360891,3.0932873767104,16.8178123676372));
#15429=CARTESIAN_POINT('Ctrl Pts',(0.820349363080166,3.11794626717646,16.8231171126153));
#15430=CARTESIAN_POINT('Ctrl Pts',(0.676226197475743,3.15150459447015,16.8318429968615));
#15431=CARTESIAN_POINT('Ctrl Pts',(0.621282522493068,3.16279473415359,16.835190668211));
#15432=CARTESIAN_POINT('Ctrl Pts',(0.549170454448684,3.17566122607053,16.8396233087036));
#15433=CARTESIAN_POINT('Ctrl Pts',(0.532242696753985,3.17854213513168,16.8406665952706));
#15434=CARTESIAN_POINT('Ctrl Pts',(0.504584497803225,3.1830221059754,16.8423760288762));
#15435=CARTESIAN_POINT('Ctrl Pts',(0.493867435710701,3.18470252832905,16.8430395790069));
#15436=CARTESIAN_POINT('Ctrl Pts',(0.4731770484024,3.18783980631016,16.8443229790252));
#15437=CARTESIAN_POINT('Ctrl Pts',(0.463204958640022,3.18930404828989,16.8449425859305));
#15438=CARTESIAN_POINT('Ctrl Pts',(0.44026346349064,3.19256277456438,16.8463705200317));
#15439=CARTESIAN_POINT('Ctrl Pts',(0.427289729461621,3.19432504072199,16.8471798595339));
#15440=CARTESIAN_POINT('Ctrl Pts',(0.392583777819613,3.1988240517302,16.8493499490017));
#15441=CARTESIAN_POINT('Ctrl Pts',(0.37083409056914,3.20141833810365,16.8507151781246));
#15442=CARTESIAN_POINT('Ctrl Pts',(0.186146766808726,3.22154043016926,16.8623545427983));
#15443=CARTESIAN_POINT('Ctrl Pts',(0.0221427005186359,3.22683565931571,
16.8730160139398));
#15444=CARTESIAN_POINT('Ctrl Pts',(-0.395194689870823,3.20848997520268,
16.900877948811));
#15445=CARTESIAN_POINT('Ctrl Pts',(-0.646637665879886,3.1674029857535,16.9184041684116));
#15446=CARTESIAN_POINT('Ctrl Pts',(-0.944851169216543,3.08164806758982,
16.9387047186415));
#15447=CARTESIAN_POINT('Ctrl Pts',(-0.998640302895386,3.06463978474988,
16.9423419768065));
#15448=CARTESIAN_POINT('Ctrl Pts',(-1.06299494740521,3.04241608297576,16.9466414272059));
#15449=CARTESIAN_POINT('Ctrl Pts',(-1.0740103568379,3.03854498788661,16.947375476424));
#15450=CARTESIAN_POINT('Ctrl Pts',(-1.09113074361928,3.03242371528115,16.9485131551884));
#15451=CARTESIAN_POINT('Ctrl Pts',(-1.09725022277467,3.03021481731377,16.9489191664214));
#15452=CARTESIAN_POINT('Ctrl Pts',(-1.10860669212745,3.02607665327396,16.949671394407));
#15453=CARTESIAN_POINT('Ctrl Pts',(-1.11384530965598,3.02415233349664,16.9500178895709));
#15454=CARTESIAN_POINT('Ctrl Pts',(-1.12571114265484,3.01975859987549,16.9508016145926));
#15455=CARTESIAN_POINT('Ctrl Pts',(-1.13233522857189,3.01728097972435,16.951238347267));
#15456=CARTESIAN_POINT('Ctrl Pts',(-1.1519693805056,3.00986341392209,16.9525306778812));
#15457=CARTESIAN_POINT('Ctrl Pts',(-1.16495586179563,3.00486090865413,16.953382622098));
#15458=CARTESIAN_POINT('Ctrl Pts',(-1.26320784837846,2.96628068057538,16.9598095905856));
#15459=CARTESIAN_POINT('Ctrl Pts',(-1.3470473050248,2.92916064175367,16.9651875753164));
#15460=CARTESIAN_POINT('Ctrl Pts',(-1.64723960812469,2.78062947794585,16.9844470886907));
#15461=CARTESIAN_POINT('Ctrl Pts',(-1.85237187114893,2.64840146045662,16.9976708473158));
#15462=CARTESIAN_POINT('Ctrl Pts',(-2.11178439176846,2.43616995736128,17.0167527005432));
#15463=CARTESIAN_POINT('Ctrl Pts',(-2.1803640826349,2.374987982864,17.0220554742781));
#15464=CARTESIAN_POINT('Ctrl Pts',(-2.28643953713941,2.27188370668758,17.0307784119491));
#15465=CARTESIAN_POINT('Ctrl Pts',(-2.32561692550568,2.23176313124768,17.0341251729222));
#15466=CARTESIAN_POINT('Ctrl Pts',(-2.37539700916889,2.17804990780606,17.0385567756291));
#15467=CARTESIAN_POINT('Ctrl Pts',(-2.38696681836457,2.16536411310951,17.0395999595713));
#15468=CARTESIAN_POINT('Ctrl Pts',(-2.40568006991776,2.14451361282182,17.0413092672694));
#15469=CARTESIAN_POINT('Ctrl Pts',(-2.41288472566808,2.13640411216259,17.0419727948554));
#15470=CARTESIAN_POINT('Ctrl Pts',(-2.42670438707492,2.1206897392875,17.0432561809479));
#15471=CARTESIAN_POINT('Ctrl Pts',(-2.43332493653283,2.11308989447489,17.0438757966316));
#15472=CARTESIAN_POINT('Ctrl Pts',(-2.44846397978494,2.09554602650425,17.0453037935163));
#15473=CARTESIAN_POINT('Ctrl Pts',(-2.45695769577548,2.08558094605268,17.0461131873146));
#15474=CARTESIAN_POINT('Ctrl Pts',(-2.47949904464798,2.05880595350854,17.048283517061));
#15475=CARTESIAN_POINT('Ctrl Pts',(-2.49343620801465,2.04190433294468,17.0496489337253));
#15476=CARTESIAN_POINT('Ctrl Pts',(-2.61025784551694,1.8972549018431,17.0612978414188));
#15477=CARTESIAN_POINT('Ctrl Pts',(-2.70340745699684,1.76198625855598,17.0719694029455));
#15478=CARTESIAN_POINT('Ctrl Pts',(-2.91365709843681,1.40048093370004,17.0998630840193));
#15479=CARTESIAN_POINT('Ctrl Pts',(-3.01500893817588,1.16638797056696,17.1174116234875));
#15480=CARTESIAN_POINT('Ctrl Pts',(-3.10383096287479,0.869186312944634,
17.1377003658454));
#15481=CARTESIAN_POINT('Ctrl Pts',(-3.1184619663617,0.815136404891894,17.141309971854));
#15482=CARTESIAN_POINT('Ctrl Pts',(-3.13442829984756,0.749408114249852,
17.1455812296786));
#15483=CARTESIAN_POINT('Ctrl Pts',(-3.13711695707819,0.738072148225407,
17.1463136656712));
#15484=CARTESIAN_POINT('Ctrl Pts',(-3.1412099373363,0.720388746664569,17.1474493933438));
#15485=CARTESIAN_POINT('Ctrl Pts',(-3.14265659555009,0.714051357367769,
17.1478550537932));
#15486=CARTESIAN_POINT('Ctrl Pts',(-3.14530977503582,0.702264291362181,
17.1486069651574));
#15487=CARTESIAN_POINT('Ctrl Pts',(-3.14652130193718,0.696815910425137,
17.1489534923926));
#15488=CARTESIAN_POINT('Ctrl Pts',(-3.14923749481479,0.684449331192447,
17.1497377144771));
#15489=CARTESIAN_POINT('Ctrl Pts',(-3.15073351874669,0.677529321743561,
17.1501749095033));
#15490=CARTESIAN_POINT('Ctrl Pts',(-3.15510991149637,0.656957885669661,
17.1514698783234));
#15491=CARTESIAN_POINT('Ctrl Pts',(-3.15792449265331,0.64329241577073,17.1523239762318));
#15492=CARTESIAN_POINT('Ctrl Pts',(-3.1787718334036,0.538638299834818,17.1588209881452));
#15493=CARTESIAN_POINT('Ctrl Pts',(-3.19295929309754,0.446918352276326,
17.1642619658142));
#15494=CARTESIAN_POINT('Ctrl Pts',(-3.22979287532408,0.114292330514911,
17.1834956713751));
#15495=CARTESIAN_POINT('Ctrl Pts',(-3.22926632173964,-0.128360909863536,
17.1966482671688));
#15496=CARTESIAN_POINT('Ctrl Pts',(-3.19106676167714,-0.460081781200723,
17.2156575103638));
#15497=CARTESIAN_POINT('Ctrl Pts',(-3.17663311220484,-0.550983175277661,
17.2209677836826));
#15498=CARTESIAN_POINT('Ctrl Pts',(-3.14716550179649,-0.696144582347413,
17.2297019309418));
#15499=CARTESIAN_POINT('Ctrl Pts',(-3.13456466839963,-0.750847346388877,
17.2330521546242));
#15500=CARTESIAN_POINT('Ctrl Pts',(-3.11625113098277,-0.82182203919301,
17.2374877045553));
#15501=CARTESIAN_POINT('Ctrl Pts',(-3.11182697131488,-0.838418426733112,
17.2385312787006));
#15502=CARTESIAN_POINT('Ctrl Pts',(-3.10439221451665,-0.865438758033863,
17.2402410651317));
#15503=CARTESIAN_POINT('Ctrl Pts',(-3.10146123211895,-0.875884402515627,
17.2409046784409));
#15504=CARTESIAN_POINT('Ctrl Pts',(-3.09570577093514,-0.896004978763492,
17.2421881175188));
#15505=CARTESIAN_POINT('Ctrl Pts',(-3.09288853656246,-0.905681864060256,
17.2428076998579));
#15506=CARTESIAN_POINT('Ctrl Pts',(-3.08630794113903,-0.92789666222965,
17.2442354581794));
#15507=CARTESIAN_POINT('Ctrl Pts',(-3.08251350669414,-0.940425114634566,
17.2450446456535));
#15508=CARTESIAN_POINT('Ctrl Pts',(-3.07216866666618,-0.973846320525354,
17.2472140623935));
#15509=CARTESIAN_POINT('Ctrl Pts',(-3.06548158241934,-0.994695733416725,
17.2485787664536));
#15510=CARTESIAN_POINT('Ctrl Pts',(-3.00707655740649,-1.17061006154054,
17.2601914949498));
#15511=CARTESIAN_POINT('Ctrl Pts',(-2.94385058567796,-1.32157727095709,
17.2708248078673));
#15512=CARTESIAN_POINT('Ctrl Pts',(-2.75425263541487,-1.69241150957489,
17.2986003649391));
#15513=CARTESIAN_POINT('Ctrl Pts',(-2.61291315845547,-1.90337702111653,
17.3160666772289));
#15514=CARTESIAN_POINT('Ctrl Pts',(-2.41093811945269,-2.13934707375403,
17.3364001332943));
#15515=CARTESIAN_POINT('Ctrl Pts',(-2.37235455828529,-2.18205484363251,
17.3401127728689));
#15516=CARTESIAN_POINT('Ctrl Pts',(-2.32454225219463,-2.23220939639732,
17.3444889650181));
#15517=CARTESIAN_POINT('Ctrl Pts',(-2.31639266660409,-2.24066519045606,
17.3452273370719));
#15518=CARTESIAN_POINT('Ctrl Pts',(-2.30364629185895,-2.25374662362072,
17.3463702426869));
#15519=CARTESIAN_POINT('Ctrl Pts',(-2.29908147682017,-2.25840307434431,
17.3467771926954));
#15520=CARTESIAN_POINT('Ctrl Pts',(-2.29058457586657,-2.26701808406307,
17.3475302726539));
#15521=CARTESIAN_POINT('Ctrl Pts',(-2.28665637943411,-2.27098024998006,
17.3478766865998));
#15522=CARTESIAN_POINT('Ctrl Pts',(-2.2777397420623,-2.27992740285685,17.348659102346));
#15523=CARTESIAN_POINT('Ctrl Pts',(-2.27274522903054,-2.28490621711702,
17.3490946139394));
#15524=CARTESIAN_POINT('Ctrl Pts',(-2.25791314556384,-2.29959493091296,
17.3503799892889));
#15525=CARTESIAN_POINT('Ctrl Pts',(-2.24802925731558,-2.30925812617988,
17.3512262574319));
#15526=CARTESIAN_POINT('Ctrl Pts',(-2.17404983510609,-2.38066057328217,
17.3574872343597));
#15527=CARTESIAN_POINT('Ctrl Pts',(-2.10747740693861,-2.43979088021718,
17.3627162187903));
#15528=CARTESIAN_POINT('Ctrl Pts',(-1.8641464998645,-2.63851686807412,17.3808054355103));
#15529=CARTESIAN_POINT('Ctrl Pts',(-1.67535224198654,-2.76223918761152,
17.3930890918511));
#15530=CARTESIAN_POINT('Ctrl Pts',(-1.47525540448705,-2.86526422063162,
17.4058265726261));
#15531=CARTESIAN_POINT('Origin',(0.,0.,4.68922655072688));
#15532=CARTESIAN_POINT('',(-1.47525548819425,-2.8652641775328,18.9012640026169));
#15533=CARTESIAN_POINT('',(-1.47525539597219,-2.86526422501572,18.654425498672));
#15534=CARTESIAN_POINT('',(-1.47525540501186,-2.86526422036142,4.68922655072688));
#15535=CARTESIAN_POINT('',(3.22274859936717,0.00236444057009463,18.0625860991293));
#15536=CARTESIAN_POINT('Ctrl Pts',(-1.4752554881943,-2.86526417753278,18.9012640026169));
#15537=CARTESIAN_POINT('Ctrl Pts',(-1.67171863009127,-2.76411003943129,
18.8885120716065));
#15538=CARTESIAN_POINT('Ctrl Pts',(-1.85735696437909,-2.64296677365553,
18.8764349148439));
#15539=CARTESIAN_POINT('Ctrl Pts',(-2.15721040708762,-2.39993951516703,
18.8546383190739));
#15540=CARTESIAN_POINT('Ctrl Pts',(-2.27705492008618,-2.28654252812363,
18.8451462635796));
#15541=CARTESIAN_POINT('Ctrl Pts',(-2.4024236645032,-2.14824553622978,18.8339192001379));
#15542=CARTESIAN_POINT('Ctrl Pts',(-2.41698387361396,-2.13185066690676,
18.8325936419603));
#15543=CARTESIAN_POINT('Ctrl Pts',(-2.43997509192983,-2.10542413185119,
18.83046483271));
#15544=CARTESIAN_POINT('Ctrl Pts',(-2.44851434335956,-2.09548722893398,
18.8296660938478));
#15545=CARTESIAN_POINT('Ctrl Pts',(-2.46351774606513,-2.07781124026806,
18.8282481899785));
#15546=CARTESIAN_POINT('Ctrl Pts',(-2.4700066516743,-2.07009332455724,18.8276300561806));
#15547=CARTESIAN_POINT('Ctrl Pts',(-2.48340240946966,-2.0540077303389,18.8263436838233));
#15548=CARTESIAN_POINT('Ctrl Pts',(-2.49030342901978,-2.04563538062245,
18.8256752182548));
#15549=CARTESIAN_POINT('Ctrl Pts',(-2.50801486865001,-2.02392532935546,
18.823944511199));
#15550=CARTESIAN_POINT('Ctrl Pts',(-2.51876111458003,-2.01053593588118,
18.8228796948802));
#15551=CARTESIAN_POINT('Ctrl Pts',(-2.56411835111969,-1.95308824128143,
18.818321431071));
#15552=CARTESIAN_POINT('Ctrl Pts',(-2.59768250219901,-1.90821947866712,
18.814786762879));
#15553=CARTESIAN_POINT('Ctrl Pts',(-2.68309084624673,-1.78761339058424,
18.8053454961269));
#15554=CARTESIAN_POINT('Ctrl Pts',(-2.73289610856644,-1.71050123479499,
18.7993675540166));
#15555=CARTESIAN_POINT('Ctrl Pts',(-2.90296300293422,-1.4207617055756,18.77714407621));
#15556=CARTESIAN_POINT('Ctrl Pts',(-3.00223360097899,-1.19680250230503,
18.7603429412645));
#15557=CARTESIAN_POINT('Ctrl Pts',(-3.10244883864784,-0.877037562064718,
18.7380575437401));
#15558=CARTESIAN_POINT('Ctrl Pts',(-3.12595815834096,-0.78915941668079,
18.7321085138865));
#15559=CARTESIAN_POINT('Ctrl Pts',(-3.14874069313296,-0.686835231848619,
18.7254687335981));
#15560=CARTESIAN_POINT('Ctrl Pts',(-3.15167246180206,-0.673254259683618,
18.7245932471418));
#15561=CARTESIAN_POINT('Ctrl Pts',(-3.15596324926836,-0.652735397201517,
18.7232796596718));
#15562=CARTESIAN_POINT('Ctrl Pts',(-3.15738737410719,-0.645811506233739,
18.7228379690362));
#15563=CARTESIAN_POINT('Ctrl Pts',(-3.15989538676375,-0.633411296429543,
18.7220498029931));
#15564=CARTESIAN_POINT('Ctrl Pts',(-3.16098783340588,-0.627936815578269,
18.7217028451295));
#15565=CARTESIAN_POINT('Ctrl Pts',(-3.16332395852555,-0.616069403648415,
18.7209529036556));
#15566=CARTESIAN_POINT('Ctrl Pts',(-3.16456248151383,-0.609675552290934,
18.7205502167251));
#15567=CARTESIAN_POINT('Ctrl Pts',(-3.16797182510812,-0.591784565590774,
18.7194271315627));
#15568=CARTESIAN_POINT('Ctrl Pts',(-3.17009945632821,-0.580279159992346,
18.718709155718));
#15569=CARTESIAN_POINT('Ctrl Pts',(-3.18218236287185,-0.512889018677115,
18.7145273501294));
#15570=CARTESIAN_POINT('Ctrl Pts',(-3.19072308545401,-0.456756874700976,
18.7111388013356));
#15571=CARTESIAN_POINT('Ctrl Pts',(-3.22929970137806,-0.148685318902755,
18.6929135928336));
#15572=CARTESIAN_POINT('Ctrl Pts',(-3.23098934338144,0.105918464265947,
18.6791451247785));
#15573=CARTESIAN_POINT('Ctrl Pts',(-3.18460986234148,0.520723345587924,
18.6555675995775));
#15574=CARTESIAN_POINT('Ctrl Pts',(-3.15407168514966,0.681699475468597,
18.6461377178382));
#15575=CARTESIAN_POINT('Ctrl Pts',(-3.10574092968199,0.860796509723744,
18.6349802178779));
#15576=CARTESIAN_POINT('Ctrl Pts',(-3.09981872906552,0.881885006168486,
18.6336560122168));
#15577=CARTESIAN_POINT('Ctrl Pts',(-3.09001322816324,0.915482004540831,
18.631528965117));
#15578=CARTESIAN_POINT('Ctrl Pts',(-3.08626778594734,0.928030277707106,
18.630730623957));
#15579=CARTESIAN_POINT('Ctrl Pts',(-3.07950351887017,0.950198553830946,
18.6293131803501));
#15580=CARTESIAN_POINT('Ctrl Pts',(-3.0765158153351,0.959827926640993,18.6286951068839));
#15581=CARTESIAN_POINT('Ctrl Pts',(-3.07021834120105,0.979793184016866,
18.6274086149846));
#15582=CARTESIAN_POINT('Ctrl Pts',(-3.06690145145268,0.990126672985495,
18.6267399683244));
#15583=CARTESIAN_POINT('Ctrl Pts',(-3.05819876055078,1.01677584053529,18.625008265472));
#15584=CARTESIAN_POINT('Ctrl Pts',(-3.05273461702311,1.03306539412136,18.6239426288216));
#15585=CARTESIAN_POINT('Ctrl Pts',(-3.02885975066243,1.10239672428763,18.6193760938647));
#15586=CARTESIAN_POINT('Ctrl Pts',(-3.00919578062714,1.15499352420319,18.6158337885739));
#15587=CARTESIAN_POINT('Ctrl Pts',(-2.95369796359921,1.29238404052255,18.6063669391563));
#15588=CARTESIAN_POINT('Ctrl Pts',(-2.91559000495747,1.37619786431467,18.6003705697869));
#15589=CARTESIAN_POINT('Ctrl Pts',(-2.76469229400977,1.67358824095776,18.5783083036408));
#15590=CARTESIAN_POINT('Ctrl Pts',(-2.63159300282053,1.87593298399687,18.5617041796305));
#15591=CARTESIAN_POINT('Ctrl Pts',(-2.4175863798237,2.13308837216077,18.5394371195426));
#15592=CARTESIAN_POINT('Ctrl Pts',(-2.35493550960416,2.20206089283585,18.5333386739722));
#15593=CARTESIAN_POINT('Ctrl Pts',(-2.27954852365089,2.27815082307226,18.5265537733142));
#15594=CARTESIAN_POINT('Ctrl Pts',(-2.26965357179802,2.28800903079234,18.525673579389));
#15595=CARTESIAN_POINT('Ctrl Pts',(-2.2546434462941,2.30277021916648,18.5243543324097));
#15596=CARTESIAN_POINT('Ctrl Pts',(-2.24957583622986,2.30772102116472,18.5239116446557));
#15597=CARTESIAN_POINT('Ctrl Pts',(-2.2404850698265,2.31654384613753,18.5231224032046));
#15598=CARTESIAN_POINT('Ctrl Pts',(-2.23646815166869,2.32042214852105,18.5227753614731));
#15599=CARTESIAN_POINT('Ctrl Pts',(-2.22775236774547,2.32879351066753,18.5220260383882));
#15600=CARTESIAN_POINT('Ctrl Pts',(-2.22304999412004,2.33328278456114,18.5216240494078));
#15601=CARTESIAN_POINT('Ctrl Pts',(-2.20988498633244,2.34577526093082,18.5205048807529));
#15602=CARTESIAN_POINT('Ctrl Pts',(-2.20139240091943,2.35374695633205,18.5197900962164));
#15603=CARTESIAN_POINT('Ctrl Pts',(-2.15189762402353,2.39970377141098,18.5156644215757));
#15604=CARTESIAN_POINT('Ctrl Pts',(-2.10995326087426,2.43666569058571,18.5123264724417));
#15605=CARTESIAN_POINT('Ctrl Pts',(-1.87192689628223,2.63565946837268,18.494104027447));
#15606=CARTESIAN_POINT('Ctrl Pts',(-1.65814347509957,2.77513942162934,18.4803020584553));
#15607=CARTESIAN_POINT('Ctrl Pts',(-1.28324315551436,2.96079095849586,18.4566721327093));
#15608=CARTESIAN_POINT('Ctrl Pts',(-1.13100556626155,3.02221972243942,18.4472249929358));
#15609=CARTESIAN_POINT('Ctrl Pts',(-0.953886489040685,3.07842461201488,
18.4360483281191));
#15610=CARTESIAN_POINT('Ctrl Pts',(-0.932937966991596,3.08483779788748,
18.4347238878604));
#15611=CARTESIAN_POINT('Ctrl Pts',(-0.899364822254162,3.0947426383176,18.432596535102));
#15612=CARTESIAN_POINT('Ctrl Pts',(-0.886781245041957,3.09837184605472,
18.4317981249496));
#15613=CARTESIAN_POINT('Ctrl Pts',(-0.86447160800387,3.10465908869522,18.4303806015085));
#15614=CARTESIAN_POINT('Ctrl Pts',(-0.854754483739298,3.10734838518644,
18.4297625175872));
#15615=CARTESIAN_POINT('Ctrl Pts',(-0.834552373647748,3.11283755934735,
18.4284760464805));
#15616=CARTESIAN_POINT('Ctrl Pts',(-0.824065558495295,3.1156301587213,18.4278074312794));
#15617=CARTESIAN_POINT('Ctrl Pts',(-0.796942050168053,3.12270652793809,
18.4260759014084));
#15618=CARTESIAN_POINT('Ctrl Pts',(-0.780285015068942,3.12691029097273,
18.4250104072577));
#15619=CARTESIAN_POINT('Ctrl Pts',(-0.709068355799243,3.14427887983443,
18.4204453101652));
#15620=CARTESIAN_POINT('Ctrl Pts',(-0.654206193393191,3.15614974688904,
18.4169043326551));
#15621=CARTESIAN_POINT('Ctrl Pts',(-0.508679431302738,3.18368099662322,
18.4074419328634));
#15622=CARTESIAN_POINT('Ctrl Pts',(-0.417610959557511,3.19690131416866,
18.4014487692547));
#15623=CARTESIAN_POINT('Ctrl Pts',(-0.0853757478731432,3.23069345661436,
18.3793561770081));
#15624=CARTESIAN_POINT('Ctrl Pts',(0.157323036334906,3.22798758196651,18.3627153256153));
#15625=CARTESIAN_POINT('Ctrl Pts',(0.489420883052464,3.18671925295795,18.3404452152041));
#15626=CARTESIAN_POINT('Ctrl Pts',(0.580895232767638,3.17132095643393,18.3343750193888));
#15627=CARTESIAN_POINT('Ctrl Pts',(0.685233822317667,3.14908984830965,18.3276175203486));
#15628=CARTESIAN_POINT('Ctrl Pts',(0.69886229639906,3.14609341425497,18.3267381954584));
#15629=CARTESIAN_POINT('Ctrl Pts',(0.719377511074815,3.14144293401129,18.3254199930564));
#15630=CARTESIAN_POINT('Ctrl Pts',(0.726278756195095,3.13985459562453,18.3249774891853));
#15631=CARTESIAN_POINT('Ctrl Pts',(0.738611764379593,3.13697328617736,18.3241884462775));
#15632=CARTESIAN_POINT('Ctrl Pts',(0.744045436093191,3.13568893981498,18.3238414202348));
#15633=CARTESIAN_POINT('Ctrl Pts',(0.755800816501357,3.13287806664361,18.3230919841252));
#15634=CARTESIAN_POINT('Ctrl Pts',(0.762121231774153,3.13134652897522,18.3226898672218));
#15635=CARTESIAN_POINT('Ctrl Pts',(0.779757984915972,3.12701629949713,18.3215699810386));
#15636=CARTESIAN_POINT('Ctrl Pts',(0.791063973366917,3.12417529150988,18.3208546118785));
#15637=CARTESIAN_POINT('Ctrl Pts',(0.856640836781233,3.10731810145019,18.3167187284499));
#15638=CARTESIAN_POINT('Ctrl Pts',(0.910557739454847,3.09194838133759,18.313371577826));
#15639=CARTESIAN_POINT('Ctrl Pts',(1.2066399540449,2.99912840565029,18.2951486835302));
#15640=CARTESIAN_POINT('Ctrl Pts',(1.43940148490777,2.89463329359777,18.2813528459546));
#15641=CARTESIAN_POINT('Ctrl Pts',(1.79797315437103,2.67959842873945,18.2577363040664));
#15642=CARTESIAN_POINT('Ctrl Pts',(1.93182129658792,2.58476522123123,18.248296275197));
#15643=CARTESIAN_POINT('Ctrl Pts',(2.07476017224962,2.46616491235887,18.2371252383939));
#15644=CARTESIAN_POINT('Ctrl Pts',(2.09150483055766,2.45198014971012,18.2357985935032));
#15645=CARTESIAN_POINT('Ctrl Pts',(2.11801710570682,2.42905185277313,18.2336683684992));
#15646=CARTESIAN_POINT('Ctrl Pts',(2.1278786896597,2.42041765768914,18.2328693101938));
#15647=CARTESIAN_POINT('Ctrl Pts',(2.14523360841067,2.40503472273328,18.2314510365198));
#15648=CARTESIAN_POINT('Ctrl Pts',(2.1527484958853,2.39831048073426,18.2308328541509));
#15649=CARTESIAN_POINT('Ctrl Pts',(2.16715096315845,2.38530107236995,18.2296401953241));
#15650=CARTESIAN_POINT('Ctrl Pts',(2.17404307714045,2.37902105891924,18.2290659409453));
#15651=CARTESIAN_POINT('Ctrl Pts',(2.19203346855889,2.3624849615626,18.2275576411727));
#15652=CARTESIAN_POINT('Ctrl Pts',(2.2030869330567,2.35218066350339,18.2266215368172));
#15653=CARTESIAN_POINT('Ctrl Pts',(2.24425796657028,2.31325527488551,18.2230990424902));
#15654=CARTESIAN_POINT('Ctrl Pts',(2.27389255058914,2.28413138744896,18.2204909112857));
#15655=CARTESIAN_POINT('Ctrl Pts',(2.3460843729106,2.21038614700822,18.2139505196783));
#15656=CARTESIAN_POINT('Ctrl Pts',(2.38793831318083,2.1651024463524,18.2099895603055));
#15657=CARTESIAN_POINT('Ctrl Pts',(2.5083266400144,2.02710933064286,18.1980787943525));
#15658=CARTESIAN_POINT('Ctrl Pts',(2.58294102879452,1.93113585737514,18.1899939342971));
#15659=CARTESIAN_POINT('Ctrl Pts',(2.7944592501101,1.62481187872696,18.1649296645631));
#15660=CARTESIAN_POINT('Ctrl Pts',(2.91239209062325,1.40249866989612,18.1476699394747));
#15661=CARTESIAN_POINT('Ctrl Pts',(3.01105641066714,1.14895945769275,18.1303019676058));
#15662=CARTESIAN_POINT('Ctrl Pts',(3.0185623306977,1.12909258064088,18.1289561275231));
#15663=CARTESIAN_POINT('Ctrl Pts',(3.02880797202738,1.10114151098179,18.1270851492334));
#15664=CARTESIAN_POINT('Ctrl Pts',(3.03171261142713,1.09311893418051,18.1265507193513));
#15665=CARTESIAN_POINT('Ctrl Pts',(3.03634854228329,1.0801539309388,18.1256913169539));
#15666=CARTESIAN_POINT('Ctrl Pts',(3.03809968381862,1.07521872047775,18.1253651754808));
#15667=CARTESIAN_POINT('Ctrl Pts',(3.04175618536977,1.06483341627488,18.1246809910771));
#15668=CARTESIAN_POINT('Ctrl Pts',(3.0436589396225,1.05938244069887,18.1243231105734));
#15669=CARTESIAN_POINT('Ctrl Pts',(3.04826915198432,1.04606023969208,18.1234513841908));
#15670=CARTESIAN_POINT('Ctrl Pts',(3.0509608069407,1.03818351274536,18.122938472925));
#15671=CARTESIAN_POINT('Ctrl Pts',(3.0604955236225,1.00992424507303,18.121106936953));
#15672=CARTESIAN_POINT('Ctrl Pts',(3.06716527260713,0.989483238282234,18.1197981678248));
#15673=CARTESIAN_POINT('Ctrl Pts',(3.10715374040053,0.862638288651236,18.111766819375));
#15674=CARTESIAN_POINT('Ctrl Pts',(3.13513996336408,0.754620344036068,18.1053169123422));
#15675=CARTESIAN_POINT('Ctrl Pts',(3.20072247970803,0.433752192019144,18.0867149640922));
#15676=CARTESIAN_POINT('Ctrl Pts',(3.2225904146029,0.218342495289665,18.0748961830584));
#15677=CARTESIAN_POINT('Ctrl Pts',(3.22274912977859,0.00236833514711092,
18.0625872459229));
#15678=CARTESIAN_POINT('Ctrl Pts',(3.22274913267655,0.00236438840992122,
18.0625870209879));
#15679=CARTESIAN_POINT('Ctrl Pts',(3.22284445157515,-0.127558807163035,
18.0551823522885));
#15680=CARTESIAN_POINT('Ctrl Pts',(3.21508323492089,-0.257358662884279,
18.0476275395715));
#15681=CARTESIAN_POINT('Ctrl Pts',(3.19737230323124,-0.404037165608398,
18.0387486267077));
#15682=CARTESIAN_POINT('Ctrl Pts',(3.19508730105094,-0.421725972463517,
18.0376722990145));
#15683=CARTESIAN_POINT('Ctrl Pts',(3.1910443671095,-0.451102061197792,18.0358751522722));
#15684=CARTESIAN_POINT('Ctrl Pts',(3.1893687454429,-0.46280041300465,18.0351569235573));
#15685=CARTESIAN_POINT('Ctrl Pts',(3.18622713333614,-0.48390583353325,18.0338564078719));
#15686=CARTESIAN_POINT('Ctrl Pts',(3.18478372254885,-0.493316164802716,
18.0332748407883));
#15687=CARTESIAN_POINT('Ctrl Pts',(3.1818967594068,-0.51159685385526,18.0321417069418));
#15688=CARTESIAN_POINT('Ctrl Pts',(3.18045775695675,-0.520467849159643,
18.0315902896153));
#15689=CARTESIAN_POINT('Ctrl Pts',(3.17713467290383,-0.540425098259222,
18.0303462202271));
#15690=CARTESIAN_POINT('Ctrl Pts',(3.17522964020086,-0.551507700262921,
18.0296529066549));
#15691=CARTESIAN_POINT('Ctrl Pts',(3.16995782196972,-0.581243711561549,
18.0277859357877));
#15692=CARTESIAN_POINT('Ctrl Pts',(3.1664844469219,-0.599877544118552,18.0266088912479));
#15693=CARTESIAN_POINT('Ctrl Pts',(3.15020371932445,-0.683135701098123,
18.0213170605459));
#15694=CARTESIAN_POINT('Ctrl Pts',(3.13558168493726,-0.747384993437679,
18.0171446573807));
#15695=CARTESIAN_POINT('Ctrl Pts',(3.10890837852777,-0.849949719402033,
18.0103355714641));
#15696=CARTESIAN_POINT('Ctrl Pts',(3.09809153218779,-0.888568778876834,
18.0077373744094));
#15697=CARTESIAN_POINT('Ctrl Pts',(3.06668922412087,-0.993129369458341,
18.0006099834175));
#15698=CARTESIAN_POINT('Ctrl Pts',(3.04470054740792,-1.05862476740318,17.9960433794611));
#15699=CARTESIAN_POINT('Ctrl Pts',(2.93043316240378,-1.36588065604806,17.9741683430614));
#15700=CARTESIAN_POINT('Ctrl Pts',(2.81136758919853,-1.5966455715593,17.9562941713203));
#15701=CARTESIAN_POINT('Ctrl Pts',(2.63770576812585,-1.85233932593556,17.936142975609));
#15702=CARTESIAN_POINT('Ctrl Pts',(2.60844262724126,-1.89332523048227,17.9329044844578));
#15703=CARTESIAN_POINT('Ctrl Pts',(2.57145644568551,-1.94264168891284,17.9290136953903));
#15704=CARTESIAN_POINT('Ctrl Pts',(2.56463620711472,-1.95163677912571,17.9283042852724));
#15705=CARTESIAN_POINT('Ctrl Pts',(2.55386159912693,-1.96569319631275,17.9271963481542));
#15706=CARTESIAN_POINT('Ctrl Pts',(2.54993920092933,-1.97077875034213,17.9267956339594));
#15707=CARTESIAN_POINT('Ctrl Pts',(2.54257202072558,-1.98027179274162,17.9260479370216));
#15708=CARTESIAN_POINT('Ctrl Pts',(2.53913100501961,-1.98468198803807,17.9257007084002));
#15709=CARTESIAN_POINT('Ctrl Pts',(2.53123508652209,-1.99474768526131,17.9249084728523));
#15710=CARTESIAN_POINT('Ctrl Pts',(2.52677271227889,-2.00039722404085,17.9244640066733));
#15711=CARTESIAN_POINT('Ctrl Pts',(2.51294295271654,-2.01778612238745,17.9230963890181));
#15712=CARTESIAN_POINT('Ctrl Pts',(2.50351225086715,-2.02947519061583,17.9221776493631));
#15713=CARTESIAN_POINT('Ctrl Pts',(2.40385725380719,-2.15124275853471,17.9126080672153));
#15714=CARTESIAN_POINT('Ctrl Pts',(2.30650440420755,-2.25530999285498,17.9044362802824));
#15715=CARTESIAN_POINT('Ctrl Pts',(2.06874167982989,-2.47790988873588,17.886057446617));
#15716=CARTESIAN_POINT('Ctrl Pts',(1.92445993656287,-2.59156023889675,17.8759620028464));
#15717=CARTESIAN_POINT('Ctrl Pts',(1.69034847326822,-2.74558344339987,17.8600440427088));
#15718=CARTESIAN_POINT('Ctrl Pts',(1.60704521374213,-2.79515829487832,17.85446386194));
#15719=CARTESIAN_POINT('Ctrl Pts',(1.48763613898095,-2.85911599057899,17.8464854752443));
#15720=CARTESIAN_POINT('Ctrl Pts',(1.45330927213291,-2.87671644517935,17.8441944455177));
#15721=CARTESIAN_POINT('Ctrl Pts',(1.39279862748717,-2.90638265272207,17.8401549113695));
#15722=CARTESIAN_POINT('Ctrl Pts',(1.36675312433593,-2.91872128779356,17.8384158914591));
#15723=CARTESIAN_POINT('Ctrl Pts',(1.32852772020526,-2.93620611107292,17.8358617185614));
#15724=CARTESIAN_POINT('Ctrl Pts',(1.31647560821576,-2.9416295135291,17.8350561397581));
#15725=CARTESIAN_POINT('Ctrl Pts',(1.29570867212515,-2.95082136747671,17.8336674404825));
#15726=CARTESIAN_POINT('Ctrl Pts',(1.28700986264378,-2.95462574891855,17.833085562513));
#15727=CARTESIAN_POINT('Ctrl Pts',(1.26968929143621,-2.96210981217899,17.8319265424967));
#15728=CARTESIAN_POINT('Ctrl Pts',(1.26106803239097,-2.96579042599213,17.8313494393696));
#15729=CARTESIAN_POINT('Ctrl Pts',(1.23847960553727,-2.97531764574597,17.829836782171));
#15730=CARTESIAN_POINT('Ctrl Pts',(1.22448720081539,-2.98110347167969,17.8288991698032));
#15731=CARTESIAN_POINT('Ctrl Pts',(1.17594884652967,-3.00077458105909,17.8256443111062));
#15732=CARTESIAN_POINT('Ctrl Pts',(1.1412044476014,-3.01415925211369,17.8233102688906));
#15733=CARTESIAN_POINT('Ctrl Pts',(1.09834236381055,-3.02982380113073,17.8204247154964));
#15734=CARTESIAN_POINT('Ctrl Pts',(1.09043642725761,-3.03267812502592,17.8198922203783));
#15735=CARTESIAN_POINT('Ctrl Pts',(0.747518494774859,-3.15496939851098,
17.7967841741866));
#15736=CARTESIAN_POINT('Ctrl Pts',(0.395077617771009,-3.21813806377519,
17.772171066051));
#15737=CARTESIAN_POINT('Ctrl Pts',(-0.0198095310532809,-3.22323680718099,
17.7446208297601));
#15738=CARTESIAN_POINT('Ctrl Pts',(-0.0792345535247083,-3.22232380114667,
17.7407189117324));
#15739=CARTESIAN_POINT('Ctrl Pts',(-0.161489729741018,-3.21878290181611,
17.7354079084667));
#15740=CARTESIAN_POINT('Ctrl Pts',(-0.184365289463808,-3.21755369916916,
17.7339405753569));
#15741=CARTESIAN_POINT('Ctrl Pts',(-0.2240003027912,-3.21499983758994,17.7314172197131));
#15742=CARTESIAN_POINT('Ctrl Pts',(-0.240765828266566,-3.2137877863793,
17.7303557495571));
#15743=CARTESIAN_POINT('Ctrl Pts',(-0.265034554699858,-3.21184231488938,
17.7288285314157));
#15744=CARTESIAN_POINT('Ctrl Pts',(-0.272545542442723,-3.21121368035888,
17.7283571606919));
#15745=CARTESIAN_POINT('Ctrl Pts',(-0.285668371530446,-3.2100689869704,
17.7275359450257));
#15746=CARTESIAN_POINT('Ctrl Pts',(-0.291281156137776,-3.20956455140521,
17.7271854525156));
#15747=CARTESIAN_POINT('Ctrl Pts',(-0.303098228047417,-3.20847126599808,
17.7264491389383));
#15748=CARTESIAN_POINT('Ctrl Pts',(-0.309302131199087,-3.20787914263887,
17.7260635042434));
#15749=CARTESIAN_POINT('Ctrl Pts',(-0.325883394367428,-3.20624801645108,
17.7250351964634));
#15750=CARTESIAN_POINT('Ctrl Pts',(-0.336257598355172,-3.20517661982347,
17.7243943248581));
#15751=CARTESIAN_POINT('Ctrl Pts',(-0.381505380560336,-3.20028154627505,
17.7216093122399));
#15752=CARTESIAN_POINT('Ctrl Pts',(-0.416321903141804,-3.19593877249969,
17.7194927826255));
#15753=CARTESIAN_POINT('Ctrl Pts',(-0.458313192895171,-3.19000316728307,
17.716964608063));
#15754=CARTESIAN_POINT('Ctrl Pts',(-0.46556074339324,-3.18895349388033,
17.7165291396256));
#15755=CARTESIAN_POINT('Ctrl Pts',(-0.769694187039384,-3.14384647410949,
17.6982901573871));
#15756=CARTESIAN_POINT('Ctrl Pts',(-1.05901076618924,-3.05855278755339,
17.6822134873302));
#15757=CARTESIAN_POINT('Ctrl Pts',(-1.38056708267961,-2.91255108091743,
17.6621009447274));
#15758=CARTESIAN_POINT('Ctrl Pts',(-1.42820932113431,-2.88948711399505,
17.6590625449461));
#15759=CARTESIAN_POINT('Ctrl Pts',(-1.47525542042047,-2.86526421242789,
17.6559915606006));
#15760=CARTESIAN_POINT('Ctrl Pts',(-1.47525540448706,-2.86526422063162,
17.4058265726261));
#15761=CARTESIAN_POINT('Ctrl Pts',(-1.45612575153564,-2.87511361731181,
17.4070443009508));
#15762=CARTESIAN_POINT('Ctrl Pts',(-1.43689277196508,-2.88477385269499,
17.4082657479273));
#15763=CARTESIAN_POINT('Ctrl Pts',(-1.33540932568462,-2.93447900172206,
17.4147004189395));
#15764=CARTESIAN_POINT('Ctrl Pts',(-1.25158913212826,-2.97119636113742,
17.4199813884629));
#15765=CARTESIAN_POINT('Ctrl Pts',(-1.11421716555984,-3.02452676453268,
17.4286717256038));
#15766=CARTESIAN_POINT('Ctrl Pts',(-1.06159419017941,-3.04339600551254,
17.432008406599));
#15767=CARTESIAN_POINT('Ctrl Pts',(-0.992220361865946,-3.06625348829933,
17.4364285173583));
#15768=CARTESIAN_POINT('Ctrl Pts',(-0.975888950667632,-3.07149026358307,
17.4374705632408));
#15769=CARTESIAN_POINT('Ctrl Pts',(-0.94916502936419,-3.07982481495259,
17.4391784747289));
#15770=CARTESIAN_POINT('Ctrl Pts',(-0.938797172099172,-3.08300097451808,
17.4398417523448));
#15771=CARTESIAN_POINT('Ctrl Pts',(-0.918760241051056,-3.08902877981518,
17.4411249844615));
#15772=CARTESIAN_POINT('Ctrl Pts',(-0.909093416116999,-3.09188750444613,
17.4417446979114));
#15773=CARTESIAN_POINT('Ctrl Pts',(-0.886830653444291,-3.0983577349787,
17.443173392985));
#15774=CARTESIAN_POINT('Ctrl Pts',(-0.874225848352245,-3.10193784910527,
17.443983390441));
#15775=CARTESIAN_POINT('Ctrl Pts',(-0.84045858751936,-3.11130652252011,
17.4461563921927));
#15776=CARTESIAN_POINT('Ctrl Pts',(-0.819258556591595,-3.11695593382606,
17.4475238945578));
#15777=CARTESIAN_POINT('Ctrl Pts',(-0.637465598794932,-3.16341758238275,
17.4592798946777));
#15778=CARTESIAN_POINT('Ctrl Pts',(-0.474028805680539,-3.19199854637558,
17.4700647636785));
#15779=CARTESIAN_POINT('Ctrl Pts',(-0.0520602623034604,-3.23266323718004,
17.4983527741121));
#15780=CARTESIAN_POINT('Ctrl Pts',(0.207054034465362,-3.22644491174887,
17.5161926589888));
#15781=CARTESIAN_POINT('Ctrl Pts',(0.512925487908727,-3.18207581288612,
17.5363480696752));
#15782=CARTESIAN_POINT('Ctrl Pts',(0.563031351146764,-3.17359345543301,
17.5396166830902));
#15783=CARTESIAN_POINT('Ctrl Pts',(0.624029143904995,-3.16177691512979,
17.5435383611158));
#15784=CARTESIAN_POINT('Ctrl Pts',(0.635128219274363,-3.15956607583364,
17.5442495996316));
#15785=CARTESIAN_POINT('Ctrl Pts',(0.652512403471344,-3.15600799054425,
17.5453596660837));
#15786=CARTESIAN_POINT('Ctrl Pts',(0.658805391426698,-3.15470035518508,
17.5457606958203));
#15787=CARTESIAN_POINT('Ctrl Pts',(0.670564923271226,-3.15222009115228,
17.5465085212806));
#15788=CARTESIAN_POINT('Ctrl Pts',(0.676032266710425,-3.15105207737857,
17.5468555654922));
#15789=CARTESIAN_POINT('Ctrl Pts',(0.68851966122885,-3.14835034101348,17.5476467755903));
#15790=CARTESIAN_POINT('Ctrl Pts',(0.695537627944248,-3.14680736686099,
17.5480904049825));
#15791=CARTESIAN_POINT('Ctrl Pts',(0.71386231002847,-3.14271419432294,17.5492462060343));
#15792=CARTESIAN_POINT('Ctrl Pts',(0.725160649341641,-3.14012642212542,
17.5499562764328));
#15793=CARTESIAN_POINT('Ctrl Pts',(0.799857766536948,-3.12259312881603,
17.5546353418392));
#15794=CARTESIAN_POINT('Ctrl Pts',(0.862809779745145,-3.10578829101587,
17.5585049655511));
#15795=CARTESIAN_POINT('Ctrl Pts',(0.94064497658008,-3.08246072137817,17.5632460170238));
#15796=CARTESIAN_POINT('Ctrl Pts',(0.956041436503322,-3.07772023705804,
17.5641816842582));
#15797=CARTESIAN_POINT('Ctrl Pts',(0.999474290684799,-3.06399012986382,
17.5668167182767));
#15798=CARTESIAN_POINT('Ctrl Pts',(1.02742435444135,-3.05473135401561,17.5685071624843));
#15799=CARTESIAN_POINT('Ctrl Pts',(1.27646377247133,-2.96842935815827,17.5835532989296));
#15800=CARTESIAN_POINT('Ctrl Pts',(1.48867332729716,-2.86788986957592,17.5963139995897));
#15801=CARTESIAN_POINT('Ctrl Pts',(1.78951810417125,-2.68289224549854,17.616471124758));
#15802=CARTESIAN_POINT('Ctrl Pts',(1.88737031194414,-2.61497889888649,17.6233938588013));
#15803=CARTESIAN_POINT('Ctrl Pts',(2.00457702756722,-2.52362126834575,17.6322979263554));
#15804=CARTESIAN_POINT('Ctrl Pts',(2.027665756965,-2.50510775311956,17.6340832592697));
#15805=CARTESIAN_POINT('Ctrl Pts',(2.06084179821304,-2.47774665658751,17.6366962003277));
#15806=CARTESIAN_POINT('Ctrl Pts',(2.07113442707925,-2.46914956775208,17.6375136478914));
#15807=CARTESIAN_POINT('Ctrl Pts',(2.08907879426095,-2.45397009440952,17.6389509366892));
#15808=CARTESIAN_POINT('Ctrl Pts',(2.09675387637832,-2.44741549621207,17.6395696297688));
#15809=CARTESIAN_POINT('Ctrl Pts',(2.11258558980024,-2.43376592056368,17.6408541010662));
#15810=CARTESIAN_POINT('Ctrl Pts',(2.12073755476609,-2.42666574739381,17.6415200909433));
#15811=CARTESIAN_POINT('Ctrl Pts',(2.14161706181175,-2.40829461365892,17.6432378565532));
#15812=CARTESIAN_POINT('Ctrl Pts',(2.15429129691026,-2.39696382447206,17.6442921360255));
#15813=CARTESIAN_POINT('Ctrl Pts',(2.20354447733288,-2.35222519811304,17.6484352167897));
#15814=CARTESIAN_POINT('Ctrl Pts',(2.2394392245659,-2.3180774718112,17.651555397475));
#15815=CARTESIAN_POINT('Ctrl Pts',(2.52114212272694,-2.03743400127064,17.676882874069));
#15816=CARTESIAN_POINT('Ctrl Pts',(2.72629240519677,-1.75343074881565,17.7009745820447));
#15817=CARTESIAN_POINT('Ctrl Pts',(2.9084817701896,-1.38937034365275,17.7280018457015));
#15818=CARTESIAN_POINT('Ctrl Pts',(2.93349290594752,-1.33575311400802,17.7318856011806));
#15819=CARTESIAN_POINT('Ctrl Pts',(2.96609490004213,-1.26052369690841,17.7371741338384));
#15820=CARTESIAN_POINT('Ctrl Pts',(2.97495177228867,-1.2394760843413,17.7386366668875));
#15821=CARTESIAN_POINT('Ctrl Pts',(2.98992246798089,-1.20281431434058,17.7411524961937));
#15822=CARTESIAN_POINT('Ctrl Pts',(2.9961394248586,-1.18724353630641,17.7422111994446));
#15823=CARTESIAN_POINT('Ctrl Pts',(3.00497141438551,-1.16461196419871,17.7437350845145));
#15824=CARTESIAN_POINT('Ctrl Pts',(3.00768354164911,-1.15758971334505,17.7442058571449));
#15825=CARTESIAN_POINT('Ctrl Pts',(3.01238189582363,-1.14529673009271,17.7450262901231));
#15826=CARTESIAN_POINT('Ctrl Pts',(3.01437894290325,-1.14003020871351,17.7453765951951));
#15827=CARTESIAN_POINT('Ctrl Pts',(3.01855692737781,-1.12892448357784,17.7461127831511));
#15828=CARTESIAN_POINT('Ctrl Pts',(3.02073473209977,-1.12308418797962,17.7464984784391));
#15829=CARTESIAN_POINT('Ctrl Pts',(3.02651483127294,-1.10744504630501,17.7475275056477));
#15830=CARTESIAN_POINT('Ctrl Pts',(3.03008651500919,-1.09763485416361,17.748169030717));
#15831=CARTESIAN_POINT('Ctrl Pts',(3.04549131867436,-1.05467487996011,17.7509617455538));
#15832=CARTESIAN_POINT('Ctrl Pts',(3.05682908966866,-1.02134843568971,17.7530851314645));
#15833=CARTESIAN_POINT('Ctrl Pts',(3.0715023371318,-0.975782481764143,17.755938623624));
#15834=CARTESIAN_POINT('Ctrl Pts',(3.0753144841719,-0.963700623448405,17.7566905184771));
#15835=CARTESIAN_POINT('Ctrl Pts',(3.17409445625344,-0.644080883971602,
17.7764650134878));
#15836=CARTESIAN_POINT('Ctrl Pts',(3.22254141043166,-0.324034029265177,
17.7935926669874));
#15837=CARTESIAN_POINT('Ctrl Pts',(3.22282044166776,0.108035746430257,17.8184236692774));
#15838=CARTESIAN_POINT('Ctrl Pts',(3.21724779405089,0.21807368094822,17.8248759566217));
#15839=CARTESIAN_POINT('Ctrl Pts',(3.2040066183689,0.347657188749756,17.8327224978492));
#15840=CARTESIAN_POINT('Ctrl Pts',(3.20176935274758,0.367691330990646,17.8339425495846));
#15841=CARTESIAN_POINT('Ctrl Pts',(3.19781499259019,0.400322921404961,17.8359416502096));
#15842=CARTESIAN_POINT('Ctrl Pts',(3.19621102356402,0.412933715995833,17.8367171221811));
#15843=CARTESIAN_POINT('Ctrl Pts',(3.19321229096217,0.435445516168138,17.8381067501153));
#15844=CARTESIAN_POINT('Ctrl Pts',(3.19184597583925,0.445350194386083,17.8387199968769));
#15845=CARTESIAN_POINT('Ctrl Pts',(3.18885901489756,0.466283169355085,17.8400200255195));
#15846=CARTESIAN_POINT('Ctrl Pts',(3.18722720255972,0.477309716199698,17.8407071546686));
#15847=CARTESIAN_POINT('Ctrl Pts',(3.18273185233956,0.506634525906609,17.8425408761129));
#15848=CARTESIAN_POINT('Ctrl Pts',(3.17976775608376,0.524916737218566,17.8436906510749));
#15849=CARTESIAN_POINT('Ctrl Pts',(3.16488131649599,0.611977458316588,17.8491980017644));
#15850=CARTESIAN_POINT('Ctrl Pts',(3.15088481514664,0.680377701780069,17.8536211727373));
#15851=CARTESIAN_POINT('Ctrl Pts',(3.0722107847683,1.00996372701713,17.8754206937213));
#15852=CARTESIAN_POINT('Ctrl Pts',(2.9772221379522,1.26277805420599,17.893766371748));
#15853=CARTESIAN_POINT('Ctrl Pts',(2.78674723024425,1.62473750826042,17.9213260861595));
#15854=CARTESIAN_POINT('Ctrl Pts',(2.71350851561203,1.74430876684402,17.9306470408837));
#15855=CARTESIAN_POINT('Ctrl Pts',(2.62406159944196,1.87100061137568,17.9404805789223));
#15856=CARTESIAN_POINT('Ctrl Pts',(2.61532452819609,1.88319414775847,17.9414264885495));
#15857=CARTESIAN_POINT('Ctrl Pts',(2.60227152039478,1.90114498447032,17.9428176970123));
#15858=CARTESIAN_POINT('Ctrl Pts',(2.59802107899454,1.90694934209511,17.9432673341457));
#15859=CARTESIAN_POINT('Ctrl Pts',(2.59043253064196,1.91723971695551,17.9440640421342));
#15860=CARTESIAN_POINT('Ctrl Pts',(2.58710215520272,1.92173132053647,17.944411640325));
#15861=CARTESIAN_POINT('Ctrl Pts',(2.5799218381257,1.93136275970628,17.9451566572599));
#15862=CARTESIAN_POINT('Ctrl Pts',(2.57606822990046,1.93649974877812,17.9455538131495));
#15863=CARTESIAN_POINT('Ctrl Pts',(2.5653966297188,1.95063712270634,17.9466463579134));
#15864=CARTESIAN_POINT('Ctrl Pts',(2.5585465749378,1.95961335087945,17.9473395321758));
#15865=CARTESIAN_POINT('Ctrl Pts',(2.52084339555108,2.00848440851368,17.951111831092));
#15866=CARTESIAN_POINT('Ctrl Pts',(2.4891023364133,2.04768924885605,17.9541318431589));
#15867=CARTESIAN_POINT('Ctrl Pts',(2.28909041658033,2.28320594578005,17.9723482904326));
#15868=CARTESIAN_POINT('Ctrl Pts',(2.09860524255749,2.45944120224401,17.9863684462292));
#15869=CARTESIAN_POINT('Ctrl Pts',(1.75475706810696,2.70821613460346,18.0103294489913));
#15870=CARTESIAN_POINT('Ctrl Pts',(1.61314684000517,2.79487988029072,18.0198778043431));
#15871=CARTESIAN_POINT('Ctrl Pts',(1.44596845230781,2.88023857575102,18.0311675990326));
#15872=CARTESIAN_POINT('Ctrl Pts',(1.4263252655106,2.8900164737955,18.0324940693776));
#15873=CARTESIAN_POINT('Ctrl Pts',(1.39479402428708,2.90531218800568,18.0346239255348));
#15874=CARTESIAN_POINT('Ctrl Pts',(1.38296928604833,2.91095950261216,18.0354227902043));
#15875=CARTESIAN_POINT('Ctrl Pts',(1.36198760539736,2.92082333392642,18.0368406660793));
#15876=CARTESIAN_POINT('Ctrl Pts',(1.3528446509083,2.92506932090614,18.0374586445365));
#15877=CARTESIAN_POINT('Ctrl Pts',(1.33382624617676,2.93379322418341,18.0387444424319));
#15878=CARTESIAN_POINT('Ctrl Pts',(1.32394782933076,2.93826433083612,18.0394124874795));
#15879=CARTESIAN_POINT('Ctrl Pts',(1.2983883234577,2.94967784950554,18.041141564178));
#15880=CARTESIAN_POINT('Ctrl Pts',(1.28267420156842,2.95654503240895,18.042205163103));
#15881=CARTESIAN_POINT('Ctrl Pts',(1.21552066309157,2.98525546664666,18.0467532827428));
#15882=CARTESIAN_POINT('Ctrl Pts',(1.16357512410711,3.005883062115,18.0502788037774));
#15883=CARTESIAN_POINT('Ctrl Pts',(1.02528184481835,3.05667749467831,18.0596900436848));
#15884=CARTESIAN_POINT('Ctrl Pts',(0.938145620133956,3.08453569894457,18.0656465561971));
#15885=CARTESIAN_POINT('Ctrl Pts',(0.6117131875876,3.17378696959399,18.0880286222714));
#15886=CARTESIAN_POINT('Ctrl Pts',(0.366805261952291,3.21131671021937,18.1050278394368));
#15887=CARTESIAN_POINT('Ctrl Pts',(0.0313047657450737,3.22382076755654,
18.1273374032897));
#15888=CARTESIAN_POINT('Ctrl Pts',(-0.0575265271992821,3.22345996427573,
18.1331421980008));
#15889=CARTESIAN_POINT('Ctrl Pts',(-0.16003808526958,3.2188035388841,18.1396412252152));
#15890=CARTESIAN_POINT('Ctrl Pts',(-0.173834755698983,3.21808792677811,
18.1405116985285));
#15891=CARTESIAN_POINT('Ctrl Pts',(-0.194665230427495,3.21687312776981,
18.1418191662402));
#15892=CARTESIAN_POINT('Ctrl Pts',(-0.201702489088259,3.21643955022421,
18.1422597030531));
#15893=CARTESIAN_POINT('Ctrl Pts',(-0.21430590901598,3.21562150574251,18.1430465178));
#15894=CARTESIAN_POINT('Ctrl Pts',(-0.219872524467502,3.21524567729424,
18.143393272275));
#15895=CARTESIAN_POINT('Ctrl Pts',(-0.23194415688964,3.21439916706936,18.1441435748152));
#15896=CARTESIAN_POINT('Ctrl Pts',(-0.23844870982701,3.21392319630281,18.1445468220878));
#15897=CARTESIAN_POINT('Ctrl Pts',(-0.256666856056883,3.21253447087215,
18.1456734525681));
#15898=CARTESIAN_POINT('Ctrl Pts',(-0.268377110289065,3.21157739095852,
18.1463943875404));
#15899=CARTESIAN_POINT('Ctrl Pts',(-0.337499059629746,3.20554733960997,
18.1506320763358));
#15900=CARTESIAN_POINT('Ctrl Pts',(-0.394775523023678,3.19899868746676,
18.1540711706208));
#15901=CARTESIAN_POINT('Ctrl Pts',(-0.702324638331072,3.15544822325933,
18.1722941354599));
#15902=CARTESIAN_POINT('Ctrl Pts',(-0.947775027874227,3.0906087361959,18.1860247379155));
#15903=CARTESIAN_POINT('Ctrl Pts',(-1.33514323720598,2.93772300548985,18.2095503232889));
#15904=CARTESIAN_POINT('Ctrl Pts',(-1.48235002958322,2.86626096733015,18.2189687358203));
#15905=CARTESIAN_POINT('Ctrl Pts',(-1.64240637987474,2.77292232708381,18.2301131129387));
#15906=CARTESIAN_POINT('Ctrl Pts',(-1.6612068788083,2.76170031289673,18.2314367682599));
#15907=CARTESIAN_POINT('Ctrl Pts',(-1.69106248285487,2.7434643424562,18.2335629569377));
#15908=CARTESIAN_POINT('Ctrl Pts',(-1.70219193274676,2.73657295451891,18.2343609939906));
#15909=CARTESIAN_POINT('Ctrl Pts',(-1.72181540523769,2.72425601806597,18.2357779119073));
#15910=CARTESIAN_POINT('Ctrl Pts',(-1.73032658930183,2.71885803828966,18.2363957646589));
#15911=CARTESIAN_POINT('Ctrl Pts',(-1.74794677968179,2.70756667920123,18.2376818105535));
#15912=CARTESIAN_POINT('Ctrl Pts',(-1.75705161524303,2.70166705640866,18.2383502318377));
#15913=CARTESIAN_POINT('Ctrl Pts',(-1.78049375351206,2.68630872756395,18.240081377511));
#15914=CARTESIAN_POINT('Ctrl Pts',(-1.79478539634146,2.6767812665121,18.2411466808569));
#15915=CARTESIAN_POINT('Ctrl Pts',(-1.85545430813714,2.63563230046035,18.2457119695986));
#15916=CARTESIAN_POINT('Ctrl Pts',(-1.90107499766036,2.60291788705741,18.2492533414002));
#15917=CARTESIAN_POINT('Ctrl Pts',(-2.01916376293855,2.51347597222458,18.2587176474169));
#15918=CARTESIAN_POINT('Ctrl Pts',(-2.09009266109183,2.45481036023131,18.2647123721423));
#15919=CARTESIAN_POINT('Ctrl Pts',(-2.33802641140208,2.23120024137729,18.2868002331147));
#15920=CARTESIAN_POINT('Ctrl Pts',(-2.49881685709087,2.04951737930807,18.303434122281));
#15921=CARTESIAN_POINT('Ctrl Pts',(-2.69107138038537,1.77562972968123,18.3257032110472));
#15922=CARTESIAN_POINT('Ctrl Pts',(-2.74107900340771,1.69741435656781,18.3317783952958));
#15923=CARTESIAN_POINT('Ctrl Pts',(-2.7946469161099,1.60507347299005,18.3385405136848));
#15924=CARTESIAN_POINT('Ctrl Pts',(-2.80156991802783,1.59295896067324,18.339419782127));
#15925=CARTESIAN_POINT('Ctrl Pts',(-2.81188697164123,1.57462990789696,18.3407378267085));
#15926=CARTESIAN_POINT('Ctrl Pts',(-2.81533947349657,1.5684487047318,18.3411802291892));
#15927=CARTESIAN_POINT('Ctrl Pts',(-2.82147728786471,1.55737427405552,18.3419690529458));
#15928=CARTESIAN_POINT('Ctrl Pts',(-2.82417027513916,1.55248541829707,18.3423159612009));
#15929=CARTESIAN_POINT('Ctrl Pts',(-2.82997206078908,1.54188778783922,18.3430650923667));
#15930=CARTESIAN_POINT('Ctrl Pts',(-2.83307628355408,1.53617661369418,18.3434670225946));
#15931=CARTESIAN_POINT('Ctrl Pts',(-2.84169552640974,1.52020387139251,18.3445862582335));
#15932=CARTESIAN_POINT('Ctrl Pts',(-2.84717228359785,1.5099216114046,18.3453011669901));
#15933=CARTESIAN_POINT('Ctrl Pts',(-2.87863828516783,1.45006623422994,18.349431806165));
#15934=CARTESIAN_POINT('Ctrl Pts',(-2.90339004261751,1.39984913486108,18.3527743805958));
#15935=CARTESIAN_POINT('Ctrl Pts',(-3.03322489957583,1.11815826409865,18.3709913416747));
#15936=CARTESIAN_POINT('Ctrl Pts',(-3.11195176420353,0.875508309364952,
18.3847853205575));
#15937=CARTESIAN_POINT('Ctrl Pts',(-3.19321191555972,0.465208420673437,
18.4084102668637));
#15938=CARTESIAN_POINT('Ctrl Pts',(-3.21274434882842,0.302133241127508,
18.4178616161261));
#15939=CARTESIAN_POINT('Ctrl Pts',(-3.22072151790662,0.1164061052905,18.4290428354201));
#15940=CARTESIAN_POINT('Ctrl Pts',(-3.22143836837094,0.0945107387812838,
18.4303672102604));
#15941=CARTESIAN_POINT('Ctrl Pts',(-3.22222693543087,0.0595196439731538,
18.4324943363956));
#15942=CARTESIAN_POINT('Ctrl Pts',(-3.22244216114432,0.0464275949480485,
18.4332925850442));
#15943=CARTESIAN_POINT('Ctrl Pts',(-3.22268185015237,0.0232560852781683,
18.4347097478172));
#15944=CARTESIAN_POINT('Ctrl Pts',(-3.22273882181897,0.0131770815811676,
18.4353276326444));
#15945=CARTESIAN_POINT('Ctrl Pts',(-3.22275893885171,-0.00774956298596178,
18.4366136148195));
#15946=CARTESIAN_POINT('Ctrl Pts',(-3.2227145976839,-0.0185970681394861,
18.4372819396603));
#15947=CARTESIAN_POINT('Ctrl Pts',(-3.22245862833361,-0.046612614277827,
18.4390125550256));
#15948=CARTESIAN_POINT('Ctrl Pts',(-3.22216457033418,-0.0637793887244116,
18.4400774215106));
#15949=CARTESIAN_POINT('Ctrl Pts',(-3.22032514702766,-0.136993269624943,
18.444638303431));
#15950=CARTESIAN_POINT('Ctrl Pts',(-3.21745453969237,-0.192994446388077,
18.448175605989));
#15951=CARTESIAN_POINT('Ctrl Pts',(-3.20603011011104,-0.340482031065212,
18.4576262782298));
#15952=CARTESIAN_POINT('Ctrl Pts',(-3.19502283927822,-0.431721692830996,
18.4636111815406));
#15953=CARTESIAN_POINT('Ctrl Pts',(-3.14068799958351,-0.762512781591523,
18.4857867267707));
#15954=CARTESIAN_POINT('Ctrl Pts',(-3.07417094454756,-0.997399013706139,
18.5025275184392));
#15955=CARTESIAN_POINT('Ctrl Pts',(-2.94711902925174,-1.3072849562709,18.5248062695083));
#15956=CARTESIAN_POINT('Ctrl Pts',(-2.9087782588942,-1.39050959865773,18.5308000860973));
#15957=CARTESIAN_POINT('Ctrl Pts',(-2.86058575656031,-1.48437200659344,
18.5374831954123));
#15958=CARTESIAN_POINT('Ctrl Pts',(-2.8541509164316,-1.49670761582106,18.5383599118175));
#15959=CARTESIAN_POINT('Ctrl Pts',(-2.84432517987452,-1.51524976111916,
18.5396748883754));
#15960=CARTESIAN_POINT('Ctrl Pts',(-2.84099350732603,-1.52148725299845,
18.5401167504258));
#15961=CARTESIAN_POINT('Ctrl Pts',(-2.83499575726047,-1.53262773184451,
18.5409049911504));
#15962=CARTESIAN_POINT('Ctrl Pts',(-2.83233745923613,-1.53753478877048,
18.5412518537816));
#15963=CARTESIAN_POINT('Ctrl Pts',(-2.82655233887873,-1.54814785195048,
18.5420013193396));
#15964=CARTESIAN_POINT('Ctrl Pts',(-2.82342098920803,-1.55385128483619,
18.542403627253));
#15965=CARTESIAN_POINT('Ctrl Pts',(-2.81462113180413,-1.56976489458433,
18.5435249819914));
#15966=CARTESIAN_POINT('Ctrl Pts',(-2.80891430043262,-1.5799539241454,18.5442416174317));
#15967=CARTESIAN_POINT('Ctrl Pts',(-2.77530316458965,-1.639205808861,18.5484025631841));
#15968=CARTESIAN_POINT('Ctrl Pts',(-2.74616729720722,-1.68756315886799,
18.551772456958));
#15969=CARTESIAN_POINT('Ctrl Pts',(-2.57910444111927,-1.94904447804319,
18.5699908557284));
#15970=CARTESIAN_POINT('Ctrl Pts',(-2.41762815720409,-2.14607905625322,
18.5837667029164));
#15971=CARTESIAN_POINT('Ctrl Pts',(-2.1166709531064,-2.43570250297297,18.6073593806759));
#15972=CARTESIAN_POINT('Ctrl Pts',(-1.99018748854851,-2.54009565574716,
18.6167973163546));
#15973=CARTESIAN_POINT('Ctrl Pts',(-1.83839186153147,-2.64705769737862,
18.6279659805628));
#15974=CARTESIAN_POINT('Ctrl Pts',(-1.8203258116047,-2.65951367601743,18.629292548026));
#15975=CARTESIAN_POINT('Ctrl Pts',(-1.79127010416872,-2.67911192493322,
18.6314225307015));
#15976=CARTESIAN_POINT('Ctrl Pts',(-1.78036143893364,-2.68637347202601,
18.632221423913));
#15977=CARTESIAN_POINT('Ctrl Pts',(-1.76098332835991,-2.69910298136446,
18.633639332837));
#15978=CARTESIAN_POINT('Ctrl Pts',(-1.75253189703156,-2.70459814630406,
18.6342573156413));
#15979=CARTESIAN_POINT('Ctrl Pts',(-1.73493688792836,-2.71592141412555,
18.6355431050426));
#15980=CARTESIAN_POINT('Ctrl Pts',(-1.72578941272728,-2.72174319712899,
18.636211137162));
#15981=CARTESIAN_POINT('Ctrl Pts',(-1.70209976081654,-2.7366527047816,18.6379401427575));
#15982=CARTESIAN_POINT('Ctrl Pts',(-1.68751426088323,-2.74567063271529,
18.6390036831066));
#15983=CARTESIAN_POINT('Ctrl Pts',(-1.62509861138716,-2.78357580128347,
18.6435512138504));
#15984=CARTESIAN_POINT('Ctrl Pts',(-1.57659588191112,-2.81133145193748,
18.6470761913566));
#15985=CARTESIAN_POINT('Ctrl Pts',(-1.51009990082008,-2.84712166642673,
18.6519001379075));
#15986=CARTESIAN_POINT('Ctrl Pts',(-1.49271811462675,-2.85627309264525,
18.6531602851047));
#15987=CARTESIAN_POINT('Ctrl Pts',(-1.47525539597219,-2.86526422501572,
18.654425498672));
#15988=CARTESIAN_POINT('Origin',(0.,0.,4.68922655072688));
#15989=CARTESIAN_POINT('',(-1.4752556264295,-2.8652641063588,20.1529125281009));
#15990=CARTESIAN_POINT('',(-1.47525540330815,-2.86526422123861,19.9090518554891));
#15991=CARTESIAN_POINT('',(-1.47525540501186,-2.86526422036142,4.68922655072688));
#15992=CARTESIAN_POINT('Ctrl Pts',(-1.4752556264295,-2.8652641063588,20.1529125281009));
#15993=CARTESIAN_POINT('Ctrl Pts',(-1.58150907081783,-2.81055676147094,
20.1448299054891));
#15994=CARTESIAN_POINT('Ctrl Pts',(-1.68472792541289,-2.74993488249402,
20.1367792763065));
#15995=CARTESIAN_POINT('Ctrl Pts',(-1.83114972518741,-2.65257561597443,
20.1252774331368));
#15996=CARTESIAN_POINT('Ctrl Pts',(-1.87706363638319,-2.62028619182486,
20.1216588491543));
#15997=CARTESIAN_POINT('Ctrl Pts',(-1.93147404658425,-2.57985688621777,
20.1173782547665));
#15998=CARTESIAN_POINT('Ctrl Pts',(-1.94079651661166,-2.57285103278714,
20.1166451165578));
#15999=CARTESIAN_POINT('Ctrl Pts',(-1.95525918022703,-2.56185897430235,
20.1155084529471));
#16000=CARTESIAN_POINT('Ctrl Pts',(-1.96042556803217,-2.55790763321436,
20.1151025536105));
#16001=CARTESIAN_POINT('Ctrl Pts',(-1.97000465665147,-2.55053531419898,
20.1143502899173));
#16002=CARTESIAN_POINT('Ctrl Pts',(-1.97442038699685,-2.54711854304556,
20.1140036484861));
#16003=CARTESIAN_POINT('Ctrl Pts',(-1.98441579419683,-2.53934275940705,
20.1132192755135));
#16004=CARTESIAN_POINT('Ctrl Pts',(-1.98998998592631,-2.53497683464435,
20.1127820434794));
#16005=CARTESIAN_POINT('Ctrl Pts',(-2.00650207559223,-2.52195589310432,
20.1114872815208));
#16006=CARTESIAN_POINT('Ctrl Pts',(-2.01739839043408,-2.51324806907348,
20.1106334244813));
#16007=CARTESIAN_POINT('Ctrl Pts',(-2.10015011911816,-2.44623180122144,
20.1041501092195));
#16008=CARTESIAN_POINT('Ctrl Pts',(-2.16952796855151,-2.38491769116596,
20.0987216065889));
#16009=CARTESIAN_POINT('Ctrl Pts',(-2.41055768199051,-2.15266626570666,
20.0794825403089));
#16010=CARTESIAN_POINT('Ctrl Pts',(-2.56545013902381,-1.96551235365663,
20.0663155778298));
#16011=CARTESIAN_POINT('Ctrl Pts',(-2.74822324564669,-1.68577691012337,
20.0472923993586));
#16012=CARTESIAN_POINT('Ctrl Pts',(-2.79520317876447,-1.60667733424567,
20.041984409537));
#16013=CARTESIAN_POINT('Ctrl Pts',(-2.8652997216595,-1.47625333857415,20.033253450469));
#16014=CARTESIAN_POINT('Ctrl Pts',(-2.89056812406987,-1.42614226424106,
20.0299040493047));
#16015=CARTESIAN_POINT('Ctrl Pts',(-2.92184569172013,-1.35986411281836,
20.0254692123888));
#16016=CARTESIAN_POINT('Ctrl Pts',(-2.92905251293947,-1.3442708098536,20.0244255044938));
#16017=CARTESIAN_POINT('Ctrl Pts',(-2.94060812459597,-1.31873393349066,
20.0227154025471));
#16018=CARTESIAN_POINT('Ctrl Pts',(-2.94503201840642,-1.30882456264583,
20.022051607653));
#16019=CARTESIAN_POINT('Ctrl Pts',(-2.95346938574099,-1.28966577351694,
20.020767748919));
#16020=CARTESIAN_POINT('Ctrl Pts',(-2.95748967348966,-1.28041948103156,
20.0201479283208));
#16021=CARTESIAN_POINT('Ctrl Pts',(-2.96663237393668,-1.25911931682916,
20.0187195215883));
#16022=CARTESIAN_POINT('Ctrl Pts',(-2.97172480178461,-1.24705284187155,
20.0179099225834));
#16023=CARTESIAN_POINT('Ctrl Pts',(-2.98513939882458,-1.21471823187708,
20.0157391763686));
#16024=CARTESIAN_POINT('Ctrl Pts',(-2.99332855008379,-1.19439598384677,
20.0143735475846));
#16025=CARTESIAN_POINT('Ctrl Pts',(-3.0610310977998,-1.02131450143205,20.002729642939));
#16026=CARTESIAN_POINT('Ctrl Pts',(-3.10900619999056,-0.864326578313328,
19.9920637161607));
#16027=CARTESIAN_POINT('Ctrl Pts',(-3.20042614120463,-0.456172900680657,
19.9641661210332));
#16028=CARTESIAN_POINT('Ctrl Pts',(-3.22643892361054,-0.202258031982122,
19.9466067707527));
#16029=CARTESIAN_POINT('Ctrl Pts',(-3.22142602316887,0.107972034062188,
19.926313550146));
#16030=CARTESIAN_POINT('Ctrl Pts',(-3.21906799093133,0.163846730134829,
19.9227086017824));
#16031=CARTESIAN_POINT('Ctrl Pts',(-3.21446315792113,0.231257128744744,
19.918441914501));
#16032=CARTESIAN_POINT('Ctrl Pts',(-3.21360626694635,0.242874502679417,
19.9177095752111));
#16033=CARTESIAN_POINT('Ctrl Pts',(-3.2121730023703,0.260968261074762,19.9165738779011));
#16034=CARTESIAN_POINT('Ctrl Pts',(-3.21163999934969,0.267447839391077,
19.9161681523385));
#16035=CARTESIAN_POINT('Ctrl Pts',(-3.21061279111775,0.279489257392999,
19.9154160452666));
#16036=CARTESIAN_POINT('Ctrl Pts',(-3.21012374463268,0.285051371403494,
19.9150693877194));
#16037=CARTESIAN_POINT('Ctrl Pts',(-3.20898141921467,0.297667597554251,
19.9142847674698));
#16038=CARTESIAN_POINT('Ctrl Pts',(-3.20831933684626,0.304720827283359,
19.9138473055874));
#16039=CARTESIAN_POINT('Ctrl Pts',(-3.20628294834694,0.325672006859688,
19.9125512314547));
#16040=CARTESIAN_POINT('Ctrl Pts',(-3.20484153427973,0.339563480716554,
19.9116963031328));
#16041=CARTESIAN_POINT('Ctrl Pts',(-3.19310183453127,0.44596150386417,19.905179108522));
#16042=CARTESIAN_POINT('Ctrl Pts',(-3.17888955565601,0.538001568397257,
19.8997201786849));
#16043=CARTESIAN_POINT('Ctrl Pts',(-3.11355387372116,0.866152352006445,
19.8804933316663));
#16044=CARTESIAN_POINT('Ctrl Pts',(-3.0399242278032,1.09695529577948,19.8673605761409));
#16045=CARTESIAN_POINT('Ctrl Pts',(-2.90357876720631,1.40136242090686,19.8483724114345));
#16046=CARTESIAN_POINT('Ctrl Pts',(-2.86238353099329,1.4836929866749,19.8430609684286));
#16047=CARTESIAN_POINT('Ctrl Pts',(-2.79047631111842,1.61323012332937,19.8343248481446));
#16048=CARTESIAN_POINT('Ctrl Pts',(-2.76195151809205,1.66159342433065,19.8309738528987));
#16049=CARTESIAN_POINT('Ctrl Pts',(-2.7230673863931,1.72375078348942,19.8265371988607));
#16050=CARTESIAN_POINT('Ctrl Pts',(-2.71383917252834,1.73824327477094,19.8254933113669));
#16051=CARTESIAN_POINT('Ctrl Pts',(-2.69859350641019,1.76176855212355,19.8237829890729));
#16052=CARTESIAN_POINT('Ctrl Pts',(-2.69264545031103,1.77084607418422,19.8231191547228));
#16053=CARTESIAN_POINT('Ctrl Pts',(-2.68108336264871,1.78829841403298,19.8218352715958));
#16054=CARTESIAN_POINT('Ctrl Pts',(-2.67547565072834,1.79667728147751,19.8212154663399));
#16055=CARTESIAN_POINT('Ctrl Pts',(-2.66249406823364,1.81587840811226,19.8197871693867));
#16056=CARTESIAN_POINT('Ctrl Pts',(-2.65509340388234,1.82668225615488,19.8189776653276));
#16057=CARTESIAN_POINT('Ctrl Pts',(-2.6351381933721,1.85543636043771,19.8168073392544));
#16058=CARTESIAN_POINT('Ctrl Pts',(-2.62246630946823,1.87330398046892,19.8154420383921));
#16059=CARTESIAN_POINT('Ctrl Pts',(-2.51356803836523,2.02358229134073,19.8038147869979));
#16060=CARTESIAN_POINT('Ctrl Pts',(-2.40757998259418,2.1485933910969,19.7931664667038));
#16061=CARTESIAN_POINT('Ctrl Pts',(-2.11417688084498,2.44556808878349,19.7653240969013));
#16062=CARTESIAN_POINT('Ctrl Pts',(-1.9150838537895,2.60441857064274,19.7478035137965));
#16063=CARTESIAN_POINT('Ctrl Pts',(-1.65129683131018,2.76813011624045,19.7274896915165));
#16064=CARTESIAN_POINT('Ctrl Pts',(-1.602389759136,2.79672550612217,19.7238366312137));
#16065=CARTESIAN_POINT('Ctrl Pts',(-1.54250491723111,2.82965242776748,19.7195208984084));
#16066=CARTESIAN_POINT('Ctrl Pts',(-1.53222811654846,2.83523037695365,19.7187857564271));
#16067=CARTESIAN_POINT('Ctrl Pts',(-1.51618177126293,2.84382713819689,19.7176466695234));
#16068=CARTESIAN_POINT('Ctrl Pts',(-1.51043317629794,2.84688453878517,19.7172403346019));
#16069=CARTESIAN_POINT('Ctrl Pts',(-1.49973850177118,2.85253100850274,19.7164876772946));
#16070=CARTESIAN_POINT('Ctrl Pts',(-1.49479500791652,2.85512462305829,19.7161410752378));
#16071=CARTESIAN_POINT('Ctrl Pts',(-1.48357465924153,2.86097427310295,19.7153573174425));
#16072=CARTESIAN_POINT('Ctrl Pts',(-1.47729382795224,2.86422249642826,19.7149206579408));
#16073=CARTESIAN_POINT('Ctrl Pts',(-1.45863136126096,2.8737963444861,19.7136291617364));
#16074=CARTESIAN_POINT('Ctrl Pts',(-1.4462192378485,2.88006263992137,19.7127779705053));
#16075=CARTESIAN_POINT('Ctrl Pts',(-1.35206956634523,2.9268322306399,19.7063770091189));
#16076=CARTESIAN_POINT('Ctrl Pts',(-1.2686777431929,2.96393304996601,19.701022470257));
#16077=CARTESIAN_POINT('Ctrl Pts',(-0.957054131969724,3.0870060763848,19.6817522891793));
#16078=CARTESIAN_POINT('Ctrl Pts',(-0.720854904344486,3.15054610207915,
19.668501139492));
#16079=CARTESIAN_POINT('Ctrl Pts',(-0.388962476747943,3.20050818343474,
19.6493922600195));
#16080=CARTESIAN_POINT('Ctrl Pts',(-0.297650857714207,3.21028760149491,
19.644093403267));
#16081=CARTESIAN_POINT('Ctrl Pts',(-0.15012324660166,3.21973932758882,19.6353760964909));
#16082=CARTESIAN_POINT('Ctrl Pts',(-0.0941142254685356,3.22186285627564,
19.6320309136472));
#16083=CARTESIAN_POINT('Ctrl Pts',(-0.0209117142161527,3.2227278941025,
19.6276008855463));
#16084=CARTESIAN_POINT('Ctrl Pts',(-0.00374160312160156,3.22279356488666,
19.6265576533029));
#16085=CARTESIAN_POINT('Ctrl Pts',(0.024278181707385,3.22267681621623,19.6248481349166));
#16086=CARTESIAN_POINT('Ctrl Pts',(0.0351280006634178,3.22257681225764,
19.6241844445094));
#16087=CARTESIAN_POINT('Ctrl Pts',(0.0560591366900466,3.22227817014431,
19.622900650278));
#16088=CARTESIAN_POINT('Ctrl Pts',(0.0661404460757551,3.22208700538951,
19.6222807889551));
#16089=CARTESIAN_POINT('Ctrl Pts',(0.0893180377935905,3.22153868352731,
19.6208520910531));
#16090=CARTESIAN_POINT('Ctrl Pts',(0.102413304188272,3.22114897331931,19.6200422402536));
#16091=CARTESIAN_POINT('Ctrl Pts',(0.137415421972493,3.21989366573872,19.6178703796962));
#16092=CARTESIAN_POINT('Ctrl Pts',(0.159316127206305,3.21888436420238,19.6165038811304));
#16093=CARTESIAN_POINT('Ctrl Pts',(0.345579019831747,3.20839483362228,19.6048155857783));
#16094=CARTESIAN_POINT('Ctrl Pts',(0.50897657726643,3.18655773930985,19.5941027114151));
#16095=CARTESIAN_POINT('Ctrl Pts',(0.920293432848455,3.09914011912911,19.5660507218547));
#16096=CARTESIAN_POINT('Ctrl Pts',(1.16337590182619,3.01631590251475,19.5483803251273));
#16097=CARTESIAN_POINT('Ctrl Pts',(1.44267641763328,2.88230902421551,19.5281421813263));
#16098=CARTESIAN_POINT('Ctrl Pts',(1.49066523205695,2.85778559960499,19.5246712743163));
#16099=CARTESIAN_POINT('Ctrl Pts',(1.54814494884393,2.82656992430758,19.5205415936416));
#16100=CARTESIAN_POINT('Ctrl Pts',(1.55824082667222,2.82101681228522,19.5198173071995));
#16101=CARTESIAN_POINT('Ctrl Pts',(1.57396235251129,2.81225923136103,19.518691353531));
#16102=CARTESIAN_POINT('Ctrl Pts',(1.57960837523857,2.80909182016631,19.5182873827851));
#16103=CARTESIAN_POINT('Ctrl Pts',(1.59010907634868,2.80315927132294,19.5175368439194));
#16104=CARTESIAN_POINT('Ctrl Pts',(1.59496605857384,2.80039855159085,19.5171900102636));
#16105=CARTESIAN_POINT('Ctrl Pts',(1.60599937265803,2.79408917454232,19.516402832119));
#16106=CARTESIAN_POINT('Ctrl Pts',(1.61217112067303,2.79053266962419,19.5159630019649));
#16107=CARTESIAN_POINT('Ctrl Pts',(1.63098363640777,2.77960860674593,19.5146236873949));
#16108=CARTESIAN_POINT('Ctrl Pts',(1.64358627478455,2.77217528396755,19.5137283547015));
#16109=CARTESIAN_POINT('Ctrl Pts',(1.81834669798318,2.66748689738016,19.5013328501473));
#16110=CARTESIAN_POINT('Ctrl Pts',(1.97171501116726,2.55621453241845,19.4906847032626));
#16111=CARTESIAN_POINT('Ctrl Pts',(2.22632928955124,2.33485562904533,19.4718063333693));
#16112=CARTESIAN_POINT('Ctrl Pts',(2.33135668770654,2.22999264012755,19.4635740262155));
#16113=CARTESIAN_POINT('Ctrl Pts',(2.48772705920942,2.05070032794521,19.4500155588232));
#16114=CARTESIAN_POINT('Ctrl Pts',(2.54381445235653,1.98069785013082,19.4448346071155));
#16115=CARTESIAN_POINT('Ctrl Pts',(2.62954086749114,1.8640464455862,19.4362937802165));
#16116=CARTESIAN_POINT('Ctrl Pts',(2.6610281800176,1.81881357012862,19.433003349463));
#16117=CARTESIAN_POINT('Ctrl Pts',(2.70072714124068,1.7585453463084,19.428635774692));
#16118=CARTESIAN_POINT('Ctrl Pts',(2.71000169836993,1.744218909385,19.4275987680179));
#16119=CARTESIAN_POINT('Ctrl Pts',(2.72497357010668,1.72068411948888,19.425896886214));
#16120=CARTESIAN_POINT('Ctrl Pts',(2.73073911634198,1.71151940415405,19.42523456219));
#16121=CARTESIAN_POINT('Ctrl Pts',(2.74178891683205,1.69375704825495,19.4239515985712));
#16122=CARTESIAN_POINT('Ctrl Pts',(2.74707919256204,1.68516328854851,19.4233311917428));
#16123=CARTESIAN_POINT('Ctrl Pts',(2.7591721815659,1.66531062372396,19.4218986246328));
#16124=CARTESIAN_POINT('Ctrl Pts',(2.76594646278878,1.6540346906137,19.4210854322));
#16125=CARTESIAN_POINT('Ctrl Pts',(2.78391987389931,1.62369837462909,19.4188987642791));
#16126=CARTESIAN_POINT('Ctrl Pts',(2.79499207600717,1.60456396936572,19.4175207033215));
#16127=CARTESIAN_POINT('Ctrl Pts',(2.91479996675928,1.39251501572033,19.4022591189098));
#16128=CARTESIAN_POINT('Ctrl Pts',(3.00355053241839,1.18903596725833,19.3876437110219));
#16129=CARTESIAN_POINT('Ctrl Pts',(3.11860587063777,0.827823499110241,19.3620682756189));
#16130=CARTESIAN_POINT('Ctrl Pts',(3.15537866889177,0.674226593354248,19.3513167057866));
#16131=CARTESIAN_POINT('Ctrl Pts',(3.19075236969728,0.457247319535713,19.3366982276522));
#16132=CARTESIAN_POINT('Ctrl Pts',(3.19897302871177,0.395661876423688,19.3326133971996));
#16133=CARTESIAN_POINT('Ctrl Pts',(3.20785573059182,0.310382054362313,19.3270780147799));
#16134=CARTESIAN_POINT('Ctrl Pts',(3.21004436785005,0.286863443872466,19.3255641214724));
#16135=CARTESIAN_POINT('Ctrl Pts',(3.21338092958647,0.246164437055192,19.3229686007711));
#16136=CARTESIAN_POINT('Ctrl Pts',(3.21465007854317,0.228995266056595,19.3218811141053));
#16137=CARTESIAN_POINT('Ctrl Pts',(3.21628184103584,0.204221952866047,19.3203235210708));
#16138=CARTESIAN_POINT('Ctrl Pts',(3.21675516676079,0.196625753492516,19.3198474815529));
#16139=CARTESIAN_POINT('Ctrl Pts',(3.21753275924213,0.183391345602903,19.3190209114062));
#16140=CARTESIAN_POINT('Ctrl Pts',(3.21784912478964,0.177753915601158,19.3186697072606));
#16141=CARTESIAN_POINT('Ctrl Pts',(3.21848164862976,0.165927228029126,19.3179348118808));
#16142=CARTESIAN_POINT('Ctrl Pts',(3.21879477083492,0.159737886394153,19.3175512923402));
#16143=CARTESIAN_POINT('Ctrl Pts',(3.21957949075374,0.143286416133132,19.316534659293));
#16144=CARTESIAN_POINT('Ctrl Pts',(3.22001988250982,0.133022769719706,19.3159032761931));
#16145=CARTESIAN_POINT('Ctrl Pts',(3.22169539694781,0.0890672795835738,
19.3132108993376));
#16146=CARTESIAN_POINT('Ctrl Pts',(3.2224509186319,0.055357896520954,19.3111753121586));
#16147=CARTESIAN_POINT('Ctrl Pts',(3.22272298602462,0.0148435258586338,
19.3087572402425));
#16148=CARTESIAN_POINT('Ctrl Pts',(3.22274712721112,0.00804552500573022,
19.3083524684467));
#16149=CARTESIAN_POINT('Ctrl Pts',(3.22277849800885,-0.0730004198150295,
19.3035377036578));
#16150=CARTESIAN_POINT('Ctrl Pts',(3.22024136583333,-0.147232271517654,
19.2992369287868));
#16151=CARTESIAN_POINT('Ctrl Pts',(3.19469428419743,-0.518366387926518,
19.2779955576693));
#16152=CARTESIAN_POINT('Ctrl Pts',(3.13318255256786,-0.811143990175159,
19.2619329255183));
#16153=CARTESIAN_POINT('Ctrl Pts',(3.00780883092955,-1.15950601489482,19.2402985590405));
#16154=CARTESIAN_POINT('Ctrl Pts',(2.9809803197666,-1.22683466623455,19.236000756736));
#16155=CARTESIAN_POINT('Ctrl Pts',(2.94413189172934,-1.31094637945692,19.2304562542369));
#16156=CARTESIAN_POINT('Ctrl Pts',(2.93619694034723,-1.3286235387898,19.2292810116694));
#16157=CARTESIAN_POINT('Ctrl Pts',(2.92332017341804,-1.35663105958172,19.2274025483642));
#16158=CARTESIAN_POINT('Ctrl Pts',(2.9184817895145,-1.36700867117513,19.2267029038936));
#16159=CARTESIAN_POINT('Ctrl Pts',(2.90933101346451,-1.38636569493844,19.2253909993415));
#16160=CARTESIAN_POINT('Ctrl Pts',(2.90503208207378,-1.39535134807705,19.2247792132542));
#16161=CARTESIAN_POINT('Ctrl Pts',(2.89534851832123,-1.41535326722515,19.2234110764857));
#16162=CARTESIAN_POINT('Ctrl Pts',(2.88994255463398,-1.42635897930154,19.2226539864985));
#16163=CARTESIAN_POINT('Ctrl Pts',(2.87391119076928,-1.45853109063794,19.2204280669516));
#16164=CARTESIAN_POINT('Ctrl Pts',(2.86311529546831,-1.47961117571212,19.2189532647551));
#16165=CARTESIAN_POINT('Ctrl Pts',(2.76478590054308,-1.6665029103353,19.2057290642957));
#16166=CARTESIAN_POINT('Ctrl Pts',(2.66318513963721,-1.82447151263482,19.1934664007828));
#16167=CARTESIAN_POINT('Ctrl Pts',(2.42455401711833,-2.13275030578677,19.167326124335));
#16168=CARTESIAN_POINT('Ctrl Pts',(2.28585811544675,-2.28077572209119,19.1534538480813));
#16169=CARTESIAN_POINT('Ctrl Pts',(2.07290344763074,-2.46898359281224,19.1346206446238));
#16170=CARTESIAN_POINT('Ctrl Pts',(2.00956486801986,-2.52080547366079,19.1292867495923));
#16171=CARTESIAN_POINT('Ctrl Pts',(1.93351400892478,-2.57833757250679,19.1232492555536));
#16172=CARTESIAN_POINT('Ctrl Pts',(1.92265922222932,-2.58644207182011,19.122395913323));
#16173=CARTESIAN_POINT('Ctrl Pts',(1.90612276766789,-2.59862703663872,19.1211089862628));
#16174=CARTESIAN_POINT('Ctrl Pts',(1.90047854601656,-2.6027577258163,19.1206720204612));
#16175=CARTESIAN_POINT('Ctrl Pts',(1.89030933609136,-2.61014928377143,19.1198889082281));
#16176=CARTESIAN_POINT('Ctrl Pts',(1.885789313741,-2.61341679326787,19.1195423058356));
#16177=CARTESIAN_POINT('Ctrl Pts',(1.87592674035221,-2.62050750522005,19.1187892428794));
#16178=CARTESIAN_POINT('Ctrl Pts',(1.87058099143988,-2.62432609947103,19.1183831001334));
#16179=CARTESIAN_POINT('Ctrl Pts',(1.85546872011168,-2.63505151332524,19.1172405603097));
#16180=CARTESIAN_POINT('Ctrl Pts',(1.84567524572291,-2.64192042782369,19.11650672306));
#16181=CARTESIAN_POINT('Ctrl Pts',(1.78541957253379,-2.68368376002771,19.1120303698343));
#16182=CARTESIAN_POINT('Ctrl Pts',(1.73400400122666,-2.71718840584321,19.1083760564091));
#16183=CARTESIAN_POINT('Ctrl Pts',(1.45619144123849,-2.88712326548705,19.0893163305726));
#16184=CARTESIAN_POINT('Ctrl Pts',(1.21459615008605,-2.99679133710031,19.075020832308));
#16185=CARTESIAN_POINT('Ctrl Pts',(0.820498522098549,-3.12009221940006,
19.0515996174903));
#16186=CARTESIAN_POINT('Ctrl Pts',(0.675816620101371,-3.15459298521018,
19.0429970513988));
#16187=CARTESIAN_POINT('Ctrl Pts',(0.507989311013196,-3.18253521482162,
19.0327610077907));
#16188=CARTESIAN_POINT('Ctrl Pts',(0.486661383154679,-3.18586631814296,
19.0314557516721));
#16189=CARTESIAN_POINT('Ctrl Pts',(0.45243582464647,-3.19086014258285,19.0293534063145));
#16190=CARTESIAN_POINT('Ctrl Pts',(0.439558566487385,-3.19265953145594,
19.0285606517345));
#16191=CARTESIAN_POINT('Ctrl Pts',(0.416691597288479,-3.19571385433673,
19.027149656768));
#16192=CARTESIAN_POINT('Ctrl Pts',(0.406706176182196,-3.19700000135308,
19.0265324141123));
#16193=CARTESIAN_POINT('Ctrl Pts',(0.385903552373792,-3.19958039377482,
19.0252441605964));
#16194=CARTESIAN_POINT('Ctrl Pts',(0.37508550066179,-3.20086661866584,19.0245729041152));
#16195=CARTESIAN_POINT('Ctrl Pts',(0.347002890967104,-3.2040612137061,19.0228268618194));
#16196=CARTESIAN_POINT('Ctrl Pts',(0.329729230712132,-3.20588488297499,
19.0217494140295));
#16197=CARTESIAN_POINT('Ctrl Pts',(0.254830727000385,-3.21318057491867,
19.0170620932696));
#16198=CARTESIAN_POINT('Ctrl Pts',(0.197082041550582,-3.21723888991693,
19.0134080413902));
#16199=CARTESIAN_POINT('Ctrl Pts',(0.04328563498193,-3.22389080046199,19.0035638996268));
#16200=CARTESIAN_POINT('Ctrl Pts',(-0.0528163788317471,-3.22374830327729,
18.9972946626481));
#16201=CARTESIAN_POINT('Ctrl Pts',(-0.290174780290116,-3.21278019237065,
18.9815453994762));
#16202=CARTESIAN_POINT('Ctrl Pts',(-0.430996169123826,-3.1969353721517,
18.9719632255826));
#16203=CARTESIAN_POINT('Ctrl Pts',(-0.753288694418371,-3.1389866440437,
18.9497987822883));
#16204=CARTESIAN_POINT('Ctrl Pts',(-0.933099434442101,-3.0903111096826,
18.9372514345219));
#16205=CARTESIAN_POINT('Ctrl Pts',(-1.12150649419319,-3.02135004532682,
18.9245347098674));
#16206=CARTESIAN_POINT('Ctrl Pts',(-1.13525290509136,-3.01621182505879,
18.9236095613343));
#16207=CARTESIAN_POINT('Ctrl Pts',(-1.15562712053581,-3.00843719929124,
18.922242854601));
#16208=CARTESIAN_POINT('Ctrl Pts',(-1.1622818173033,-3.00587248619864,18.9217971732528));
#16209=CARTESIAN_POINT('Ctrl Pts',(-1.17413503282518,-3.00125902039302,
18.9210046857931));
#16210=CARTESIAN_POINT('Ctrl Pts',(-1.17933677590245,-2.99921882386719,
18.9206573749229));
#16211=CARTESIAN_POINT('Ctrl Pts',(-1.1905482801737,-2.99478783657652,18.9199098291231));
#16212=CARTESIAN_POINT('Ctrl Pts',(-1.19655614087605,-2.99239248712474,
18.9195098739371));
#16213=CARTESIAN_POINT('Ctrl Pts',(-1.21322110132825,-2.98568991114394,
18.9184020951802));
#16214=CARTESIAN_POINT('Ctrl Pts',(-1.22386255480651,-2.98134368069958,
18.9176965882952));
#16215=CARTESIAN_POINT('Ctrl Pts',(-1.28385358468796,-2.95646653970393,
18.9137286453667));
#16216=CARTESIAN_POINT('Ctrl Pts',(-1.33271285124997,-2.93476603096161,
18.9105327837608));
#16217=CARTESIAN_POINT('Ctrl Pts',(-1.41269118604885,-2.89683455101536,
18.905325133276));
#16218=CARTESIAN_POINT('Ctrl Pts',(-1.44410934605154,-2.88130057567452,
18.903285620779));
#16219=CARTESIAN_POINT('Ctrl Pts',(-1.47525548819429,-2.86526417753278,
18.9012640026169));
#16220=CARTESIAN_POINT('',(3.22274909203151,0.00241915483385854,19.0621741053498));
#16221=CARTESIAN_POINT('Ctrl Pts',(-1.47525539597219,-2.86526422501572,
18.654425498672));
#16222=CARTESIAN_POINT('Ctrl Pts',(-1.41144708398913,-2.8981175848347,18.6590485555753));
#16223=CARTESIAN_POINT('Ctrl Pts',(-1.34655824498599,-2.92883077286582,
18.6637399058522));
#16224=CARTESIAN_POINT('Ctrl Pts',(-1.05392432190458,-3.05555739076919,
18.6848308599967));
#16225=CARTESIAN_POINT('Ctrl Pts',(-0.816634087221224,-3.12734400873752,
18.7018403219975));
#16226=CARTESIAN_POINT('Ctrl Pts',(-0.486223261711201,-3.18709402826258,
18.7241514003409));
#16227=CARTESIAN_POINT('Ctrl Pts',(-0.398337112113005,-3.19926742450981,
18.7299489907558));
#16228=CARTESIAN_POINT('Ctrl Pts',(-0.296305891333724,-3.2091293402707,
18.7364409869867));
#16229=CARTESIAN_POINT('Ctrl Pts',(-0.282550351901905,-3.2103697012255,
18.7373112136248));
#16230=CARTESIAN_POINT('Ctrl Pts',(-0.26176186273103,-3.21210958524966,
18.7386183845476));
#16231=CARTESIAN_POINT('Ctrl Pts',(-0.254734758486197,-3.21267450350909,
18.7390588689056));
#16232=CARTESIAN_POINT('Ctrl Pts',(-0.242143065127759,-3.21364519295148,
18.7398456273208));
#16233=CARTESIAN_POINT('Ctrl Pts',(-0.23657924651088,-3.21405957502829,
18.7401923776251));
#16234=CARTESIAN_POINT('Ctrl Pts',(-0.224508543681847,-3.21492706278769,
18.740942713798));
#16235=CARTESIAN_POINT('Ctrl Pts',(-0.218001371343994,-3.21537486292088,
18.7413459986431));
#16236=CARTESIAN_POINT('Ctrl Pts',(-0.19976630781111,-3.21657412327742,
18.7424728403003));
#16237=CARTESIAN_POINT('Ctrl Pts',(-0.188035458177054,-3.21728120385095,
18.7431939473967));
#16238=CARTESIAN_POINT('Ctrl Pts',(-0.118703746524175,-3.22107968863735,
18.7474347471748));
#16239=CARTESIAN_POINT('Ctrl Pts',(-0.0610281615454945,-3.22268854529622,
18.750876647311));
#16240=CARTESIAN_POINT('Ctrl Pts',(0.249602492011957,-3.22301013794714,
18.7690998249373));
#16241=CARTESIAN_POINT('Ctrl Pts',(0.501715478025962,-3.19349397726525,
18.7828286133357));
#16242=CARTESIAN_POINT('Ctrl Pts',(0.906658883228421,-3.09689503042297,
18.8063463238252));
#16243=CARTESIAN_POINT('Ctrl Pts',(1.06238520286678,-3.0469848183783,18.8157585454186));
#16244=CARTESIAN_POINT('Ctrl Pts',(1.23397521955806,-2.9772309678316,18.8268989886587));
#16245=CARTESIAN_POINT('Ctrl Pts',(1.25421790558573,-2.96876009255208,18.8282255405014));
#16246=CARTESIAN_POINT('Ctrl Pts',(1.28640856389834,-2.95490140226963,18.8303555028277));
#16247=CARTESIAN_POINT('Ctrl Pts',(1.29841313498423,-2.94964618443391,18.8311543914486));
#16248=CARTESIAN_POINT('Ctrl Pts',(1.31959511261298,-2.94021902675593,18.832572295057));
#16249=CARTESIAN_POINT('Ctrl Pts',(1.32878567448206,-2.93607694281898,18.833190277162));
#16250=CARTESIAN_POINT('Ctrl Pts',(1.33812432300256,-2.93181528966114,18.8338210809947));
#16251=CARTESIAN_POINT('Ctrl Pts',(1.33829207043237,-2.93173872142791,18.8338324128837));
#16252=CARTESIAN_POINT('Ctrl Pts',(1.33865440448754,-2.9315732966456,18.8338568917751));
#16253=CARTESIAN_POINT('Ctrl Pts',(1.33884898883243,-2.9314844351219,18.8338700389496));
#16254=CARTESIAN_POINT('Ctrl Pts',(1.33921163754135,-2.93131877940916,18.8338945438315));
#16255=CARTESIAN_POINT('Ctrl Pts',(1.33937970398714,-2.93124199021328,18.8339059013573));
#16256=CARTESIAN_POINT('Ctrl Pts',(1.339692941405,-2.93109884014989,18.8339270709544));
#16257=CARTESIAN_POINT('Ctrl Pts',(1.33983811505365,-2.93103248249264,18.8339368829661));
#16258=CARTESIAN_POINT('Ctrl Pts',(1.34010869714778,-2.93090877738365,18.8339551724155));
#16259=CARTESIAN_POINT('Ctrl Pts',(1.34023410819899,-2.93085143204747,18.8339636498499));
#16260=CARTESIAN_POINT('Ctrl Pts',(1.34046786643706,-2.93074452584053,18.833979452234));
#16261=CARTESIAN_POINT('Ctrl Pts',(1.34057621625092,-2.93069496623512,18.8339867772273));
#16262=CARTESIAN_POINT('Ctrl Pts',(1.34077818258811,-2.93060257254258,18.8340004319043));
#16263=CARTESIAN_POINT('Ctrl Pts',(1.34087180185896,-2.93055973903892,18.8340067616739));
#16264=CARTESIAN_POINT('Ctrl Pts',(1.3410742718813,-2.93046709145935,18.834020451678));
#16265=CARTESIAN_POINT('Ctrl Pts',(1.34118312428248,-2.93041727471893,18.8340278121276));
#16266=CARTESIAN_POINT('Ctrl Pts',(1.34139727358124,-2.93031925399564,18.8340422933924));
#16267=CARTESIAN_POINT('Ctrl Pts',(1.34150256491635,-2.93027105303097,18.8340494138057));
#16268=CARTESIAN_POINT('Ctrl Pts',(1.34170970930445,-2.93017621159662,18.8340634228487));
#16269=CARTESIAN_POINT('Ctrl Pts',(1.34181156326627,-2.93012957115092,18.834070311516));
#16270=CARTESIAN_POINT('Ctrl Pts',(1.34201195401537,-2.93003779660355,18.8340838651873));
#16271=CARTESIAN_POINT('Ctrl Pts',(1.34211049177097,-2.92999266246921,18.8340905302344));
#16272=CARTESIAN_POINT('Ctrl Pts',(1.34230436658175,-2.92990384841405,18.8341036444773));
#16273=CARTESIAN_POINT('Ctrl Pts',(1.34239970473408,-2.92986016837412,18.8341100937265));
#16274=CARTESIAN_POINT('Ctrl Pts',(1.34258729253158,-2.92977421224376,18.8341227839013));
#16275=CARTESIAN_POINT('Ctrl Pts',(1.34267954334087,-2.92973193597798,18.8341290248862));
#16276=CARTESIAN_POINT('Ctrl Pts',(1.34286106445551,-2.92964873896367,18.8341413057813));
#16277=CARTESIAN_POINT('Ctrl Pts',(1.34295033599251,-2.92960781798504,18.8341473457568));
#16278=CARTESIAN_POINT('Ctrl Pts',(1.34312600243163,-2.92952728492555,18.8341592316067));
#16279=CARTESIAN_POINT('Ctrl Pts',(1.34321239869068,-2.92948767253496,18.8341650775562));
#16280=CARTESIAN_POINT('Ctrl Pts',(1.34338241451021,-2.92940971175856,18.8341765820659));
#16281=CARTESIAN_POINT('Ctrl Pts',(1.34346603554994,-2.92937136298623,18.8341822407105));
#16282=CARTESIAN_POINT('Ctrl Pts',(1.3436305972863,-2.92929588612408,18.8341933770839));
#16283=CARTESIAN_POINT('Ctrl Pts',(1.34371153949483,-2.92925875761347,18.8341988549002));
#16284=CARTESIAN_POINT('Ctrl Pts',(1.34387083601108,-2.92918567968094,18.8342096358293));
#16285=CARTESIAN_POINT('Ctrl Pts',(1.34394919204544,-2.92914972972171,18.8342149390451));
#16286=CARTESIAN_POINT('Ctrl Pts',(1.34410339855715,-2.92907897186964,18.8342253763051));
#16287=CARTESIAN_POINT('Ctrl Pts',(1.3441792508224,-2.92904416339651,18.8342305104569));
#16288=CARTESIAN_POINT('Ctrl Pts',(1.34432856920439,-2.92897563442441,18.8342406176337));
#16289=CARTESIAN_POINT('Ctrl Pts',(1.34440201662103,-2.92894192273188,18.8342455893803));
#16290=CARTESIAN_POINT('Ctrl Pts',(1.34454658297553,-2.92887556151379,18.8342553756139));
#16291=CARTESIAN_POINT('Ctrl Pts',(1.34461770197756,-2.92884291216728,18.8342601900938));
#16292=CARTESIAN_POINT('Ctrl Pts',(1.34475769107534,-2.92877863972968,18.834269667147));
#16293=CARTESIAN_POINT('Ctrl Pts',(1.34482656124352,-2.92874701680036,18.8342743297146));
#16294=CARTESIAN_POINT('Ctrl Pts',(1.34496212922607,-2.92868476262546,18.8342835080944));
#16295=CARTESIAN_POINT('Ctrl Pts',(1.34502882713768,-2.92865413151767,18.8342880239033));
#16296=CARTESIAN_POINT('Ctrl Pts',(1.3555316014687,-2.92383028347042,18.8349991420772));
#16297=CARTESIAN_POINT('Ctrl Pts',(1.36594187343311,-2.91898137062315,18.8357076702584));
#16298=CARTESIAN_POINT('Ctrl Pts',(1.39472831273764,-2.90538546276715,18.8376772155866));
#16299=CARTESIAN_POINT('Ctrl Pts',(1.41304763236518,-2.89652000020959,18.8389423402925));
#16300=CARTESIAN_POINT('Ctrl Pts',(1.45372256568881,-2.87635804568532,18.8417780579109));
#16301=CARTESIAN_POINT('Ctrl Pts',(1.47603273893388,-2.864973333465,18.8433516816669));
#16302=CARTESIAN_POINT('Ctrl Pts',(1.54471926499953,-2.82890787114527,18.8482539967374));
#16303=CARTESIAN_POINT('Ctrl Pts',(1.5906246673697,-2.8033533505077,18.8516128199475));
#16304=CARTESIAN_POINT('Ctrl Pts',(1.76993406431116,-2.69771345288985,18.8650655338483));
#16305=CARTESIAN_POINT('Ctrl Pts',(1.89807506545773,-2.60914267118674,18.8754406178092));
#16306=CARTESIAN_POINT('Ctrl Pts',(2.19757436559864,-2.36835486473635,18.9013832556073));
#16307=CARTESIAN_POINT('Ctrl Pts',(2.36008820460303,-2.20645334753572,18.9170503024327));
#16308=CARTESIAN_POINT('Ctrl Pts',(2.51910484713755,-2.01017331778175,18.9332152231008));
#16309=CARTESIAN_POINT('Ctrl Pts',(2.53390764186923,-1.99148139324945,18.9347287371475));
#16310=CARTESIAN_POINT('Ctrl Pts',(2.55398018834381,-1.9655489963369,18.9367912321941));
#16311=CARTESIAN_POINT('Ctrl Pts',(2.55942881391245,-1.95844882764018,18.9373521463012));
#16312=CARTESIAN_POINT('Ctrl Pts',(2.56806622478967,-1.94709570397389,18.9382429020261));
#16313=CARTESIAN_POINT('Ctrl Pts',(2.57127413946588,-1.94285746158336,18.9385740757507));
#16314=CARTESIAN_POINT('Ctrl Pts',(2.57790233280137,-1.93405523512263,18.9392590387867));
#16315=CARTESIAN_POINT('Ctrl Pts',(2.58132098781501,-1.92949010059257,18.9396127059518));
#16316=CARTESIAN_POINT('Ctrl Pts',(2.58948315772167,-1.91853014885856,18.9404580723942));
#16317=CARTESIAN_POINT('Ctrl Pts',(2.5942151680183,-1.91212672733993,18.9409489683024));
#16318=CARTESIAN_POINT('Ctrl Pts',(2.61030816014087,-1.89017976378948,18.9426214271854));
#16319=CARTESIAN_POINT('Ctrl Pts',(2.62155382595271,-1.87455162896909,18.9437952552479));
#16320=CARTESIAN_POINT('Ctrl Pts',(2.68468333444436,-1.78514104273174,18.9504200944338));
#16321=CARTESIAN_POINT('Ctrl Pts',(2.73359640057202,-1.70930012724519,18.9556916366246));
#16322=CARTESIAN_POINT('Ctrl Pts',(2.90189607001275,-1.42260096633018,18.9747551100313));
#16323=CARTESIAN_POINT('Ctrl Pts',(3.00058569078484,-1.20053787915899,18.9879287755434));
#16324=CARTESIAN_POINT('Ctrl Pts',(3.09252404420871,-0.909080226280977,
19.0053563879611));
#16325=CARTESIAN_POINT('Ctrl Pts',(3.10979736006618,-0.848110596943444,
19.009005038856));
#16326=CARTESIAN_POINT('Ctrl Pts',(3.14340939593379,-0.714578214367164,
19.0170438762466));
#16327=CARTESIAN_POINT('Ctrl Pts',(3.15905556683538,-0.641881058450411,
19.0214506154029));
#16328=CARTESIAN_POINT('Ctrl Pts',(3.17562244515314,-0.549473968270774,
19.0271181295656));
#16329=CARTESIAN_POINT('Ctrl Pts',(3.1788963119542,-0.530205401495658,19.0283034490697));
#16330=CARTESIAN_POINT('Ctrl Pts',(3.18381564484577,-0.499567256271762,
19.0301942563104));
#16331=CARTESIAN_POINT('Ctrl Pts',(3.18557596675757,-0.488216405429767,
19.0308960844592));
#16332=CARTESIAN_POINT('Ctrl Pts',(3.18860115029231,-0.467996289951824,
19.0321487444159));
#16333=CARTESIAN_POINT('Ctrl Pts',(3.18988978738244,-0.459130662040544,
19.0326988140614));
#16334=CARTESIAN_POINT('Ctrl Pts',(3.19246118852457,-0.440906286102035,
19.0338313070568));
#16335=CARTESIAN_POINT('Ctrl Pts',(3.19373980388004,-0.431547048913755,
19.0344138564375));
#16336=CARTESIAN_POINT('Ctrl Pts',(3.19648766264385,-0.410751899432377,
19.035710377853));
#16337=CARTESIAN_POINT('Ctrl Pts',(3.19793671442684,-0.399313492478713,
19.0364249826057));
#16338=CARTESIAN_POINT('Ctrl Pts',(3.20138806936181,-0.370845010632214,
19.0382072294497));
#16339=CARTESIAN_POINT('Ctrl Pts',(3.20331587446157,-0.353806419702777,
19.0392772088441));
#16340=CARTESIAN_POINT('Ctrl Pts',(3.21694690436431,-0.224070826567322,
19.0474500812389));
#16341=CARTESIAN_POINT('Ctrl Pts',(3.2228341227182,-0.110857004473895,19.0547344658747));
#16342=CARTESIAN_POINT('Ctrl Pts',(3.22274909203151,0.00241915483385854,
19.0621741053498));
#16343=CARTESIAN_POINT('Ctrl Pts',(3.22274909510165,0.00241506138934033,
19.0621738365046));
#16344=CARTESIAN_POINT('Ctrl Pts',(3.22257571361233,0.233781866502874,19.0773693093119));
#16345=CARTESIAN_POINT('Ctrl Pts',(3.19748646516631,0.464455112312948,19.0932022669885));
#16346=CARTESIAN_POINT('Ctrl Pts',(3.12345943544361,0.801971971738992,19.1164103917512));
#16347=CARTESIAN_POINT('Ctrl Pts',(3.09308090398364,0.912147907119489,19.1239794830628));
#16348=CARTESIAN_POINT('Ctrl Pts',(3.05002227525443,1.04113175163933,19.1326611875246));
#16349=CARTESIAN_POINT('Ctrl Pts',(3.04292174037639,1.06170548949412,19.1340403176688));
#16350=CARTESIAN_POINT('Ctrl Pts',(3.03280502634267,1.09008309910926,19.1359331767385));
#16351=CARTESIAN_POINT('Ctrl Pts',(3.02996625960551,1.09794897883596,19.1364568455494));
#16352=CARTESIAN_POINT('Ctrl Pts',(3.02511371521723,1.11123263876078,19.1373393908265));
#16353=CARTESIAN_POINT('Ctrl Pts',(3.02311593428994,1.11665617671798,19.1376992097038));
#16354=CARTESIAN_POINT('Ctrl Pts',(3.01928372423851,1.12697412315389,19.1383827268384));
#16355=CARTESIAN_POINT('Ctrl Pts',(3.01745196880854,1.1318694706423,19.1387065867933));
#16356=CARTESIAN_POINT('Ctrl Pts',(3.01261503131926,1.14470094247849,19.1395543871147));
#16357=CARTESIAN_POINT('Ctrl Pts',(3.00959037505906,1.15262975530922,19.14007716581));
#16358=CARTESIAN_POINT('Ctrl Pts',(2.99898192020575,1.18011222217206,19.1418857002611));
#16359=CARTESIAN_POINT('Ctrl Pts',(2.99123840527567,1.19960421419486,19.1431622471303));
#16360=CARTESIAN_POINT('Ctrl Pts',(2.88715549902908,1.45432611834879,19.1597805028388));
#16361=CARTESIAN_POINT('Ctrl Pts',(2.76348893439609,1.677468820385,19.1736720097659));
#16362=CARTESIAN_POINT('Ctrl Pts',(2.54248959412162,1.98423612103214,19.1948604344727));
#16363=CARTESIAN_POINT('Ctrl Pts',(2.46439515289904,2.08043257470821,19.2018560436664));
#16364=CARTESIAN_POINT('Ctrl Pts',(2.34155844371033,2.21509385933022,19.2124327210213));
#16365=CARTESIAN_POINT('Ctrl Pts',(2.30098485551773,2.25721174392057,19.2158647779638));
#16366=CARTESIAN_POINT('Ctrl Pts',(2.24000443729592,2.31715969222176,19.2209535899304));
#16367=CARTESIAN_POINT('Ctrl Pts',(2.22048174427643,2.33587449917993,19.2225728256336));
#16368=CARTESIAN_POINT('Ctrl Pts',(2.18494913950105,2.36908869248058,19.2255040093059));
#16369=CARTESIAN_POINT('Ctrl Pts',(2.16902447605159,2.38367715145035,19.2268120926198));
#16370=CARTESIAN_POINT('Ctrl Pts',(2.14418234442706,2.40597976196341,19.2288447498348));
#16371=CARTESIAN_POINT('Ctrl Pts',(2.13536695048044,2.41380705983496,19.2295645366471));
#16372=CARTESIAN_POINT('Ctrl Pts',(2.12642692555814,2.42165771831261,19.2302930365842));
#16373=CARTESIAN_POINT('Ctrl Pts',(2.12634494758734,2.4217296996716,19.2302997166374));
#16374=CARTESIAN_POINT('Ctrl Pts',(2.12617967318954,2.42187480520795,19.2303131839302));
#16375=CARTESIAN_POINT('Ctrl Pts',(2.12609637664471,2.42194792925109,19.2303199711756));
#16376=CARTESIAN_POINT('Ctrl Pts',(2.12592842233624,2.42209535697728,19.2303336563253));
#16377=CARTESIAN_POINT('Ctrl Pts',(2.12584376443013,2.42216966053609,19.2303405542372));
#16378=CARTESIAN_POINT('Ctrl Pts',(2.12567304284607,2.42231948564346,19.2303544643375));
#16379=CARTESIAN_POINT('Ctrl Pts',(2.12558697905882,2.42239500702632,19.2303614765305));
#16380=CARTESIAN_POINT('Ctrl Pts',(2.12541339949649,2.42254730754527,19.2303756189457));
#16381=CARTESIAN_POINT('Ctrl Pts',(2.12532588357581,2.42262408653442,19.230382749175));
#16382=CARTESIAN_POINT('Ctrl Pts',(2.12514935159806,2.42277894367654,19.2303971315718));
#16383=CARTESIAN_POINT('Ctrl Pts',(2.12506033540586,2.4228570216595,19.2304043837455));
#16384=CARTESIAN_POINT('Ctrl Pts',(2.12491014938738,2.42298873834555,19.2304166191967));
#16385=CARTESIAN_POINT('Ctrl Pts',(2.12484898181302,2.42304237965559,19.2304216023674));
#16386=CARTESIAN_POINT('Ctrl Pts',(2.12472164845756,2.4231540369567,19.2304319757578));
#16387=CARTESIAN_POINT('Ctrl Pts',(2.12465548235526,2.42321205253306,19.230437365992));
#16388=CARTESIAN_POINT('Ctrl Pts',(2.12451769323387,2.42333285842221,19.2304485908422));
#16389=CARTESIAN_POINT('Ctrl Pts',(2.12444606980804,2.42339564826911,19.2304544254776));
#16390=CARTESIAN_POINT('Ctrl Pts',(2.12429685715508,2.42352644628159,19.2304665805429));
#16391=CARTESIAN_POINT('Ctrl Pts',(2.12421926744352,2.42359445389836,19.2304729009961));
#16392=CARTESIAN_POINT('Ctrl Pts',(2.12405755639071,2.4237361803939,19.2304860737391));
#16393=CARTESIAN_POINT('Ctrl Pts',(2.12397343448553,2.42380989861222,19.2304929260556));
#16394=CARTESIAN_POINT('Ctrl Pts',(2.12379802851159,2.42396359529586,19.2305072138272));
#16395=CARTESIAN_POINT('Ctrl Pts',(2.12370674374051,2.42404357300368,19.2305146493166));
#16396=CARTESIAN_POINT('Ctrl Pts',(2.12351630738218,2.42421040179192,19.2305301607597));
#16397=CARTESIAN_POINT('Ctrl Pts',(2.12341715501037,2.42429725192308,19.2305382367501));
#16398=CARTESIAN_POINT('Ctrl Pts',(2.12321019414125,2.42447851187231,19.2305550934004));
#16399=CARTESIAN_POINT('Ctrl Pts',(2.12310238466953,2.42457292058755,19.230563874107));
#16400=CARTESIAN_POINT('Ctrl Pts',(2.12287722273016,2.42477006828284,19.2305822123214));
#16401=CARTESIAN_POINT('Ctrl Pts',(2.12275986911201,2.42487280592497,19.2305917698838));
#16402=CARTESIAN_POINT('Ctrl Pts',(2.12251461956958,2.42508747906139,19.2306117430751));
#16403=CARTESIAN_POINT('Ctrl Pts',(2.12238672223894,2.42519941296603,19.2306221587716));
#16404=CARTESIAN_POINT('Ctrl Pts',(2.12211925381301,2.42543346012375,19.2306439402293));
#16405=CARTESIAN_POINT('Ctrl Pts',(2.12197968102787,2.42555557144983,19.2306553060716));
#16406=CARTESIAN_POINT('Ctrl Pts',(2.12168759008914,2.42581107541734,19.230679091196));
#16407=CARTESIAN_POINT('Ctrl Pts',(2.12153506450358,2.42594447043604,19.2306915110146));
#16408=CARTESIAN_POINT('Ctrl Pts',(2.12121560090079,2.42622381205055,19.2307175233392));
#16409=CARTESIAN_POINT('Ctrl Pts',(2.12104866203641,2.42636975437433,19.2307311158305));
#16410=CARTESIAN_POINT('Ctrl Pts',(2.12075350799421,2.42662773202234,19.2307551469606));
#16411=CARTESIAN_POINT('Ctrl Pts',(2.12062530156263,2.42673977217675,19.2307655850946));
#16412=CARTESIAN_POINT('Ctrl Pts',(2.1202954851253,2.42702795408887,19.2307924368673));
#16413=CARTESIAN_POINT('Ctrl Pts',(2.12009386477938,2.42720407850242,19.2308088509091));
#16414=CARTESIAN_POINT('Ctrl Pts',(2.11957162365641,2.42766016482273,19.230851364989));
#16415=CARTESIAN_POINT('Ctrl Pts',(2.11925097118889,2.4279400867375,19.2308774664831));
#16416=CARTESIAN_POINT('Ctrl Pts',(2.11133468747185,2.43484804958631,19.2315218156038));
#16417=CARTESIAN_POINT('Ctrl Pts',(2.10370812179963,2.44144041944195,19.2321415419821));
#16418=CARTESIAN_POINT('Ctrl Pts',(2.08609652225864,2.45652001720474,19.2335703292408));
#16419=CARTESIAN_POINT('Ctrl Pts',(2.07609045106348,2.46498229729061,19.2343804063808));
#16420=CARTESIAN_POINT('Ctrl Pts',(2.04919159886154,2.48745108432295,19.2365537609265));
#16421=CARTESIAN_POINT('Ctrl Pts',(2.03220713606083,2.50134628218794,19.2379215386953));
#16422=CARTESIAN_POINT('Ctrl Pts',(1.88738910441523,2.61737512304025,19.2495479094667));
#16423=CARTESIAN_POINT('Ctrl Pts',(1.75211009938113,2.70979440964908,19.2601925364903));
#16424=CARTESIAN_POINT('Ctrl Pts',(1.39079336838108,2.91823572082224,19.2880124635982));
#16425=CARTESIAN_POINT('Ctrl Pts',(1.15699553393417,3.01856958470996,19.3055130634214));
#16426=CARTESIAN_POINT('Ctrl Pts',(0.859310904607945,3.10659592343055,19.3258274673674));
#16427=CARTESIAN_POINT('Ctrl Pts',(0.804339278287263,3.12128062342996,19.329496753474));
#16428=CARTESIAN_POINT('Ctrl Pts',(0.737619803548651,3.13722354726431,19.3338288298399));
#16429=CARTESIAN_POINT('Ctrl Pts',(0.72622076435119,3.139881840363,19.334564729004));
#16430=CARTESIAN_POINT('Ctrl Pts',(0.708457302187487,3.14392242622939,19.335704644825));
#16431=CARTESIAN_POINT('Ctrl Pts',(0.702102883003066,3.1453475983794,19.3361110580181));
#16432=CARTESIAN_POINT('Ctrl Pts',(0.690295429859775,3.14795821470906,19.3368636499795));
#16433=CARTESIAN_POINT('Ctrl Pts',(0.684843688567357,3.1491487460892,19.3372101095524));
#16434=CARTESIAN_POINT('Ctrl Pts',(0.672483946041851,3.15181420747561,19.337993270266));
#16435=CARTESIAN_POINT('Ctrl Pts',(0.665574188270009,3.1532805866719,19.3384294772263));
#16436=CARTESIAN_POINT('Ctrl Pts',(0.645076709243011,3.15756015597896,19.3397188111984));
#16437=CARTESIAN_POINT('Ctrl Pts',(0.631475373786384,3.16030836593499,19.3405683095803));
#16438=CARTESIAN_POINT('Ctrl Pts',(0.52903137793221,3.18031984489479,19.3469240674594));
#16439=CARTESIAN_POINT('Ctrl Pts',(0.439505752586364,3.19392336490035,19.3522381804442));
#16440=CARTESIAN_POINT('Ctrl Pts',(0.106249106673691,3.23028059638407,19.3715259399356));
#16441=CARTESIAN_POINT('Ctrl Pts',(-0.139258832592949,3.22902807506504,
19.3848234414536));
#16442=CARTESIAN_POINT('Ctrl Pts',(-0.473337921352233,3.18911904278954,
19.4039799646665));
#16443=CARTESIAN_POINT('Ctrl Pts',(-0.563892696915195,3.17435854375601,
19.4092742090918));
#16444=CARTESIAN_POINT('Ctrl Pts',(-0.708528007674001,3.14439848719691,
19.417984395934));
#16445=CARTESIAN_POINT('Ctrl Pts',(-0.763057725260847,3.13161238315833,
19.4213272160721));
#16446=CARTESIAN_POINT('Ctrl Pts',(-0.833825371675357,3.11306076831362,
19.4257543261987));
#16447=CARTESIAN_POINT('Ctrl Pts',(-0.850391164562575,3.10857635376277,
19.4267970655948));
#16448=CARTESIAN_POINT('Ctrl Pts',(-0.877366355964989,3.10104232096191,
19.4285058278988));
#16449=CARTESIAN_POINT('Ctrl Pts',(-0.887797710056435,3.09807204894377,
19.4291692578335));
#16450=CARTESIAN_POINT('Ctrl Pts',(-0.907894141976137,3.09223986640998,
19.4304525836808));
#16451=CARTESIAN_POINT('Ctrl Pts',(-0.917561189606142,3.08938515308372,
19.4310722374624));
#16452=CARTESIAN_POINT('Ctrl Pts',(-0.939758340571584,3.08271688113162,
19.432500506646));
#16453=CARTESIAN_POINT('Ctrl Pts',(-0.952278841997937,3.07887221346227,
19.433310135907));
#16454=CARTESIAN_POINT('Ctrl Pts',(-0.985689749266093,3.06838943896977,
19.4354815077615));
#16455=CARTESIAN_POINT('Ctrl Pts',(-1.00653616406198,3.0616144340987,19.4368477378353));
#16456=CARTESIAN_POINT('Ctrl Pts',(-1.18263861392223,3.00238886084082,19.4484881738583));
#16457=CARTESIAN_POINT('Ctrl Pts',(-1.33373061961618,2.93838746724878,19.4591496921086));
#16458=CARTESIAN_POINT('Ctrl Pts',(-1.70491113282351,2.74661474782247,19.4870153917478));
#16459=CARTESIAN_POINT('Ctrl Pts',(-1.915957641142,2.60378878879702,19.5045455434699));
#16460=CARTESIAN_POINT('Ctrl Pts',(-2.15065158148517,2.40083068483367,19.5248439959419));
#16461=CARTESIAN_POINT('Ctrl Pts',(-2.1922864089605,2.36287355148469,19.5284763657729));
#16462=CARTESIAN_POINT('Ctrl Pts',(-2.2413233330016,2.31575549072658,19.5327708339352));
#16463=CARTESIAN_POINT('Ctrl Pts',(-2.24969518935308,2.30762330997188,19.5335045990551));
#16464=CARTESIAN_POINT('Ctrl Pts',(-2.26266409403743,2.29488803072314,19.5346419342408));
#16465=CARTESIAN_POINT('Ctrl Pts',(-2.26729159466737,2.29031628875332,19.5350478837161));
#16466=CARTESIAN_POINT('Ctrl Pts',(-2.27586361075188,2.28179612054045,19.5358000558898));
#16467=CARTESIAN_POINT('Ctrl Pts',(-2.27981167394376,2.27785149703018,19.5361465566314));
#16468=CARTESIAN_POINT('Ctrl Pts',(-2.28874047043527,2.26888401115437,19.5369303688514));
#16469=CARTESIAN_POINT('Ctrl Pts',(-2.2937149142901,2.26385500668586,19.5373671826831));
#16470=CARTESIAN_POINT('Ctrl Pts',(-2.30843101844807,2.24887919444394,19.5386599761996));
#16471=CARTESIAN_POINT('Ctrl Pts',(-2.31812497260019,2.23888544275162,19.5395122982776));
#16472=CARTESIAN_POINT('Ctrl Pts',(-2.39129210720271,2.16247083377905,19.5459538318366));
#16473=CARTESIAN_POINT('Ctrl Pts',(-2.45197011327385,2.09341921234325,19.5513449833047));
#16474=CARTESIAN_POINT('Ctrl Pts',(-2.66205968332149,1.83264728213634,19.5705991427137));
#16475=CARTESIAN_POINT('Ctrl Pts',(-2.79261739876554,1.62679408855662,19.5838080707924));
#16476=CARTESIAN_POINT('Ctrl Pts',(-2.93895816844397,1.3255518241652,19.6028748324302));
#16477=CARTESIAN_POINT('Ctrl Pts',(-2.97555715281676,1.24121732841146,19.6081792234531));
#16478=CARTESIAN_POINT('Ctrl Pts',(-3.02860796877706,1.10308500903541,19.616904578623));
#16479=CARTESIAN_POINT('Ctrl Pts',(-3.04734384197765,1.0502179290835,19.6202520865171));
#16480=CARTESIAN_POINT('Ctrl Pts',(-3.07000154359415,0.980562554144265,
19.6246845406797));
#16481=CARTESIAN_POINT('Ctrl Pts',(-3.0751823230422,0.964191922056175,19.6257278088227));
#16482=CARTESIAN_POINT('Ctrl Pts',(-3.08342224532108,0.937412661608031,
19.6274372198243));
#16483=CARTESIAN_POINT('Ctrl Pts',(-3.08656013262519,0.927028470017138,
19.6281007659076));
#16484=CARTESIAN_POINT('Ctrl Pts',(-3.09251223786166,0.906965935963204,
19.6293841634253));
#16485=CARTESIAN_POINT('Ctrl Pts',(-3.09533360127239,0.897289832480227,
19.630003771906));
#16486=CARTESIAN_POINT('Ctrl Pts',(-3.1017155579208,0.875014050540049,19.6314317172765));
#16487=CARTESIAN_POINT('Ctrl Pts',(-3.10524483249448,0.862405654564231,
19.6322410665247));
#16488=CARTESIAN_POINT('Ctrl Pts',(-3.11447286694119,0.828647163133197,
19.6344111991212));
#16489=CARTESIAN_POINT('Ctrl Pts',(-3.1200329143053,0.807460175655846,19.6357764619065));
#16490=CARTESIAN_POINT('Ctrl Pts',(-3.16536230969041,0.627266740960554,
19.6474175383769));
#16491=CARTESIAN_POINT('Ctrl Pts',(-3.19315789070699,0.465521324437458,
19.6580808194204));
#16492=CARTESIAN_POINT('Ctrl Pts',(-3.23236142276593,0.0495422632228797,
19.685948416339));
#16493=CARTESIAN_POINT('Ctrl Pts',(-3.22622005801688,-0.205217290080257,
19.7034786047808));
#16494=CARTESIAN_POINT('Ctrl Pts',(-3.18225876866391,-0.512366327591324,
19.7237770376986));
#16495=CARTESIAN_POINT('Ctrl Pts',(-3.17281742835111,-0.567908978396284,
19.7274093619145));
#16496=CARTESIAN_POINT('Ctrl Pts',(-3.15966744969356,-0.634630114524239,
19.7317037835819));
#16497=CARTESIAN_POINT('Ctrl Pts',(-3.15734841410374,-0.646068708967421,
19.7324375460487));
#16498=CARTESIAN_POINT('Ctrl Pts',(-3.15364014572805,-0.663862717085865,
19.7335748780255));
#16499=CARTESIAN_POINT('Ctrl Pts',(-3.15229375207197,-0.670226811092926,
19.7339808269241));
#16500=CARTESIAN_POINT('Ctrl Pts',(-3.14975639720097,-0.682043509433465,
19.7347329985767));
#16501=CARTESIAN_POINT('Ctrl Pts',(-3.14857055271795,-0.687497044168862,
19.7350794993705));
#16502=CARTESIAN_POINT('Ctrl Pts',(-3.14584958693042,-0.699855680598632,
19.7358633124055));
#16503=CARTESIAN_POINT('Ctrl Pts',(-3.14430589884105,-0.706758808946262,
19.7363001269957));
#16504=CARTESIAN_POINT('Ctrl Pts',(-3.13965642136871,-0.727233769513876,
19.7375929248387));
#16505=CARTESIAN_POINT('Ctrl Pts',(-3.13648535284086,-0.740790825672001,
19.7384452504484));
#16506=CARTESIAN_POINT('Ctrl Pts',(-3.11172217067486,-0.843648920727268,
19.7448868931244));
#16507=CARTESIAN_POINT('Ctrl Pts',(-3.08640591243335,-0.932019473435434,
19.7502781425933));
#16508=CARTESIAN_POINT('Ctrl Pts',(-2.9805025239281,-1.24970455136136,19.7695322608739));
#16509=CARTESIAN_POINT('Ctrl Pts',(-2.87783637579601,-1.47079151425014,
19.7827410774952));
#16510=CARTESIAN_POINT('Ctrl Pts',(-2.70343455100568,-1.75670271328719,
19.8018077256279));
#16511=CARTESIAN_POINT('Ctrl Pts',(-2.65224805277895,-1.83306877464473,
19.8071121286915));
#16512=CARTESIAN_POINT('Ctrl Pts',(-2.56468345938699,-1.95234769687855,
19.8158375018593));
#16513=CARTESIAN_POINT('Ctrl Pts',(-2.53032271894615,-1.99667952822963,
19.8191850153139));
#16514=CARTESIAN_POINT('Ctrl Pts',(-2.48395474598055,-2.05338287236936,
19.8236174758151));
#16515=CARTESIAN_POINT('Ctrl Pts',(-2.4729792275753,-2.06658803897859,19.8246607445848));
#16516=CARTESIAN_POINT('Ctrl Pts',(-2.4548984534088,-2.08799157675144,19.8263701563554));
#16517=CARTESIAN_POINT('Ctrl Pts',(-2.44785630927522,-2.09624300254644,
19.8270337025763));
#16518=CARTESIAN_POINT('Ctrl Pts',(-2.43419105997023,-2.11209209881246,
19.8283171001792));
#16519=CARTESIAN_POINT('Ctrl Pts',(-2.42757369983697,-2.11969457197999,
19.8289367086063));
#16520=CARTESIAN_POINT('Ctrl Pts',(-2.41227840547815,-2.13710128099154,
19.8303646535934));
#16521=CARTESIAN_POINT('Ctrl Pts',(-2.40357621304076,-2.14688387453169,
19.8311740025101));
#16522=CARTESIAN_POINT('Ctrl Pts',(-2.38015677030373,-2.17289003584273,
19.8333441336393));
#16523=CARTESIAN_POINT('Ctrl Pts',(-2.36533352474845,-2.18901681983613,
19.8347093952794));
#16524=CARTESIAN_POINT('Ctrl Pts',(-2.23820550853008,-2.32452531060372,
19.8463504135067));
#16525=CARTESIAN_POINT('Ctrl Pts',(-2.11712615437145,-2.43531188296846,
19.8570136329685));
#16526=CARTESIAN_POINT('Ctrl Pts',(-1.82787122541351,-2.66204535638539,
19.8815266994009));
#16527=CARTESIAN_POINT('Ctrl Pts',(-1.65612355608179,-2.77213957406373,
19.8954708340483));
#16528=CARTESIAN_POINT('Ctrl Pts',(-1.47525540330811,-2.86526422123863,
19.9090518554891));
#16529=CARTESIAN_POINT('Origin',(0.,0.,4.68922655072688));
#16530=CARTESIAN_POINT('',(-1.47286814312172,-2.86060451358776,21.4037167033623));
#16531=CARTESIAN_POINT('',(-1.47525512068018,-2.86526436675691,21.1585511949183));
#16532=CARTESIAN_POINT('',(-1.47525540501186,-2.86526422036142,4.68922655072688));
#16533=CARTESIAN_POINT('',(3.22288743813532,-0.00297411405783051,20.5607735307834));
#16534=CARTESIAN_POINT('Ctrl Pts',(3.22288743813532,-0.00297411405783051,
20.5607735307834));
#16535=CARTESIAN_POINT('Ctrl Pts',(3.21520567054372,0.825027405902577,20.6119075522263));
#16536=CARTESIAN_POINT('Ctrl Pts',(2.46751291112442,2.73910351537692,20.7293525531237));
#16537=CARTESIAN_POINT('Ctrl Pts',(-0.758236137317192,3.73602587213299,
20.9131085334756));
#16538=CARTESIAN_POINT('Ctrl Pts',(-3.55335956546679,1.38074152385103,21.112041471839));
#16539=CARTESIAN_POINT('Ctrl Pts',(-3.16575851074329,-1.59892501153937,
21.275577528468));
#16540=CARTESIAN_POINT('Ctrl Pts',(-1.92022651981776,-2.63131100466499,
21.3728026056424));
#16541=CARTESIAN_POINT('Ctrl Pts',(-1.47286814312172,-2.86060451358776,
21.4037167033623));
#16542=CARTESIAN_POINT('Ctrl Pts',(3.22274863154765,-0.00296990870983751,
20.5606936678279));
#16543=CARTESIAN_POINT('Ctrl Pts',(3.22255702526824,-0.210888378631545,
20.5466283729016));
#16544=CARTESIAN_POINT('Ctrl Pts',(3.20224496926727,-0.418325185966235,
20.5324657971094));
#16545=CARTESIAN_POINT('Ctrl Pts',(3.15908206884142,-0.637620041575319,
20.518181388141));
#16546=CARTESIAN_POINT('Ctrl Pts',(3.1559721229632,-0.652839042730332,20.5171938674373));
#16547=CARTESIAN_POINT('Ctrl Pts',(3.15091550430859,-0.676703448685813,
20.5156519965644));
#16548=CARTESIAN_POINT('Ctrl Pts',(3.14904304839768,-0.685364104943512,
20.5150938098942));
#16549=CARTESIAN_POINT('Ctrl Pts',(3.1454329574484,-0.701734658377767,20.5140414607767));
#16550=CARTESIAN_POINT('Ctrl Pts',(3.14370263853446,-0.70944608264459,20.5135469029785));
#16551=CARTESIAN_POINT('Ctrl Pts',(3.14067682238565,-0.722702625013594,
20.5126988029036));
#16552=CARTESIAN_POINT('Ctrl Pts',(3.13939496920804,-0.72825079208872,20.5123444837374));
#16553=CARTESIAN_POINT('Ctrl Pts',(3.13688399774121,-0.738989034692541,
20.5116599683094));
#16554=CARTESIAN_POINT('Ctrl Pts',(3.13565670042801,-0.744179458682553,
20.5113296656626));
#16555=CARTESIAN_POINT('Ctrl Pts',(3.13231537774037,-0.758155386377132,
20.5104417418585));
#16556=CARTESIAN_POINT('Ctrl Pts',(3.13017725927639,-0.76693516390364,20.5098854995544));
#16557=CARTESIAN_POINT('Ctrl Pts',(3.12212946917851,-0.799387544907498,
20.5078348572979));
#16558=CARTESIAN_POINT('Ctrl Pts',(3.11598777851726,-0.823002500528097,
20.5063532493039));
#16559=CARTESIAN_POINT('Ctrl Pts',(3.06178724070192,-1.02209477404303,20.4939344040308));
#16560=CARTESIAN_POINT('Ctrl Pts',(2.99920953173441,-1.19330578281535,20.4837203162587));
#16561=CARTESIAN_POINT('Ctrl Pts',(2.87583190712063,-1.4587566095342,20.4673516209356));
#16562=CARTESIAN_POINT('Ctrl Pts',(2.82401428160712,-1.55670251602427,20.4611867627293));
#16563=CARTESIAN_POINT('Ctrl Pts',(2.69206053692797,-1.77776652101174,20.4466380028718));
#16564=CARTESIAN_POINT('Ctrl Pts',(2.60835517109728,-1.89845190222038,20.4381960080741));
#16565=CARTESIAN_POINT('Ctrl Pts',(2.49540547378774,-2.03966524559805,20.4273968919483));
#16566=CARTESIAN_POINT('Ctrl Pts',(2.47366209540388,-2.0659812427616,20.4253423585494));
#16567=CARTESIAN_POINT('Ctrl Pts',(2.44430161146891,-2.10038814427956,20.4225973701187));
#16568=CARTESIAN_POINT('Ctrl Pts',(2.4370543160944,-2.10879277788329,20.4219220975046));
#16569=CARTESIAN_POINT('Ctrl Pts',(2.422633370982,-2.12534301273849,20.4205828268747));
#16570=CARTESIAN_POINT('Ctrl Pts',(2.4154616919937,-2.13349014104704,20.4199189156074));
#16571=CARTESIAN_POINT('Ctrl Pts',(2.40154942518816,-2.14913460820212,20.4186349848711));
#16572=CARTESIAN_POINT('Ctrl Pts',(2.39481453444172,-2.15663686042271,20.4180152094677));
#16573=CARTESIAN_POINT('Ctrl Pts',(2.37925279366811,-2.17380889753686,20.4165871262543));
#16574=CARTESIAN_POINT('Ctrl Pts',(2.37040204296757,-2.18345669197984,20.4157778070735));
#16575=CARTESIAN_POINT('Ctrl Pts',(2.3465936800498,-2.2090937154951,20.4136082990189));
#16576=CARTESIAN_POINT('Ctrl Pts',(2.33153170497183,-2.22498467715795,20.412243636602));
#16577=CARTESIAN_POINT('Ctrl Pts',(2.20285382459719,-2.35800338760957,20.4006486714134));
#16578=CARTESIAN_POINT('Ctrl Pts',(2.08067272930059,-2.46648158922455,20.390034475905));
#16579=CARTESIAN_POINT('Ctrl Pts',(1.81292074882527,-2.67010310770066,20.3676030363587));
#16580=CARTESIAN_POINT('Ctrl Pts',(1.66679074097349,-2.76368164665189,20.355786790884));
#16581=CARTESIAN_POINT('Ctrl Pts',(1.43228552428668,-2.88846221882935,20.3379143046628));
#16582=CARTESIAN_POINT('Ctrl Pts',(1.34887693653242,-2.92834240706479,20.3317553119291));
#16583=CARTESIAN_POINT('Ctrl Pts',(1.22128111550323,-2.98273916011704,20.3227342276422));
#16584=CARTESIAN_POINT('Ctrl Pts',(1.17830904076372,-2.9999747988446,20.3197620595982));
#16585=CARTESIAN_POINT('Ctrl Pts',(1.12472705459159,-3.02013684708874,20.3161498424875));
#16586=CARTESIAN_POINT('Ctrl Pts',(1.11445635505942,-3.02394189152159,20.3154616579489));
#16587=CARTESIAN_POINT('Ctrl Pts',(1.09815557219796,-3.02988660438592,20.3143763167279));
#16588=CARTESIAN_POINT('Ctrl Pts',(1.09213828426504,-3.03206076224097,20.3139771533421));
#16589=CARTESIAN_POINT('Ctrl Pts',(1.08084422142813,-3.03610353353027,20.3132307762371));
#16590=CARTESIAN_POINT('Ctrl Pts',(1.0755691143866,-3.03797629649145,20.3128833260842));
#16591=CARTESIAN_POINT('Ctrl Pts',(1.06346238302641,-3.04223892925854,20.3120885295093));
#16592=CARTESIAN_POINT('Ctrl Pts',(1.05662757989833,-3.04461953331037,20.3116417370742));
#16593=CARTESIAN_POINT('Ctrl Pts',(1.03866701523993,-3.05080754388606,20.3104725065262));
#16594=CARTESIAN_POINT('Ctrl Pts',(1.02752821529575,-3.05457715812865,20.3097522491478));
#16595=CARTESIAN_POINT('Ctrl Pts',(0.951480412198136,-3.07985034135917,
20.3048664235266));
#16596=CARTESIAN_POINT('Ctrl Pts',(0.885916736396182,-3.09934608524292,
20.3008104733203));
#16597=CARTESIAN_POINT('Ctrl Pts',(0.792185486093892,-3.12399963083853,
20.2951666747592));
#16598=CARTESIAN_POINT('Ctrl Pts',(0.764497875989363,-3.1308903865538,20.2935183760302));
#16599=CARTESIAN_POINT('Ctrl Pts',(0.486427029054515,-3.19618649732061,
20.2771200303123));
#16600=CARTESIAN_POINT('Ctrl Pts',(0.229993707192357,-3.22480013484399,
20.2631807265878));
#16601=CARTESIAN_POINT('Ctrl Pts',(-0.107817291833416,-3.22195662129813,
20.2438394675536));
#16602=CARTESIAN_POINT('Ctrl Pts',(-0.188449265195834,-3.21824711955131,
20.2391571262057));
#16603=CARTESIAN_POINT('Ctrl Pts',(-0.319515712341894,-3.20727484932672,
20.2313799938083));
#16604=CARTESIAN_POINT('Ctrl Pts',(-0.370068567194212,-3.20183557855471,
20.2283400132662));
#16605=CARTESIAN_POINT('Ctrl Pts',(-0.436521147958708,-3.19309081671208,
20.2242822137591));
#16606=CARTESIAN_POINT('Ctrl Pts',(-0.452556315503421,-3.19085763436655,
20.2232983124319));
#16607=CARTESIAN_POINT('Ctrl Pts',(-0.479310679560346,-3.18692588653344,
20.2216484882992));
#16608=CARTESIAN_POINT('Ctrl Pts',(-0.490039463727698,-3.18529380956157,
20.2209846823272));
#16609=CARTESIAN_POINT('Ctrl Pts',(-0.510719701399489,-3.18204094963412,
20.2197008167466));
#16610=CARTESIAN_POINT('Ctrl Pts',(-0.520672207161982,-3.18042759193602,
20.2190810004579));
#16611=CARTESIAN_POINT('Ctrl Pts',(-0.543534810750672,-3.17661124383535,
20.217652624557));
#16612=CARTESIAN_POINT('Ctrl Pts',(-0.556439312019799,-3.17437621728409,
20.2168430522169));
#16613=CARTESIAN_POINT('Ctrl Pts',(-0.590893704973165,-3.16819225723482,
20.2146724239986));
#16614=CARTESIAN_POINT('Ctrl Pts',(-0.612417258319161,-3.16410218115768,
20.213306887312));
#16615=CARTESIAN_POINT('Ctrl Pts',(-0.794565218114907,-3.12756084875824,
20.2016676644578));
#16616=CARTESIAN_POINT('Ctrl Pts',(-0.952515678574345,-3.08312665038861,
20.1910066877899));
#16617=CARTESIAN_POINT('Ctrl Pts',(-1.23270251018825,-2.98071306369046,
20.1711098801217));
#16618=CARTESIAN_POINT('Ctrl Pts',(-1.35589394543767,-2.92672056723879,
20.1619922847839));
#16619=CARTESIAN_POINT('Ctrl Pts',(-1.4752556264295,-2.8652641063588,20.1529125281009));
#16620=CARTESIAN_POINT('Ctrl Pts',(-1.47525540330811,-2.86526422123863,
19.9090518554891));
#16621=CARTESIAN_POINT('Ctrl Pts',(-1.43059364733655,-2.88825948161633,
19.9124054158376));
#16622=CARTESIAN_POINT('Ctrl Pts',(-1.38537564121385,-2.91022009359238,
19.9157346329231));
#16623=CARTESIAN_POINT('Ctrl Pts',(-1.2884052929316,-2.95453925547849,19.9227095951287));
#16624=CARTESIAN_POINT('Ctrl Pts',(-1.23656546639833,-2.97660833423677,
19.9263420874058));
#16625=CARTESIAN_POINT('Ctrl Pts',(-1.173315447835,-3.00159701465284,19.9306366803748));
#16626=CARTESIAN_POINT('Ctrl Pts',(-1.16243730808193,-3.00582655739098,
19.9313704526167));
#16627=CARTESIAN_POINT('Ctrl Pts',(-1.14546075708148,-3.01232128603614,
19.9325077964155));
#16628=CARTESIAN_POINT('Ctrl Pts',(-1.13937819040285,-3.01462721034128,
19.9329137474391));
#16629=CARTESIAN_POINT('Ctrl Pts',(-1.12806404462338,-3.01887731146156,
19.9336659210117));
#16630=CARTESIAN_POINT('Ctrl Pts',(-1.122834447533,-3.02082629665752,19.934012421613));
#16631=CARTESIAN_POINT('Ctrl Pts',(-1.11096515309334,-3.02521470729258,
19.9347962316453));
#16632=CARTESIAN_POINT('Ctrl Pts',(-1.10432248725709,-3.02764585825333,
19.9352330434412));
#16633=CARTESIAN_POINT('Ctrl Pts',(-1.08458191114903,-3.03479710553718,
19.9365258253445));
#16634=CARTESIAN_POINT('Ctrl Pts',(-1.07146116147525,-3.03945429138847,
19.9373781379427));
#16635=CARTESIAN_POINT('Ctrl Pts',(-0.971537604603511,-3.07419450798429,
19.9438193786349));
#16636=CARTESIAN_POINT('Ctrl Pts',(-0.883505585124597,-3.10064162017366,
19.9492102670712));
#16637=CARTESIAN_POINT('Ctrl Pts',(-0.558966391189524,-3.18319293008847,
19.9684645368859));
#16638=CARTESIAN_POINT('Ctrl Pts',(-0.317451220646878,-3.21627090049025,
19.9816737641273));
#16639=CARTESIAN_POINT('Ctrl Pts',(0.017371273963098,-3.22401316464108,
20.0007408304169));
#16640=CARTESIAN_POINT('Ctrl Pts',(0.109286574692442,-3.22220687777445,
20.0060451891133));
#16641=CARTESIAN_POINT('Ctrl Pts',(0.256967022909014,-3.21297847584007,
20.0147704959626));
#16642=CARTESIAN_POINT('Ctrl Pts',(0.312836077540626,-3.20802053450097,
20.0181179889282));
#16643=CARTESIAN_POINT('Ctrl Pts',(0.385603084667792,-3.19964414589995,
20.0225504260731));
#16644=CARTESIAN_POINT('Ctrl Pts',(0.402645022190167,-3.19754427141391,
20.0235936925333));
#16645=CARTESIAN_POINT('Ctrl Pts',(0.430424712482557,-3.19389571023135,
20.0253031014704));
#16646=CARTESIAN_POINT('Ctrl Pts',(0.441173005347996,-3.19242879572148,
20.025966647184));
#16647=CARTESIAN_POINT('Ctrl Pts',(0.461893078703285,-3.18949430697291,
20.0272500444734));
#16648=CARTESIAN_POINT('Ctrl Pts',(0.471865796048477,-3.18803416186256,
20.0278696530981));
#16649=CARTESIAN_POINT('Ctrl Pts',(0.494777328685117,-3.18456973330488,
20.0292975994978));
#16650=CARTESIAN_POINT('Ctrl Pts',(0.507711041074096,-3.18253334340763,
20.0301069496362));
#16651=CARTESIAN_POINT('Ctrl Pts',(0.542248440319117,-3.17687959969929,
20.0322770861719));
#16652=CARTESIAN_POINT('Ctrl Pts',(0.563827963357143,-3.17312075904579,
20.0336423520319));
#16653=CARTESIAN_POINT('Ctrl Pts',(0.74654716372541,-3.13937099560035,20.0452835848779));
#16654=CARTESIAN_POINT('Ctrl Pts',(0.905195752620308,-3.09735191204722,
20.0559470312609));
#16655=CARTESIAN_POINT('Ctrl Pts',(1.2997804612932,-2.95993042531818,20.0838151461165));
#16656=CARTESIAN_POINT('Ctrl Pts',(1.52889307559395,-2.84835014186709,20.1013456978682));
#16657=CARTESIAN_POINT('Ctrl Pts',(1.78990399511722,-2.68058445922449,20.1216439373497));
#16658=CARTESIAN_POINT('Ctrl Pts',(1.83647744846099,-2.64889426983437,20.1252758102766));
#16659=CARTESIAN_POINT('Ctrl Pts',(1.89167286329933,-2.6091813933757,20.1295697719503));
#16660=CARTESIAN_POINT('Ctrl Pts',(1.90110929303378,-2.60231382255424,20.1303035081653));
#16661=CARTESIAN_POINT('Ctrl Pts',(1.91574691020634,-2.59153885765746,20.1314408083938));
#16662=CARTESIAN_POINT('Ctrl Pts',(1.92097381189348,-2.58766680438355,20.1318467515854));
#16663=CARTESIAN_POINT('Ctrl Pts',(1.93066350703265,-2.5804432047977,20.1325989180819));
#16664=CARTESIAN_POINT('Ctrl Pts',(1.93512927498804,-2.57709592378187,20.1329454193927));
#16665=CARTESIAN_POINT('Ctrl Pts',(1.94523555673107,-2.56947975820593,20.1337292404925));
#16666=CARTESIAN_POINT('Ctrl Pts',(1.9508707114145,-2.56520390390303,20.1341660625877));
#16667=CARTESIAN_POINT('Ctrl Pts',(1.96755560463566,-2.55245692589137,20.1354589032418));
#16668=CARTESIAN_POINT('Ctrl Pts',(1.97856474330087,-2.54393258335488,20.1363112637982));
#16669=CARTESIAN_POINT('Ctrl Pts',(2.06180923517692,-2.47860933068432,20.1427539864464));
#16670=CARTESIAN_POINT('Ctrl Pts',(2.13164810818292,-2.41880988654524,20.1481462058679));
#16671=CARTESIAN_POINT('Ctrl Pts',(2.37646464157625,-2.19033378829858,20.1673999172869));
#16672=CARTESIAN_POINT('Ctrl Pts',(2.53477886146611,-2.00500761500875,20.1806076309195));
#16673=CARTESIAN_POINT('Ctrl Pts',(2.72220038006782,-1.72748032725434,20.1996731557343));
#16674=CARTESIAN_POINT('Ctrl Pts',(2.77034849214687,-1.64916054216864,20.2049776778626));
#16675=CARTESIAN_POINT('Ctrl Pts',(2.84238438129296,-1.51990588878749,20.2137032290034));
#16676=CARTESIAN_POINT('Ctrl Pts',(2.86840192106599,-1.47021519686481,20.2170507974422));
#16677=CARTESIAN_POINT('Ctrl Pts',(2.9006738132955,-1.40445855511251,20.2214833206224));
#16678=CARTESIAN_POINT('Ctrl Pts',(2.90811552800719,-1.3889839675746,20.2225265955898));
#16679=CARTESIAN_POINT('Ctrl Pts',(2.92005624595743,-1.3636373279111,20.2242360149641));
#16680=CARTESIAN_POINT('Ctrl Pts',(2.92462975280815,-1.35380059316961,20.2248995625466));
#16681=CARTESIAN_POINT('Ctrl Pts',(2.93335660632352,-1.33478019549209,20.2261829609906));
#16682=CARTESIAN_POINT('Ctrl Pts',(2.93751671077762,-1.32559975873509,20.2268025688877));
#16683=CARTESIAN_POINT('Ctrl Pts',(2.9469817590324,-1.30444911794695,20.2282305100838));
#16684=CARTESIAN_POINT('Ctrl Pts',(2.95225693048704,-1.29246585937163,20.229039855722));
#16685=CARTESIAN_POINT('Ctrl Pts',(2.96616171916738,-1.26034995417123,20.2312099723427));
#16686=CARTESIAN_POINT('Ctrl Pts',(2.97465923040746,-1.24016118949239,20.2325752226589));
#16687=CARTESIAN_POINT('Ctrl Pts',(3.04498798364075,-1.06818867824241,20.2442156649899));
#16688=CARTESIAN_POINT('Ctrl Pts',(3.09535393480341,-0.912002300567566,
20.2548782755466));
#16689=CARTESIAN_POINT('Ctrl Pts',(3.19293068539289,-0.505764808144659,
20.282743773313));
#16690=CARTESIAN_POINT('Ctrl Pts',(3.22284582310859,-0.252714055134884,
20.3002724897376));
#16691=CARTESIAN_POINT('Ctrl Pts',(3.22272882498705,0.0565890285072366,
20.3205073847095));
#16692=CARTESIAN_POINT('Ctrl Pts',(3.22128091307601,0.11195331730861,20.3240790385116));
#16693=CARTESIAN_POINT('Ctrl Pts',(3.21783469679233,0.178266586000064,20.328275425723));
#16694=CARTESIAN_POINT('Ctrl Pts',(3.21720601370459,0.189273836510378,20.3289692737853));
#16695=CARTESIAN_POINT('Ctrl Pts',(3.21608497941296,0.207277976993981,20.3300995100013));
#16696=CARTESIAN_POINT('Ctrl Pts',(3.21562625717631,0.214276762442052,20.3305377148613));
#16697=CARTESIAN_POINT('Ctrl Pts',(3.21476178402536,0.22683768393226,20.3313220336635));
#16698=CARTESIAN_POINT('Ctrl Pts',(3.2143644426741,0.232400288401883,20.331668611077));
#16699=CARTESIAN_POINT('Ctrl Pts',(3.21346902791398,0.244493904199337,20.3324204468636));
#16700=CARTESIAN_POINT('Ctrl Pts',(3.21296548478553,0.2510244170038,20.3328253940434));
#16701=CARTESIAN_POINT('Ctrl Pts',(3.21149279830193,0.269393111152186,20.3339615913295));
#16702=CARTESIAN_POINT('Ctrl Pts',(3.21047810202809,0.281227680896662,20.3346903257257));
#16703=CARTESIAN_POINT('Ctrl Pts',(3.20395303145869,0.352686741949944,20.3390720920251));
#16704=CARTESIAN_POINT('Ctrl Pts',(3.19684684816458,0.412158047780392,20.3426411780582));
#16705=CARTESIAN_POINT('Ctrl Pts',(3.15131524322269,0.720088476940664,20.3608762159645));
#16706=CARTESIAN_POINT('Ctrl Pts',(3.08556915115906,0.963640744857692,20.3745244198022));
#16707=CARTESIAN_POINT('Ctrl Pts',(2.93178788686179,1.34802195342613,20.3979169732379));
#16708=CARTESIAN_POINT('Ctrl Pts',(2.86007993088528,1.49414722746266,20.4072883198121));
#16709=CARTESIAN_POINT('Ctrl Pts',(2.7665690792335,1.65308551433941,20.4183800688993));
#16710=CARTESIAN_POINT('Ctrl Pts',(2.75528367714294,1.67182774537481,20.4197026878485));
#16711=CARTESIAN_POINT('Ctrl Pts',(2.73694482775648,1.70159389875943,20.421827526181));
#16712=CARTESIAN_POINT('Ctrl Pts',(2.73001341266207,1.71269248414219,20.4226252583894));
#16713=CARTESIAN_POINT('Ctrl Pts',(2.71762434755924,1.73226355709479,20.4240418236202));
#16714=CARTESIAN_POINT('Ctrl Pts',(2.71219415423518,1.74075328285015,20.4246596302377));
#16715=CARTESIAN_POINT('Ctrl Pts',(2.70083445733673,1.75833118296704,20.4259457683132));
#16716=CARTESIAN_POINT('Ctrl Pts',(2.69489870136719,1.76741514639021,20.4266143288479));
#16717=CARTESIAN_POINT('Ctrl Pts',(2.67944367762728,1.79080833973204,20.4283462401536));
#16718=CARTESIAN_POINT('Ctrl Pts',(2.66985571581806,1.80507156907996,20.4294121742095));
#16719=CARTESIAN_POINT('Ctrl Pts',(2.62841608890123,1.86566542037911,20.4339838327829));
#16720=CARTESIAN_POINT('Ctrl Pts',(2.59547065082444,1.91123260109075,20.4375310874418));
#16721=CARTESIAN_POINT('Ctrl Pts',(2.50538165199908,2.02920802967106,20.4470151165299));
#16722=CARTESIAN_POINT('Ctrl Pts',(2.44629576541941,2.10006117389156,20.4530240540219));
#16723=CARTESIAN_POINT('Ctrl Pts',(2.22314640179419,2.34543811945696,20.4749682767047));
#16724=CARTESIAN_POINT('Ctrl Pts',(2.04280962477906,2.50407153022852,20.4914294610284));
#16725=CARTESIAN_POINT('Ctrl Pts',(1.82179466870766,2.65858914126104,20.5093885050216));
#16726=CARTESIAN_POINT('Ctrl Pts',(1.79676740234166,2.67556704894589,20.5113921426775));
#16727=CARTESIAN_POINT('Ctrl Pts',(1.715914209649,2.72876973637368,20.517761598418));
#16728=CARTESIAN_POINT('Ctrl Pts',(1.65919983656839,2.76362139095914,20.522074508461));
#16729=CARTESIAN_POINT('Ctrl Pts',(1.59132073202676,2.80249030937626,20.5270221392162));
#16730=CARTESIAN_POINT('Ctrl Pts',(1.58116735857222,2.80823136515241,20.5277567005687));
#16731=CARTESIAN_POINT('Ctrl Pts',(1.56468968310015,2.81743069236902,20.5289396426155));
#16732=CARTESIAN_POINT('Ctrl Pts',(1.55838466428329,2.82092303177971,20.529390128335));
#16733=CARTESIAN_POINT('Ctrl Pts',(1.54716633851884,2.82708775313512,20.5301877701745));
#16734=CARTESIAN_POINT('Ctrl Pts',(1.54225774521927,2.82976852268922,20.5305354583536));
#16735=CARTESIAN_POINT('Ctrl Pts',(1.53170577647935,2.83549574207186,20.53128003427));
#16736=CARTESIAN_POINT('Ctrl Pts',(1.52606029464082,2.83853812160837,20.5316766624953));
#16737=CARTESIAN_POINT('Ctrl Pts',(1.5104848697193,2.84687190111473,20.5327662675448));
#16738=CARTESIAN_POINT('Ctrl Pts',(1.50053612632213,2.85212824139069,20.5334570494147));
#16739=CARTESIAN_POINT('Ctrl Pts',(1.44635048270484,2.88039479698909,20.5371923321958));
#16740=CARTESIAN_POINT('Ctrl Pts',(1.40160893316019,2.90242948925155,20.5401790810496));
#16741=CARTESIAN_POINT('Ctrl Pts',(1.12140652716319,3.03243431434718,20.5583972938457));
#16742=CARTESIAN_POINT('Ctrl Pts',(0.874131878556189,3.11273753382656,20.5724421024193));
#16743=CARTESIAN_POINT('Ctrl Pts',(0.457025189978494,3.19449346324033,20.5964381437279));
#16744=CARTESIAN_POINT('Ctrl Pts',(0.291962332503283,3.21378402454912,20.6059953026084));
#16745=CARTESIAN_POINT('Ctrl Pts',(0.104232790564992,3.22113872450317,20.6172949558947));
#16746=CARTESIAN_POINT('Ctrl Pts',(0.0822965744579971,3.22177379629132,
20.6186216148224));
#16747=CARTESIAN_POINT('Ctrl Pts',(0.0472532656245252,3.22243020607399,
20.6207517166503));
#16748=CARTESIAN_POINT('Ctrl Pts',(0.0341493206615145,3.22259571154476,
20.6215506367417));
#16749=CARTESIAN_POINT('Ctrl Pts',(0.0109641388187761,3.22274711633592,
20.6229685767907));
#16750=CARTESIAN_POINT('Ctrl Pts',(0.000883235815767659,3.2227656452833,
20.6235865636895));
#16751=CARTESIAN_POINT('Ctrl Pts',(-0.0200402444660291,3.22270593092331,
20.624872345095));
#16752=CARTESIAN_POINT('Ctrl Pts',(-0.0308826578445186,3.22262026702658,
20.625540365042));
#16753=CARTESIAN_POINT('Ctrl Pts',(-0.0588701856281349,3.22225788748839,
20.6272693036906));
#16754=CARTESIAN_POINT('Ctrl Pts',(-0.0760137250679063,3.22189904986492,
20.6283327888876));
#16755=CARTESIAN_POINT('Ctrl Pts',(-0.148998447703224,3.2197885506647,20.6328797652262));
#16756=CARTESIAN_POINT('Ctrl Pts',(-0.204789093561608,3.21672187873367,
20.6364042310468));
#16757=CARTESIAN_POINT('Ctrl Pts',(-0.351579871151899,3.20481901177623,
20.6458119421613));
#16758=CARTESIAN_POINT('Ctrl Pts',(-0.442327499869453,3.19355870535963,
20.6517659150887));
#16759=CARTESIAN_POINT('Ctrl Pts',(-0.776325528478468,3.13760606711091,
20.674163348959));
#16760=CARTESIAN_POINT('Ctrl Pts',(-1.01464607421257,3.06883215841772,20.6911823289542));
#16761=CARTESIAN_POINT('Ctrl Pts',(-1.32447853273326,2.9393401510836,20.713494840073));
#16762=CARTESIAN_POINT('Ctrl Pts',(-1.40477267742463,2.90182368975267,20.7192857620217));
#16763=CARTESIAN_POINT('Ctrl Pts',(-1.49568364174185,2.85468713671611,20.7257712492287));
#16764=CARTESIAN_POINT('Ctrl Pts',(-1.50790058231765,2.84825280735781,20.7266412469668));
#16765=CARTESIAN_POINT('Ctrl Pts',(-1.52629159731091,2.83841526376611,20.7279481424801));
#16766=CARTESIAN_POINT('Ctrl Pts',(-1.53249629291243,2.83507008097799,20.7283885781568));
#16767=CARTESIAN_POINT('Ctrl Pts',(-1.54359222503694,2.82904077955072,20.7291752843002));
#16768=CARTESIAN_POINT('Ctrl Pts',(-1.54848749310999,2.82636430326622,20.7295220307416));
#16769=CARTESIAN_POINT('Ctrl Pts',(-1.55909120527533,2.82053092986941,20.7302723981622));
#16770=CARTESIAN_POINT('Ctrl Pts',(-1.564797005452,2.81736941955191,20.7306757179039));
#16771=CARTESIAN_POINT('Ctrl Pts',(-1.5807575489111,2.80846244444094,20.7318027557087));
#16772=CARTESIAN_POINT('Ctrl Pts',(-1.59099063962236,2.80267809868083,20.7325240226806));
#16773=CARTESIAN_POINT('Ctrl Pts',(-1.65129116581673,2.76815599566594,20.7367677147697));
#16774=CARTESIAN_POINT('Ctrl Pts',(-1.70061424802841,2.73813116351675,20.7402122235753));
#16775=CARTESIAN_POINT('Ctrl Pts',(-1.96152439243689,2.56953331030511,20.7584356009522));
#16776=CARTESIAN_POINT('Ctrl Pts',(-2.15706493037836,2.40773268599829,20.7721627041973));
#16777=CARTESIAN_POINT('Ctrl Pts',(-2.44447442685418,2.10650358354623,20.7956827307223));
#16778=CARTESIAN_POINT('Ctrl Pts',(-2.54809538238246,1.97990204823421,20.8050992443411));
#16779=CARTESIAN_POINT('Ctrl Pts',(-2.65420633500666,1.82805515489491,20.8162414977202));
#16780=CARTESIAN_POINT('Ctrl Pts',(-2.66656394562522,1.80998165896321,20.8175651114207));
#16781=CARTESIAN_POINT('Ctrl Pts',(-2.68601406075094,1.78090352893238,20.8196912458699));
#16782=CARTESIAN_POINT('Ctrl Pts',(-2.69322546249081,1.76997895868048,20.8204892706818));
#16783=CARTESIAN_POINT('Ctrl Pts',(-2.70587104179589,1.75056592169788,20.8219061744347));
#16784=CARTESIAN_POINT('Ctrl Pts',(-2.71133236162739,1.74209527930201,20.8225240253321));
#16785=CARTESIAN_POINT('Ctrl Pts',(-2.72258989951244,1.72445339395382,20.8238100749195));
#16786=CARTESIAN_POINT('Ctrl Pts',(-2.72837971126088,1.71527823265415,20.8244785017883));
#16787=CARTESIAN_POINT('Ctrl Pts',(-2.74321608235527,1.69150173674997,20.8262096781686));
#16788=CARTESIAN_POINT('Ctrl Pts',(-2.75219234481016,1.67685714319281,20.8272750068103));
#16789=CARTESIAN_POINT('Ctrl Pts',(-2.79000285477184,1.61404857269709,20.8318405508547));
#16790=CARTESIAN_POINT('Ctrl Pts',(-2.81769165543471,1.56520983261283,20.8353821584189));
#16791=CARTESIAN_POINT('Ctrl Pts',(-2.887367285934,1.43446696320475,20.8448472545682));
#16792=CARTESIAN_POINT('Ctrl Pts',(-2.92714336674572,1.3514490350802,20.8508425485672));
#16793=CARTESIAN_POINT('Ctrl Pts',(-3.05835586934631,1.04452739272671,20.8729250471122));
#16794=CARTESIAN_POINT('Ctrl Pts',(-3.12807125861198,0.812239784608602,
20.8895524387025));
#16795=CARTESIAN_POINT('Ctrl Pts',(-3.18770530887634,0.482985157539663,
20.9118209845893));
#16796=CARTESIAN_POINT('Ctrl Pts',(-3.20029910267135,0.390933432686804,
20.9179011624078));
#16797=CARTESIAN_POINT('Ctrl Pts',(-3.21019258239435,0.284562630579857,
20.9246681250829));
#16798=CARTESIAN_POINT('Ctrl Pts',(-3.21139471910581,0.270658976312678,
20.9255475475012));
#16799=CARTESIAN_POINT('Ctrl Pts',(-3.21307061028902,0.249689704848372,
20.9268657771642));
#16800=CARTESIAN_POINT('Ctrl Pts',(-3.21361143624875,0.242629830184885,
20.9273082122274));
#16801=CARTESIAN_POINT('Ctrl Pts',(-3.21453698031546,0.230001560988902,
20.9280970711628));
#16802=CARTESIAN_POINT('Ctrl Pts',(-3.21493050237897,0.2244339152739,20.9284439821962));
#16803=CARTESIAN_POINT('Ctrl Pts',(-3.21575098718649,0.212380316170144,
20.929193093328));
#16804=CARTESIAN_POINT('Ctrl Pts',(-3.216172792279,0.20589410446725,20.9295950008836));
#16805=CARTESIAN_POINT('Ctrl Pts',(-3.21729568418752,0.187781032326448,
20.9307141093516));
#16806=CARTESIAN_POINT('Ctrl Pts',(-3.21795337358538,0.17615144245827,20.9314289144922));
#16807=CARTESIAN_POINT('Ctrl Pts',(-3.22140390745169,0.108647058728933,
20.9355577441873));
#16808=CARTESIAN_POINT('Ctrl Pts',(-3.22280470667723,0.0527069175510339,
20.9388986876561));
#16809=CARTESIAN_POINT('Ctrl Pts',(-3.22249238833365,-0.257458018862945,
20.9571155695141));
#16810=CARTESIAN_POINT('Ctrl Pts',(-3.19215944264278,-0.510771299372993,
20.9709106357355));
#16811=CARTESIAN_POINT('Ctrl Pts',(-3.09378614221512,-0.917339506017467,
20.9945372654579));
#16812=CARTESIAN_POINT('Ctrl Pts',(-3.04309930352166,-1.07357376295313,
21.0039891562796));
#16813=CARTESIAN_POINT('Ctrl Pts',(-2.97241861120438,-1.24552201332927,
21.0151709814409));
#16814=CARTESIAN_POINT('Ctrl Pts',(-2.96388348962222,-1.26569826956019,
21.0164953680751));
#16815=CARTESIAN_POINT('Ctrl Pts',(-2.94991939163909,-1.29779220053816,
21.0186225095763));
#16816=CARTESIAN_POINT('Ctrl Pts',(-2.94462223104488,-1.30976674314188,
21.019420761693));
#16817=CARTESIAN_POINT('Ctrl Pts',(-2.9351186366654,-1.33090110139177,21.0208379284795));
#16818=CARTESIAN_POINT('Ctrl Pts',(-2.9309419043456,-1.3400741407368,21.0214558138328));
#16819=CARTESIAN_POINT('Ctrl Pts',(-2.92218081748639,-1.35907854925507,
21.0227417949653));
#16820=CARTESIAN_POINT('Ctrl Pts',(-2.91758972435345,-1.36890665454996,
21.0234101182268));
#16821=CARTESIAN_POINT('Ctrl Pts',(-2.90560406909069,-1.3942300157804,21.0251407249081));
#16822=CARTESIAN_POINT('Ctrl Pts',(-2.89813521475951,-1.40968954092806,
21.0262055842394));
#16823=CARTESIAN_POINT('Ctrl Pts',(-2.86575059353019,-1.47537609712777,
21.0307663940314));
#16824=CARTESIAN_POINT('Ctrl Pts',(-2.8396511648637,-1.52500548098698,21.0343036299909));
#16825=CARTESIAN_POINT('Ctrl Pts',(-2.76740708042064,-1.65409029240971,
21.0437540791577));
#16826=CARTESIAN_POINT('Ctrl Pts',(-2.71913897162283,-1.73229252164342,
21.0497388217944));
#16827=CARTESIAN_POINT('Ctrl Pts',(-2.53102936976523,-2.0097881813213,21.07191572751));
#16828=CARTESIAN_POINT('Ctrl Pts',(-2.37209054798314,-2.19511493300139,
21.088658188419));
#16829=CARTESIAN_POINT('Ctrl Pts',(-2.12674616973946,-2.42310789164414,
21.1109371020969));
#16830=CARTESIAN_POINT('Ctrl Pts',(-2.05704101931461,-2.48255649322211,
21.1169296606735));
#16831=CARTESIAN_POINT('Ctrl Pts',(-1.97393166968701,-2.54752916970758,
21.1236115473473));
#16832=CARTESIAN_POINT('Ctrl Pts',(-1.96291583197397,-2.55602671349855,
21.1244882236578));
#16833=CARTESIAN_POINT('Ctrl Pts',(-1.94621821876125,-2.56873552755151,
21.1258031520079));
#16834=CARTESIAN_POINT('Ctrl Pts',(-1.94057721188963,-2.57299973814683,
21.1262450055616));
#16835=CARTESIAN_POINT('Ctrl Pts',(-1.93045915347212,-2.58059608710188,
21.1270332371268));
#16836=CARTESIAN_POINT('Ctrl Pts',(-1.92598745573521,-2.58393518299284,
21.1273800990478));
#16837=CARTESIAN_POINT('Ctrl Pts',(-1.91628349109191,-2.59114211863501,
21.1281295698948));
#16838=CARTESIAN_POINT('Ctrl Pts',(-1.91104819375541,-2.59500572255781,
21.1285318837708));
#16839=CARTESIAN_POINT('Ctrl Pts',(-1.896383515664,-2.60575968037963,21.1296532719735));
#16840=CARTESIAN_POINT('Ctrl Pts',(-1.88692821635097,-2.61261475660756,
21.1303699346826));
#16841=CARTESIAN_POINT('Ctrl Pts',(-1.83155358487942,-2.65230383777476,
21.1345313613818));
#16842=CARTESIAN_POINT('Ctrl Pts',(-1.78481207014196,-2.68398043156078,
21.1379016887379));
#16843=CARTESIAN_POINT('Ctrl Pts',(-1.65226489266357,-2.76881227520234,
21.1471413340034));
#16844=CARTESIAN_POINT('Ctrl Pts',(-1.56483039988362,-2.81914422829277,
21.1528793324542));
#16845=CARTESIAN_POINT('Ctrl Pts',(-1.47525512068014,-2.86526436675694,
21.1585511949183));
#16846=CARTESIAN_POINT('Origin',(0.,0.,4.68922655072688));
#16847=CARTESIAN_POINT('',(-1.47525567074797,-2.86526408354029,22.6538402050192));
#16848=CARTESIAN_POINT('',(-1.47525540254685,-2.86526422163059,22.4042343665403));
#16849=CARTESIAN_POINT('',(-1.47525540501186,-2.86526422036142,4.68922655072688));
#16850=CARTESIAN_POINT('',(3.21778804064233,0.000208849362278093,21.8109814966979));
#16851=CARTESIAN_POINT('Ctrl Pts',(-1.47525567074797,-2.86526408354029,
22.6538402050192));
#16852=CARTESIAN_POINT('Ctrl Pts',(-1.59395129052928,-2.80415055924728,
22.6463741799665));
#16853=CARTESIAN_POINT('Ctrl Pts',(-1.70883224031351,-2.73567054746652,
22.6388641912748));
#16854=CARTESIAN_POINT('Ctrl Pts',(-1.89870517497142,-2.60582223290445,
22.6255690687147));
#16855=CARTESIAN_POINT('Ctrl Pts',(-1.97571020711639,-2.54793197975155,
22.6199016273927));
#16856=CARTESIAN_POINT('Ctrl Pts',(-2.06493547434476,-2.47437538588842,
22.6129308383243));
#16857=CARTESIAN_POINT('Ctrl Pts',(-2.07975612873059,-2.46193145382807,
22.6117589647593));
#16858=CARTESIAN_POINT('Ctrl Pts',(-2.10393967710873,-2.44125190312021,
22.6098230902081));
#16859=CARTESIAN_POINT('Ctrl Pts',(-2.11336857710181,-2.43309397061587,
22.6090622919252));
#16860=CARTESIAN_POINT('Ctrl Pts',(-2.13025681712948,-2.41830994659176,
22.6076885960526));
#16861=CARTESIAN_POINT('Ctrl Pts',(-2.13773321125937,-2.41170350968555,
22.6070765240084));
#16862=CARTESIAN_POINT('Ctrl Pts',(-2.15361492482094,-2.39753792604147,
22.6057678265943));
#16863=CARTESIAN_POINT('Ctrl Pts',(-2.16201137145421,-2.38996907421465,
22.605070795996));
#16864=CARTESIAN_POINT('Ctrl Pts',(-2.18457767229459,-2.36941078420404,
22.6031833981221));
#16865=CARTESIAN_POINT('Ctrl Pts',(-2.19867124373978,-2.35633864431985,
22.6019895141823));
#16866=CARTESIAN_POINT('Ctrl Pts',(-2.26953082816861,-2.28942538429351,
22.5959087262619));
#16867=CARTESIAN_POINT('Ctrl Pts',(-2.32443553587578,-2.23365988856786,
22.5909385365495));
#16868=CARTESIAN_POINT('Ctrl Pts',(-2.55443533166249,-1.98238281204841,
22.5689347652013));
#16869=CARTESIAN_POINT('Ctrl Pts',(-2.70729118301288,-1.76791284089322,
22.551023846707));
#16870=CARTESIAN_POINT('Ctrl Pts',(-2.89775382083268,-1.41700004791609,
22.5241359849261));
#16871=CARTESIAN_POINT('Ctrl Pts',(-2.95534375634447,-1.29260148780202,
22.5150322898949));
#16872=CARTESIAN_POINT('Ctrl Pts',(-3.01026399239769,-1.150935558751,22.5053984875968));
#16873=CARTESIAN_POINT('Ctrl Pts',(-3.01558138979936,-1.1369304579617,22.5044538574264));
#16874=CARTESIAN_POINT('Ctrl Pts',(-3.02330682749529,-1.11614744085675,
22.5030640696143));
#16875=CARTESIAN_POINT('Ctrl Pts',(-3.02579005383667,-1.10939796078506,
22.5026145876036));
#16876=CARTESIAN_POINT('Ctrl Pts',(-3.03016431509733,-1.09738464916309,
22.5018179435708));
#16877=CARTESIAN_POINT('Ctrl Pts',(-3.03206425801083,-1.09212416038817,
22.5014702555993));
#16878=CARTESIAN_POINT('Ctrl Pts',(-3.03611811845573,-1.0808078660793,22.5007248041255));
#16879=CARTESIAN_POINT('Ctrl Pts',(-3.03826761196424,-1.07475057217456,
22.5003273049443));
#16880=CARTESIAN_POINT('Ctrl Pts',(-3.04414960466641,-1.05801638564751,
22.4992332385375));
#16881=CARTESIAN_POINT('Ctrl Pts',(-3.04784408357195,-1.04732609009186,
22.4985388951071));
#16882=CARTESIAN_POINT('Ctrl Pts',(-3.06778219979724,-0.988634360706152,
22.4947507245502));
#16883=CARTESIAN_POINT('Ctrl Pts',(-3.0829492140565,-0.94027141500147,22.4917165902451));
#16884=CARTESIAN_POINT('Ctrl Pts',(-3.16846841782635,-0.643209970583038,
22.4734950773695));
#16885=CARTESIAN_POINT('Ctrl Pts',(-3.20984010007619,-0.387128211958623,
22.4594804483602));
#16886=CARTESIAN_POINT('Ctrl Pts',(-3.22679472407655,0.0366577776000503,
22.4355343236601));
#16887=CARTESIAN_POINT('Ctrl Pts',(-3.22064835929335,0.2023893017631,22.4259957306645));
#16888=CARTESIAN_POINT('Ctrl Pts',(-3.19929825503873,0.388702664193861,
22.4147165712294));
#16889=CARTESIAN_POINT('Ctrl Pts',(-3.19657747944004,0.410477121535496,
22.4133900098312));
#16890=CARTESIAN_POINT('Ctrl Pts',(-3.19187676228284,0.445210160735792,
22.4112598935972));
#16891=CARTESIAN_POINT('Ctrl Pts',(-3.19003972375883,0.458187631543052,
22.4104608598315));
#16892=CARTESIAN_POINT('Ctrl Pts',(-3.18664934270805,0.48112910692513,22.4090426145696));
#16893=CARTESIAN_POINT('Ctrl Pts',(-3.18512829190906,0.491097761470688,
22.4084244359355));
#16894=CARTESIAN_POINT('Ctrl Pts',(-3.18187392370323,0.511774922358287,
22.4071381517292));
#16895=CARTESIAN_POINT('Ctrl Pts',(-3.18013327650125,0.522482130392948,
22.4064698200499));
#16896=CARTESIAN_POINT('Ctrl Pts',(-3.17549981627052,0.550102631730018,
22.4047398493039));
#16897=CARTESIAN_POINT('Ctrl Pts',(-3.17252595247678,0.567001808706687,
22.4036756395635));
#16898=CARTESIAN_POINT('Ctrl Pts',(-3.1592826060433,0.638889811009705,22.3991234820072));
#16899=CARTESIAN_POINT('Ctrl Pts',(-3.14771780532546,0.693627249082833,
22.3955944507245));
#16900=CARTESIAN_POINT('Ctrl Pts',(-3.11348233097286,0.837095632719853,
22.3861720499949));
#16901=CARTESIAN_POINT('Ctrl Pts',(-3.08844551759512,0.925204363725221,
22.3802076910293));
#16902=CARTESIAN_POINT('Ctrl Pts',(-2.98245007986553,1.24563382940991,22.3578843759559));
#16903=CARTESIAN_POINT('Ctrl Pts',(-2.87873813428715,1.46951127851072,22.340958487716));
#16904=CARTESIAN_POINT('Ctrl Pts',(-2.70391060322844,1.75584939025165,22.3186584077431));
#16905=CARTESIAN_POINT('Ctrl Pts',(-2.65406555130686,1.83032206604534,22.3128008144069));
#16906=CARTESIAN_POINT('Ctrl Pts',(-2.59300324952485,1.91380339232455,22.3062500744374));
#16907=CARTESIAN_POINT('Ctrl Pts',(-2.58475677157753,1.92492642054307,22.3053776043138));
#16908=CARTESIAN_POINT('Ctrl Pts',(-2.57219837354516,1.94163923371114,22.3040676446802));
#16909=CARTESIAN_POINT('Ctrl Pts',(-2.56793948074423,1.94726839758761,22.303626594299));
#16910=CARTESIAN_POINT('Ctrl Pts',(-2.56027977441543,1.95732373257563,22.3028391172023));
#16911=CARTESIAN_POINT('Ctrl Pts',(-2.55688593841843,1.96175508584873,22.302492211615));
#16912=CARTESIAN_POINT('Ctrl Pts',(-2.54950266752828,1.97134376053639,22.3017418658776));
#16913=CARTESIAN_POINT('Ctrl Pts',(-2.54550910161745,1.97649778378345,22.3013387252002));
#16914=CARTESIAN_POINT('Ctrl Pts',(-2.53428447724387,1.99089363052469,22.300213091656));
#16915=CARTESIAN_POINT('Ctrl Pts',(-2.52701845699144,2.00010824395954,22.2994930389822));
#16916=CARTESIAN_POINT('Ctrl Pts',(-2.48395238004216,2.05411441393317,22.2952741657301));
#16917=CARTESIAN_POINT('Ctrl Pts',(-2.44700991682696,2.09798685874913,22.2918521928202));
#16918=CARTESIAN_POINT('Ctrl Pts',(-2.24065786219948,2.33017668466074,22.273624769719));
#16919=CARTESIAN_POINT('Ctrl Pts',(-2.05065486161858,2.49902227565613,22.2598781434133));
#16920=CARTESIAN_POINT('Ctrl Pts',(-1.70881839437805,2.7372865768509,22.2363394714562));
#16921=CARTESIAN_POINT('Ctrl Pts',(-1.56792633257803,2.82035365922715,22.2269257542924));
#16922=CARTESIAN_POINT('Ctrl Pts',(-1.40166323893353,2.90205776206202,22.2157836563833));
#16923=CARTESIAN_POINT('Ctrl Pts',(-1.38187105645885,2.91153420666235,22.2144570897182));
#16924=CARTESIAN_POINT('Ctrl Pts',(-1.35010510066578,2.92634679603342,22.2123269666227));
#16925=CARTESIAN_POINT('Ctrl Pts',(-1.33819265137013,2.93181339333739,22.211527931309));
#16926=CARTESIAN_POINT('Ctrl Pts',(-1.31705672322591,2.94135697235125,22.2101096842547));
#16927=CARTESIAN_POINT('Ctrl Pts',(-1.30784678057482,2.94546363852328,22.209491505385));
#16928=CARTESIAN_POINT('Ctrl Pts',(-1.2886896691464,2.95389813194206,22.2082052216403));
#16929=CARTESIAN_POINT('Ctrl Pts',(-1.27873963224085,2.95821909019347,22.207536890663));
#16930=CARTESIAN_POINT('Ctrl Pts',(-1.25299496510242,2.96924495524708,22.2058069237774));
#16931=CARTESIAN_POINT('Ctrl Pts',(-1.23716841760577,2.97587403546525,22.2047427172173));
#16932=CARTESIAN_POINT('Ctrl Pts',(-1.1695233091085,3.00357486230951,22.2001905916544));
#16933=CARTESIAN_POINT('Ctrl Pts',(-1.11721636204581,3.0234208591613,22.1966615899032));
#16934=CARTESIAN_POINT('Ctrl Pts',(-0.977998455384767,3.07213608949535,
22.1872392879752));
#16935=CARTESIAN_POINT('Ctrl Pts',(-0.890332533671326,3.09867820479817,
22.1812750001309));
#16936=CARTESIAN_POINT('Ctrl Pts',(-0.563428271747264,3.18263489796652,
22.1589512017364));
#16937=CARTESIAN_POINT('Ctrl Pts',(-0.318999298178052,3.21633957864115,
22.1420247028377));
#16938=CARTESIAN_POINT('Ctrl Pts',(0.0164072852926216,3.22395242924655,
22.1197245435649));
#16939=CARTESIAN_POINT('Ctrl Pts',(0.105998843521479,3.22225168076818,22.1138673903833));
#16940=CARTESIAN_POINT('Ctrl Pts',(0.209231663251922,3.21598062512818,22.1073170794617));
#16941=CARTESIAN_POINT('Ctrl Pts',(0.223046778683697,3.21505200903909,22.1064446241078));
#16942=CARTESIAN_POINT('Ctrl Pts',(0.243895259891753,3.21351559639254,22.105134682241));
#16943=CARTESIAN_POINT('Ctrl Pts',(0.250933107399983,3.21297369486896,22.1046936349974));
#16944=CARTESIAN_POINT('Ctrl Pts',(0.263532938620348,3.21196187829281,22.1039061612739));
#16945=CARTESIAN_POINT('Ctrl Pts',(0.269095512498012,3.21150063429049,22.1035592559397));
#16946=CARTESIAN_POINT('Ctrl Pts',(0.281153390932553,3.21046925622811,22.1028089082071));
#16947=CARTESIAN_POINT('Ctrl Pts',(0.287648152437793,3.20989386375882,22.1024057652952));
#16948=CARTESIAN_POINT('Ctrl Pts',(0.305826824667847,3.20822773769851,22.1012801191968));
#16949=CARTESIAN_POINT('Ctrl Pts',(0.317506731082661,3.20709288128821,22.1005600562913));
#16950=CARTESIAN_POINT('Ctrl Pts',(0.386223443863662,3.20003706707863,22.0963409993511));
#16951=CARTESIAN_POINT('Ctrl Pts',(0.443104151032635,3.19265805112663,22.0929188607913));
#16952=CARTESIAN_POINT('Ctrl Pts',(0.749980879806487,3.14448702791497,22.0746914259509));
#16953=CARTESIAN_POINT('Ctrl Pts',(0.994720160776134,3.07584597266029,22.0609449073278));
#16954=CARTESIAN_POINT('Ctrl Pts',(1.37991334895783,2.91695679789033,22.0374063976115));
#16955=CARTESIAN_POINT('Ctrl Pts',(1.5259393122153,2.84328976111937,22.0279927296228));
#16956=CARTESIAN_POINT('Ctrl Pts',(1.68618817838258,2.74653552841282,22.0167340207944));
#16957=CARTESIAN_POINT('Ctrl Pts',(1.70649564461843,2.73396425535425,22.0152895437326));
#16958=CARTESIAN_POINT('Ctrl Pts',(1.73706053886546,2.71456993622543,22.0130875549612));
#16959=CARTESIAN_POINT('Ctrl Pts',(1.74742195055384,2.70791169989794,22.0123361592619));
#16960=CARTESIAN_POINT('Ctrl Pts',(1.7657622079298,2.69597716689805,22.010997243));
#16961=CARTESIAN_POINT('Ctrl Pts',(1.7737562493654,2.69072440507944,22.010410609565));
#16962=CARTESIAN_POINT('Ctrl Pts',(1.78206910837562,2.6852090094271,22.0097973764916));
#16963=CARTESIAN_POINT('Ctrl Pts',(1.78241145366999,2.68498177668975,22.0097721162636));
#16964=CARTESIAN_POINT('Ctrl Pts',(1.78303958452356,2.68456467983984,22.0097257586782));
#16965=CARTESIAN_POINT('Ctrl Pts',(1.78332538578223,2.68437483385814,22.009704661884));
#16966=CARTESIAN_POINT('Ctrl Pts',(1.78385673916683,2.68402175541997,22.0096654319599));
#16967=CARTESIAN_POINT('Ctrl Pts',(1.78410229623998,2.68385853688113,22.0096472995028));
#16968=CARTESIAN_POINT('Ctrl Pts',(1.78456335181609,2.6835519881005,22.0096132486726));
#16969=CARTESIAN_POINT('Ctrl Pts',(1.7847788554715,2.68340866558655,22.009597330592));
#16970=CARTESIAN_POINT('Ctrl Pts',(1.78518662470617,2.68313740438402,22.0095672066249));
#16971=CARTESIAN_POINT('Ctrl Pts',(1.7853788938218,2.68300947097285,22.0095530009377));
#16972=CARTESIAN_POINT('Ctrl Pts',(1.78574498937772,2.68276581889266,22.009525948762));
#16973=CARTESIAN_POINT('Ctrl Pts',(1.78591881833183,2.68265010398946,22.009513102416));
#16974=CARTESIAN_POINT('Ctrl Pts',(1.78625153667906,2.68242857251684,22.0094885109731));
#16975=CARTESIAN_POINT('Ctrl Pts',(1.78641042791563,2.68232275872559,22.0094767659818));
#16976=CARTESIAN_POINT('Ctrl Pts',(1.7867159093031,2.68211928388161,22.0094541829101));
#16977=CARTESIAN_POINT('Ctrl Pts',(1.78686250086671,2.68202162491706,22.0094433449083));
#16978=CARTESIAN_POINT('Ctrl Pts',(1.78714542080856,2.68183311080744,22.0094224256734));
#16979=CARTESIAN_POINT('Ctrl Pts',(1.78728175025666,2.68174225729088,22.0094123445027));
#16980=CARTESIAN_POINT('Ctrl Pts',(1.7875457534526,2.68156628957007,22.0093928204693));
#16981=CARTESIAN_POINT('Ctrl Pts',(1.78767342806627,2.68148117663183,22.009383377654));
#16982=CARTESIAN_POINT('Ctrl Pts',(1.78792141284636,2.68131583460374,22.0093650351524));
#16983=CARTESIAN_POINT('Ctrl Pts',(1.78804172368694,2.68123560653776,22.0093561355053));
#16984=CARTESIAN_POINT('Ctrl Pts',(1.78827603459676,2.68107933589541,22.0093388016557));
#16985=CARTESIAN_POINT('Ctrl Pts',(1.78839003520651,2.68100329415175,22.0093303674852));
#16986=CARTESIAN_POINT('Ctrl Pts',(1.78861259754135,2.68085481804755,22.0093139002929));
#16987=CARTESIAN_POINT('Ctrl Pts',(1.78872115972714,2.68078238435662,22.0093058672959));
#16988=CARTESIAN_POINT('Ctrl Pts',(1.7889335758828,2.68064063969209,22.0092901485569));
#16989=CARTESIAN_POINT('Ctrl Pts',(1.78903743022243,2.68057132927904,22.0092824628363));
#16990=CARTESIAN_POINT('Ctrl Pts',(1.78924105001169,2.68043542019606,22.0092673929587));
#16991=CARTESIAN_POINT('Ctrl Pts',(1.78934081577337,2.68036882198999,22.0092600088193));
#16992=CARTESIAN_POINT('Ctrl Pts',(1.78953678895431,2.68023798511654,22.0092455029544));
#16993=CARTESIAN_POINT('Ctrl Pts',(1.78963299664239,2.6801737468327,22.0092383812429));
#16994=CARTESIAN_POINT('Ctrl Pts',(1.78982231271286,2.68004732494618,22.0092243663532));
#16995=CARTESIAN_POINT('Ctrl Pts',(1.78991542132132,2.67998514166629,22.0092174731868));
#16996=CARTESIAN_POINT('Ctrl Pts',(1.79009894011211,2.67986256344072,22.0092038857921));
#16997=CARTESIAN_POINT('Ctrl Pts',(1.79018935049083,2.67980216876373,22.0091971915734));
#16998=CARTESIAN_POINT('Ctrl Pts',(1.79036782611743,2.67968293290854,22.0091839759859));
#16999=CARTESIAN_POINT('Ctrl Pts',(1.79045589151262,2.67962409196991,22.0091774546265));
#17000=CARTESIAN_POINT('Ctrl Pts',(1.79062999123189,2.6795077547394,22.0091645615606));
#17001=CARTESIAN_POINT('Ctrl Pts',(1.79071602566652,2.67945025865919,22.0091581898631));
#17002=CARTESIAN_POINT('Ctrl Pts',(1.79099388431743,2.67926454872842,22.0091376105219));
#17003=CARTESIAN_POINT('Ctrl Pts',(1.79118569753948,2.67913631841781,22.0091234022527));
#17004=CARTESIAN_POINT('Ctrl Pts',(1.79156939066867,2.6788797535923,22.0090949771682));
#17005=CARTESIAN_POINT('Ctrl Pts',(1.79176127054781,2.67875141906682,22.0090807603532));
#17006=CARTESIAN_POINT('Ctrl Pts',(1.79214538799836,2.67849445104486,22.0090522966071));
#17007=CARTESIAN_POINT('Ctrl Pts',(1.79233762551632,2.67836581746414,22.0090380496727));
#17008=CARTESIAN_POINT('Ctrl Pts',(1.79272273506006,2.67810806570047,22.0090095051474));
#17009=CARTESIAN_POINT('Ctrl Pts',(1.79291560699319,2.67797894737269,22.0089952075509));
#17010=CARTESIAN_POINT('Ctrl Pts',(1.80340648599425,2.67095417552641,22.0082174193466));
#17011=CARTESIAN_POINT('Ctrl Pts',(1.81366452662376,2.66399927542424,22.0074516857675));
#17012=CARTESIAN_POINT('Ctrl Pts',(1.84539382376048,2.64221876609504,22.0050667876261));
#17013=CARTESIAN_POINT('Ctrl Pts',(1.86672490895186,2.62719173687639,22.0034399535533));
#17014=CARTESIAN_POINT('Ctrl Pts',(2.05440155226368,2.49154022336499,21.9889129138892));
#17015=CARTESIAN_POINT('Ctrl Pts',(2.20900862282055,2.35554484432636,21.9753926897263));
#17016=CARTESIAN_POINT('Ctrl Pts',(2.52132880371376,2.02286214952885,21.9446692896455));
#17017=CARTESIAN_POINT('Ctrl Pts',(2.67111581519442,1.82050118546984,21.9274017204445));
#17018=CARTESIAN_POINT('Ctrl Pts',(2.80647432485881,1.58438324492992,21.9100271370072));
#17019=CARTESIAN_POINT('Ctrl Pts',(2.81685238460383,1.56585794456482,21.9086815099155));
#17020=CARTESIAN_POINT('Ctrl Pts',(2.83114285715885,1.53974688552513,21.906810776752));
#17021=CARTESIAN_POINT('Ctrl Pts',(2.83520912492648,1.5322465764312,21.9062763821614));
#17022=CARTESIAN_POINT('Ctrl Pts',(2.84172308973391,1.52011672740408,21.9054170214908));
#17023=CARTESIAN_POINT('Ctrl Pts',(2.84418933805486,1.51549727610832,21.9050908866655));
#17024=CARTESIAN_POINT('Ctrl Pts',(2.84935108089058,1.50577199957431,21.9044067024821));
#17025=CARTESIAN_POINT('Ctrl Pts',(2.85204412901494,1.50066491389003,21.9040488156069));
#17026=CARTESIAN_POINT('Ctrl Pts',(2.85858644406345,1.48817687076824,21.9031770502427));
#17027=CARTESIAN_POINT('Ctrl Pts',(2.86242089972674,1.48078811897645,21.9026641065641));
#17028=CARTESIAN_POINT('Ctrl Pts',(2.87605793273143,1.45425951856528,21.900832327141));
#17029=CARTESIAN_POINT('Ctrl Pts',(2.88569777376022,1.43503602593669,21.8995233504325));
#17030=CARTESIAN_POINT('Ctrl Pts',(2.96660010267425,1.26959055024847,21.8884021931337));
#17031=CARTESIAN_POINT('Ctrl Pts',(3.02689960620394,1.11824370915806,21.8791827574043));
#17032=CARTESIAN_POINT('Ctrl Pts',(3.15335679161336,0.714368169763034,21.8554513473008));
#17033=CARTESIAN_POINT('Ctrl Pts',(3.20076165487119,0.45726867794257,21.8411029445533));
#17034=CARTESIAN_POINT('Ctrl Pts',(3.21956011058785,0.150742852665705,21.8229367508855));
#17035=CARTESIAN_POINT('Ctrl Pts',(3.22140363024258,0.104158682245796,21.8201506984579));
#17036=CARTESIAN_POINT('Ctrl Pts',(3.22246428113639,0.0447753340969706,
21.8165606977749));
#17037=CARTESIAN_POINT('Ctrl Pts',(3.22261649317016,0.0319969438730099,
21.8157859246616));
#17038=CARTESIAN_POINT('Ctrl Pts',(3.22273083041161,0.0128237021512873,
21.8146199070751));
#17039=CARTESIAN_POINT('Ctrl Pts',(3.22274993082051,0.00642922219497983,
21.8142304413701));
#17040=CARTESIAN_POINT('Ctrl Pts',(3.22274999981242,3.47713463869469E-5,
21.8138403813771));
#17041=CARTESIAN_POINT('Ctrl Pts',(-1.47286814312172,-2.86060451358776,
21.4037167033623));
#17042=CARTESIAN_POINT('Ctrl Pts',(-0.960639331001378,-3.1231473602644,
21.4391135850969));
#17043=CARTESIAN_POINT('Ctrl Pts',(0.704518003503453,-3.50470367487752,
21.5408214462859));
#17044=CARTESIAN_POINT('Ctrl Pts',(2.81881824515291,-2.1837009951111,21.6765070282561));
#17045=CARTESIAN_POINT('Ctrl Pts',(3.21708968004072,-0.552330809057621,
21.7767957284918));
#17046=CARTESIAN_POINT('Ctrl Pts',(3.2174269477886,0.000221517408381389,
21.8107734492731));
#17047=CARTESIAN_POINT('',(3.22274864473311,-0.00295556608512274,21.5646308008574));
#17048=CARTESIAN_POINT('Ctrl Pts',(-1.47525512068015,-2.86526436675693,
21.1585511949183));
#17049=CARTESIAN_POINT('Ctrl Pts',(-1.33950807638485,-2.93515722709376,
21.1671466307572));
#17050=CARTESIAN_POINT('Ctrl Pts',(-1.19884492489093,-2.99537723415258,
21.1755968604717));
#17051=CARTESIAN_POINT('Ctrl Pts',(-0.899465629869808,-3.09902033723927,
21.1934919964054));
#17052=CARTESIAN_POINT('Ctrl Pts',(-0.740786060354651,-3.14073097250001,
21.2029340534885));
#17053=CARTESIAN_POINT('Ctrl Pts',(-0.558089735586257,-3.17413502792007,
21.2141048776658));
#17054=CARTESIAN_POINT('Ctrl Pts',(-0.536504182726207,-3.17785470940248,
21.2154290499623));
#17055=CARTESIAN_POINT('Ctrl Pts',(-0.501958106984388,-3.18344578158891,
21.2175559122077));
#17056=CARTESIAN_POINT('Ctrl Pts',(-0.489020949228741,-3.18545875640527,
21.2183541012963));
#17057=CARTESIAN_POINT('Ctrl Pts',(-0.466103564706559,-3.18888171882243,
21.2197711951427));
#17058=CARTESIAN_POINT('Ctrl Pts',(-0.456128258359685,-3.19032383276872,
21.2203890709369));
#17059=CARTESIAN_POINT('Ctrl Pts',(-0.435402827530088,-3.19322088506343,
21.2216750710259));
#17060=CARTESIAN_POINT('Ctrl Pts',(-0.424651807406015,-3.19466838355501,
21.222343422996));
#17061=CARTESIAN_POINT('Ctrl Pts',(-0.39686473737466,-3.19826684230201,
21.2240741875394));
#17062=CARTESIAN_POINT('Ctrl Pts',(-0.379818605891042,-3.20033595464038,
21.225139176916));
#17063=CARTESIAN_POINT('Ctrl Pts',(-0.308115007466941,-3.20845862817185,
21.2296331346792));
#17064=CARTESIAN_POINT('Ctrl Pts',(-0.253326450116323,-3.21324862636154,
21.233101655442));
#17065=CARTESIAN_POINT('Ctrl Pts',(-0.108743703005732,-3.22216841205644,
21.2423517675451));
#17066=CARTESIAN_POINT('Ctrl Pts',(-0.0188576932707636,-3.22394734568775,
21.248201726647));
#17067=CARTESIAN_POINT('Ctrl Pts',(0.32913764104249,-3.21628111846667,21.2712055080523));
#17068=CARTESIAN_POINT('Ctrl Pts',(0.585647945511776,-3.17959032228132,
21.289011533561));
#17069=CARTESIAN_POINT('Ctrl Pts',(0.838613857033333,-3.11172913699444,
21.3063582333857));
#17070=CARTESIAN_POINT('Ctrl Pts',(0.842208054769976,-3.11075827024362,
21.3066046337369));
#17071=CARTESIAN_POINT('Ctrl Pts',(0.920165065851668,-3.08955546496622,
21.3119474498516));
#17072=CARTESIAN_POINT('Ctrl Pts',(0.993787133678537,-3.06666691940676,
21.316963441133));
#17073=CARTESIAN_POINT('Ctrl Pts',(1.07800331495973,-3.03713259557178,21.3226122754996));
#17074=CARTESIAN_POINT('Ctrl Pts',(1.08946019955861,-3.03304171331183,21.3233788028289));
#17075=CARTESIAN_POINT('Ctrl Pts',(1.1077345490467,-3.02639962800358,21.3245980238515));
#17076=CARTESIAN_POINT('Ctrl Pts',(1.11456687938823,-3.02389007957721,21.3250530905193));
#17077=CARTESIAN_POINT('Ctrl Pts',(1.12665525077406,-3.01940342477296,21.3258567945723));
#17078=CARTESIAN_POINT('Ctrl Pts',(1.13191469660646,-3.01743570223392,21.3262059853068));
#17079=CARTESIAN_POINT('Ctrl Pts',(1.14306127972063,-3.01323217303237,21.3269449841012));
#17080=CARTESIAN_POINT('Ctrl Pts',(1.14894700354903,-3.01099285991152,21.3273345782617));
#17081=CARTESIAN_POINT('Ctrl Pts',(1.16464103778939,-3.00496910775478,21.3283718565764));
#17082=CARTESIAN_POINT('Ctrl Pts',(1.17443755662519,-3.00115386446673,21.329017717207));
#17083=CARTESIAN_POINT('Ctrl Pts',(1.2221666206223,-2.98229633681415,21.3321572309124));
#17084=CARTESIAN_POINT('Ctrl Pts',(1.25983171720971,-2.96658171880922,21.3346126650525));
#17085=CARTESIAN_POINT('Ctrl Pts',(1.36720005157037,-2.91937160855032,21.3415761941654));
#17086=CARTESIAN_POINT('Ctrl Pts',(1.43609691118943,-2.88610357271859,21.3460005577997));
#17087=CARTESIAN_POINT('Ctrl Pts',(1.65816342658134,-2.76895132924326,21.3603187328803));
#17088=CARTESIAN_POINT('Ctrl Pts',(1.80570754010328,-2.67507424181031,21.3699390637197));
#17089=CARTESIAN_POINT('Ctrl Pts',(2.09125523990477,-2.45895253000787,21.3900784150237));
#17090=CARTESIAN_POINT('Ctrl Pts',(2.22783781776974,-2.33591979532386,21.4005880111145));
#17091=CARTESIAN_POINT('Ctrl Pts',(2.36837593722782,-2.18572785803136,21.4129564952059));
#17092=CARTESIAN_POINT('Ctrl Pts',(2.38338261920232,-2.16935430533993,21.4142989408526));
#17093=CARTESIAN_POINT('Ctrl Pts',(2.40702432127102,-2.14301778947604,21.4164495998106));
#17094=CARTESIAN_POINT('Ctrl Pts',(2.41576968775737,-2.1331545037367,21.4172531498078));
#17095=CARTESIAN_POINT('Ctrl Pts',(2.43110390863767,-2.11564487131514,21.4186764612445));
#17096=CARTESIAN_POINT('Ctrl Pts',(2.43771785326446,-2.10802065936518,21.419295163645));
#17097=CARTESIAN_POINT('Ctrl Pts',(2.45134110985849,-2.09216662447021,21.420579618525));
#17098=CARTESIAN_POINT('Ctrl Pts',(2.45834503832784,-2.08393236200208,21.4212455824865));
#17099=CARTESIAN_POINT('Ctrl Pts',(2.47625568841935,-2.06265951807285,21.4229632053543));
#17100=CARTESIAN_POINT('Ctrl Pts',(2.48710081044941,-2.04956972624567,21.4240173672019));
#17101=CARTESIAN_POINT('Ctrl Pts',(2.53147277884801,-1.99514307719448,21.4283897737));
#17102=CARTESIAN_POINT('Ctrl Pts',(2.56407504241998,-1.95306655282825,21.4317448886286));
#17103=CARTESIAN_POINT('Ctrl Pts',(2.6768404675664,-1.79983889683936,21.4438823209671));
#17104=CARTESIAN_POINT('Ctrl Pts',(2.75093057672508,-1.68441916529371,21.4528859333923));
#17105=CARTESIAN_POINT('Ctrl Pts',(2.87096507175701,-1.46827427041668,21.4694296951672));
#17106=CARTESIAN_POINT('Ctrl Pts',(2.91950367172001,-1.36922117344101,21.4768991879181));
#17107=CARTESIAN_POINT('Ctrl Pts',(3.03429855343958,-1.10096044481153,21.4966461558731));
#17108=CARTESIAN_POINT('Ctrl Pts',(3.09150258183659,-0.92828287185256,21.508884305806));
#17109=CARTESIAN_POINT('Ctrl Pts',(3.13730125473036,-0.737343887368482,
21.5213310729406));
#17110=CARTESIAN_POINT('Ctrl Pts',(3.14064352229288,-0.722975419068099,
21.5222611186853));
#17111=CARTESIAN_POINT('Ctrl Pts',(3.14545813538205,-0.701613666799873,
21.5236335390728));
#17112=CARTESIAN_POINT('Ctrl Pts',(3.14700601629606,-0.694637858609409,
21.5240800875861));
#17113=CARTESIAN_POINT('Ctrl Pts',(3.14972282611667,-0.682198574760167,
21.524873412208));
#17114=CARTESIAN_POINT('Ctrl Pts',(3.15090075822329,-0.676737164818766,
21.525220698444));
#17115=CARTESIAN_POINT('Ctrl Pts',(3.15340886380438,-0.664959966208358,
21.5259673920913));
#17116=CARTESIAN_POINT('Ctrl Pts',(3.15473426512354,-0.658643254852206,
21.5263665242143));
#17117=CARTESIAN_POINT('Ctrl Pts',(3.15742019752989,-0.645648284617995,
21.527184923401));
#17118=CARTESIAN_POINT('Ctrl Pts',(3.15877853968128,-0.638969600537329,
21.5276040657581));
#17119=CARTESIAN_POINT('Ctrl Pts',(3.16217827962945,-0.621977983445314,
21.5286668132887));
#17120=CARTESIAN_POINT('Ctrl Pts',(3.16419043798832,-0.611659188647948,
21.5293088245528));
#17121=CARTESIAN_POINT('Ctrl Pts',(3.20361203272885,-0.404094879550618,
21.5421584531868));
#17122=CARTESIAN_POINT('Ctrl Pts',(3.22256448354999,-0.203764881871651,
21.5534055260314));
#17123=CARTESIAN_POINT('Ctrl Pts',(3.22274864473311,-0.00295556608512274,
21.5646308008574));
#17124=CARTESIAN_POINT('Ctrl Pts',(3.22274864368595,-0.00295670769533594,
21.5646307370412));
#17125=CARTESIAN_POINT('Ctrl Pts',(3.22295282629112,0.219597998984461,21.5770715831944));
#17126=CARTESIAN_POINT('Ctrl Pts',(3.20010444854947,0.441562064382687,21.5894492096769));
#17127=CARTESIAN_POINT('Ctrl Pts',(3.14673634528828,0.69687401531595,21.6048156091233));
#17128=CARTESIAN_POINT('Ctrl Pts',(3.13823688387506,0.734201676282312,21.6070896830952));
#17129=CARTESIAN_POINT('Ctrl Pts',(3.12429679400706,0.790750022564981,21.6105811709925));
#17130=CARTESIAN_POINT('Ctrl Pts',(3.11933890778647,0.810086912924945,21.6117834248368));
#17131=CARTESIAN_POINT('Ctrl Pts',(3.10979440434312,0.845925306397751,21.614027806844));
#17132=CARTESIAN_POINT('Ctrl Pts',(3.10525525136024,0.86243879062455,21.6150683829872));
#17133=CARTESIAN_POINT('Ctrl Pts',(3.09762897389315,0.889342322691042,21.616774491472));
#17134=CARTESIAN_POINT('Ctrl Pts',(3.09462063337281,0.899754498625532,21.6174374463735));
#17135=CARTESIAN_POINT('Ctrl Pts',(3.08871236438747,0.919823435719477,21.6187204808833));
#17136=CARTESIAN_POINT('Ctrl Pts',(3.08581952256584,0.929482164047732,21.6193403217328));
#17137=CARTESIAN_POINT('Ctrl Pts',(3.07905938034888,0.951673747629037,21.6207699237972));
#17138=CARTESIAN_POINT('Ctrl Pts',(3.07516081999333,0.964196822564485,21.6215807050466));
#17139=CARTESIAN_POINT('Ctrl Pts',(3.06452385157253,0.997644406488598,21.623757177833));
#17140=CARTESIAN_POINT('Ctrl Pts',(3.05764770551607,1.01852406399257,21.6251273900306));
#17141=CARTESIAN_POINT('Ctrl Pts',(2.97678679442496,1.25586026475295,21.6408371547048));
#17142=CARTESIAN_POINT('Ctrl Pts',(2.88018608059178,1.46387664779887,21.6559615330626));
#17143=CARTESIAN_POINT('Ctrl Pts',(2.70765625881592,1.75100442390043,21.6785803442124));
#17144=CARTESIAN_POINT('Ctrl Pts',(2.64842710458284,1.83936209436748,21.6858011659358));
#17145=CARTESIAN_POINT('Ctrl Pts',(2.51373232281548,2.02026837872625,21.700979927261));
#17146=CARTESIAN_POINT('Ctrl Pts',(2.43726475125761,2.11189033486796,21.7089097039046));
#17147=CARTESIAN_POINT('Ctrl Pts',(2.33895678800487,2.21720868162038,21.7181355393821));
#17148=CARTESIAN_POINT('Ctrl Pts',(2.32181664457092,2.23515116972683,21.7197113277131));
#17149=CARTESIAN_POINT('Ctrl Pts',(2.29973084143584,2.25774258635489,21.7216985157936));
#17150=CARTESIAN_POINT('Ctrl Pts',(2.29497596244741,2.26257571432059,21.7221238319612));
#17151=CARTESIAN_POINT('Ctrl Pts',(2.28568246253389,2.27196271496768,21.7229501835752));
#17152=CARTESIAN_POINT('Ctrl Pts',(2.28114539962296,2.27651807926786,21.7233513350811));
#17153=CARTESIAN_POINT('Ctrl Pts',(2.27263773403242,2.2850090910286,21.7240992656313));
#17154=CARTESIAN_POINT('Ctrl Pts',(2.26867056720638,2.2889479405013,21.7244462939011));
#17155=CARTESIAN_POINT('Ctrl Pts',(2.25958292584611,2.29792387884901,21.7252373095417));
#17156=CARTESIAN_POINT('Ctrl Pts',(2.25445585761577,2.30295417674287,21.7256807614283));
#17157=CARTESIAN_POINT('Ctrl Pts',(2.23861198667107,2.31839538667485,21.7270426298571));
#17158=CARTESIAN_POINT('Ctrl Pts',(2.22783938872911,2.32874912212685,21.7279566866643));
#17159=CARTESIAN_POINT('Ctrl Pts',(2.1205391453096,2.4304512467272,21.7369488467762));
#17160=CARTESIAN_POINT('Ctrl Pts',(2.01850774736131,2.51583284858812,21.7446097803966));
#17161=CARTESIAN_POINT('Ctrl Pts',(1.73102869093033,2.72761684924705,21.7648130241963));
#17162=CARTESIAN_POINT('Ctrl Pts',(1.53720297659449,2.84136638498967,21.7770803494871));
#17163=CARTESIAN_POINT('Ctrl Pts',(1.22818359270064,2.98177341482338,21.7965542219053));
#17164=CARTESIAN_POINT('Ctrl Pts',(1.12075412501294,3.02379124447066,21.8033010148054));
#17165=CARTESIAN_POINT('Ctrl Pts',(0.990978726205584,3.06668181516498,21.8115360485272));
#17166=CARTESIAN_POINT('Ctrl Pts',(0.970578767855779,3.07319914951331,21.8128328261443));
#17167=CARTESIAN_POINT('Ctrl Pts',(0.93849983260424,3.08309639808588,21.8148761928178));
#17168=CARTESIAN_POINT('Ctrl Pts',(0.926863867253536,3.0866144399477,21.8156182376361));
#17169=CARTESIAN_POINT('Ctrl Pts',(0.905666518172883,3.09289261932481,21.8169716976677));
#17170=CARTESIAN_POINT('Ctrl Pts',(0.896111683248289,3.09567447326493,21.817582392299));
#17171=CARTESIAN_POINT('Ctrl Pts',(0.875464235851754,3.10158229790063,21.8189034597646));
#17172=CARTESIAN_POINT('Ctrl Pts',(0.86436746181194,3.10469310308352,21.8196143186824));
#17173=CARTESIAN_POINT('Ctrl Pts',(0.834248176430598,3.112962577351,21.821546214587));
#17174=CARTESIAN_POINT('Ctrl Pts',(0.815194877462533,3.11800630399879,21.8227709705366));
#17175=CARTESIAN_POINT('Ctrl Pts',(0.72226220243879,3.14169710593575,21.8287584645775));
#17176=CARTESIAN_POINT('Ctrl Pts',(0.647788816692424,3.15789351661783,21.8335995835933));
#17177=CARTESIAN_POINT('Ctrl Pts',(0.541870914711993,3.17702413104094,21.8405499499866));
#17178=CARTESIAN_POINT('Ctrl Pts',(0.510846240653213,3.18216002648297,21.8425934826073));
#17179=CARTESIAN_POINT('Ctrl Pts',(0.228988224158424,3.22459138493855,21.8612258034302));
#17180=CARTESIAN_POINT('Ctrl Pts',(-0.0253405976808572,3.23260809533602,
21.8786177615519));
#17181=CARTESIAN_POINT('Ctrl Pts',(-0.357675158241974,3.20384033930764,
21.9009738786876));
#17182=CARTESIAN_POINT('Ctrl Pts',(-0.4371408368981,3.19396839345557,21.9062822783302));
#17183=CARTESIAN_POINT('Ctrl Pts',(-0.557680685416124,3.17441003154079,
21.9142028767085));
#17184=CARTESIAN_POINT('Ctrl Pts',(-0.599066495246496,3.16686067466407,
21.9168982172272));
#17185=CARTESIAN_POINT('Ctrl Pts',(-0.650813328018528,3.15637050398897,
21.9202281266089));
#17186=CARTESIAN_POINT('Ctrl Pts',(-0.661321207210347,3.15418563419551,
21.9209022132087));
#17187=CARTESIAN_POINT('Ctrl Pts',(-0.67797790443711,3.15063536289355,21.9219672077881));
#17188=CARTESIAN_POINT('Ctrl Pts',(-0.684133860205735,3.14930438220198,
21.9223600372643));
#17189=CARTESIAN_POINT('Ctrl Pts',(-0.695770929613101,3.14675259716486,
21.9231011241821));
#17190=CARTESIAN_POINT('Ctrl Pts',(-0.701252684778172,3.14553552941198,
21.923449579583));
#17191=CARTESIAN_POINT('Ctrl Pts',(-0.713831201254937,3.14270831179557,
21.924247716182));
#17192=CARTESIAN_POINT('Ctrl Pts',(-0.720925705135605,3.14108844941254,
21.924696833898));
#17193=CARTESIAN_POINT('Ctrl Pts',(-0.739860132272624,3.13669769114947,
21.925892832266));
#17194=CARTESIAN_POINT('Ctrl Pts',(-0.751690096958051,3.13388376139916,
21.9266373072449));
#17195=CARTESIAN_POINT('Ctrl Pts',(-0.838251190800964,3.11277558950185,
21.9320662977008));
#17196=CARTESIAN_POINT('Ctrl Pts',(-0.912328405000588,3.09187579131151,
21.9366117456639));
#17197=CARTESIAN_POINT('Ctrl Pts',(-1.01944935674911,3.05746710897152,21.9431311272733));
#17198=CARTESIAN_POINT('Ctrl Pts',(-1.05312470906741,3.04603194245208,21.9451726580142));
#17199=CARTESIAN_POINT('Ctrl Pts',(-1.29679423462334,2.95876468941543,21.9599315535288));
#17200=CARTESIAN_POINT('Ctrl Pts',(-1.49859496734826,2.86184968974938,21.9721255693895));
#17201=CARTESIAN_POINT('Ctrl Pts',(-1.7670368015759,2.6966913951922,21.9900692075541));
#17202=CARTESIAN_POINT('Ctrl Pts',(-1.84320972511707,2.64521067585503,21.9953738345733));
#17203=CARTESIAN_POINT('Ctrl Pts',(-1.96215709237816,2.55718644597886,22.0040995425003));
#17204=CARTESIAN_POINT('Ctrl Pts',(-2.00635836832358,2.52265504906626,22.0074471593772));
#17205=CARTESIAN_POINT('Ctrl Pts',(-2.06288515274036,2.47606891137863,22.0118797377743));
#17206=CARTESIAN_POINT('Ctrl Pts',(-2.07604831800045,2.46504275234092,22.0129230182015));
#17207=CARTESIAN_POINT('Ctrl Pts',(-2.09738259994558,2.44687994628014,22.0146324442743));
#17208=CARTESIAN_POINT('Ctrl Pts',(-2.10560701442335,2.43980620917381,22.0152959930562));
#17209=CARTESIAN_POINT('Ctrl Pts',(-2.12140365397103,2.42608031336815,22.0165793922412));
#17210=CARTESIAN_POINT('Ctrl Pts',(-2.1289807040943,2.4194338816973,22.0171989996714));
#17211=CARTESIAN_POINT('Ctrl Pts',(-2.14632859348215,2.40407207815753,22.018626937528));
#17212=CARTESIAN_POINT('Ctrl Pts',(-2.156077698355,2.39533253196708,22.019436280278));
#17213=CARTESIAN_POINT('Ctrl Pts',(-2.18199361258413,2.37181390900654,22.0216063841181));
#17214=CARTESIAN_POINT('Ctrl Pts',(-2.19806323658842,2.35692921277075,22.0229716244587));
#17215=CARTESIAN_POINT('Ctrl Pts',(-2.33307114566668,2.22929480060283,22.0346115595203));
#17216=CARTESIAN_POINT('Ctrl Pts',(-2.44338256528359,2.10780531015908,22.0452736337356));
#17217=CARTESIAN_POINT('Ctrl Pts',(-2.69985356445187,1.77802891565876,22.0731374537039));
#17218=CARTESIAN_POINT('Ctrl Pts',(-2.83149784131443,1.55987539728716,22.0906649940966));
#17219=CARTESIAN_POINT('Ctrl Pts',(-2.95941181492372,1.27717557502508,22.1109648388526));
#17220=CARTESIAN_POINT('Ctrl Pts',(-2.98130184259496,1.22520854647347,22.1146004542298));
#17221=CARTESIAN_POINT('Ctrl Pts',(-3.00606652050387,1.1618166462215,22.118898230362));
#17222=CARTESIAN_POINT('Ctrl Pts',(-3.0102554097266,1.15091972925438,22.1196321841571));
#17223=CARTESIAN_POINT('Ctrl Pts',(-3.01668630368315,1.13391517742121,22.1207697475211));
#17224=CARTESIAN_POINT('Ctrl Pts',(-3.01896913263,1.12782324076915,22.1211757380117));
#17225=CARTESIAN_POINT('Ctrl Pts',(-3.02317605894916,1.11649237628293,22.1219279472487));
#17226=CARTESIAN_POINT('Ctrl Pts',(-3.02510497612679,1.11125541340866,22.1222744442827));
#17227=CARTESIAN_POINT('Ctrl Pts',(-3.02944757651277,1.09937025869898,22.1230581985766));
#17228=CARTESIAN_POINT('Ctrl Pts',(-3.03185297887558,1.09271913193039,22.1234949584975));
#17229=CARTESIAN_POINT('Ctrl Pts',(-3.03892694265621,1.07295587966443,22.1247874445107));
#17230=CARTESIAN_POINT('Ctrl Pts',(-3.0435325500688,1.05982117141884,22.1256395155764));
#17231=CARTESIAN_POINT('Ctrl Pts',(-3.07785030995952,0.959881673521503,
22.1320733059404));
#17232=CARTESIAN_POINT('Ctrl Pts',(-3.10393147585281,0.871864739967578,
22.1374575030244));
#17233=CARTESIAN_POINT('Ctrl Pts',(-3.18528373571642,0.546992208606677,
22.1567145906095));
#17234=CARTESIAN_POINT('Ctrl Pts',(-3.21746735844233,0.305204731909847,
22.1699314351238));
#17235=CARTESIAN_POINT('Ctrl Pts',(-3.22392200778803,-0.0297789318281736,
22.1890062553779));
#17236=CARTESIAN_POINT('Ctrl Pts',(-3.22176255867939,-0.121671627717367,
22.194309786876));
#17237=CARTESIAN_POINT('Ctrl Pts',(-3.21196866190613,-0.269294113501907,
22.2030338572505));
#17238=CARTESIAN_POINT('Ctrl Pts',(-3.20679703277196,-0.325137231871912,
22.2063809681983));
#17239=CARTESIAN_POINT('Ctrl Pts',(-3.19814263192213,-0.397864399675196,
22.2108129698619));
#17240=CARTESIAN_POINT('Ctrl Pts',(-3.195977543996,-0.414897451391854,22.2118561932592));
#17241=CARTESIAN_POINT('Ctrl Pts',(-3.1922226605767,-0.442662086495636,
22.2135655493634));
#17242=CARTESIAN_POINT('Ctrl Pts',(-3.19071458648495,-0.453404521991138,
22.2142290856169));
#17243=CARTESIAN_POINT('Ctrl Pts',(-3.18770072665389,-0.474113097061738,
22.2155124770625));
#17244=CARTESIAN_POINT('Ctrl Pts',(-3.18620236428957,-0.484080201647737,
22.2161320893705));
#17245=CARTESIAN_POINT('Ctrl Pts',(-3.18265008980904,-0.506978704304749,
22.2175600621141));
#17246=CARTESIAN_POINT('Ctrl Pts',(-3.18056408718891,-0.519904875848573,
22.2183694350351));
#17247=CARTESIAN_POINT('Ctrl Pts',(-3.17477774499518,-0.554421939029222,
22.2205396723911));
#17248=CARTESIAN_POINT('Ctrl Pts',(-3.17093599157242,-0.575988121122701,
22.221905016943));
#17249=CARTESIAN_POINT('Ctrl Pts',(-3.13647413144644,-0.758639188682412,
22.2335502534206));
#17250=CARTESIAN_POINT('Ctrl Pts',(-3.09382621544345,-0.9171848398229,22.2442179330315));
#17251=CARTESIAN_POINT('Ctrl Pts',(-2.9548060603783,-1.31141319276203,22.2720993486826));
#17252=CARTESIAN_POINT('Ctrl Pts',(-2.84226314543941,-1.54020091533875,
22.2896392452633));
#17253=CARTESIAN_POINT('Ctrl Pts',(-2.67347616072602,-1.80049849873391,
22.3099325313362));
#17254=CARTESIAN_POINT('Ctrl Pts',(-2.64170245852142,-1.84680227835355,
22.3135528176121));
#17255=CARTESIAN_POINT('Ctrl Pts',(-2.60188667582506,-1.90169378285213,
22.3178349670948));
#17256=CARTESIAN_POINT('Ctrl Pts',(-2.59498915959727,-1.91109518050673,
22.3185680279477));
#17257=CARTESIAN_POINT('Ctrl Pts',(-2.58416578109671,-1.92568093421766,
22.3197045113805));
#17258=CARTESIAN_POINT('Ctrl Pts',(-2.5802750789569,-1.93089108012031,22.3201103077295));
#17259=CARTESIAN_POINT('Ctrl Pts',(-2.57301559457092,-1.94055132975122,
22.3208623416454));
#17260=CARTESIAN_POINT('Ctrl Pts',(-2.56965105406861,-1.94500441499229,
22.3212088563431));
#17261=CARTESIAN_POINT('Ctrl Pts',(-2.56199409194724,-1.95508412013192,
22.3219928853447));
#17262=CARTESIAN_POINT('Ctrl Pts',(-2.557694705479,-1.96070534241777,22.3224299008504));
#17263=CARTESIAN_POINT('Ctrl Pts',(-2.54487271110028,-1.97735548534706,
22.3237238450113));
#17264=CARTESIAN_POINT('Ctrl Pts',(-2.53629690409943,-1.98834349690016,
22.3245771063966));
#17265=CARTESIAN_POINT('Ctrl Pts',(-2.47036674278148,-2.07169786429477,
22.3310478300525));
#17266=CARTESIAN_POINT('Ctrl Pts',(-2.40999153727165,-2.14163211295888,
22.3364651978303));
#17267=CARTESIAN_POINT('Ctrl Pts',(-2.180546989088,-2.38539117508947,22.355708484335));
#17268=CARTESIAN_POINT('Ctrl Pts',(-1.99501578242429,-2.54259732980843,
22.3688876917867));
#17269=CARTESIAN_POINT('Ctrl Pts',(-1.71720405350204,-2.72869629653299,
22.3879241436484));
#17270=CARTESIAN_POINT('Ctrl Pts',(-1.63865613057525,-2.7765765601685,22.3932316875754));
#17271=CARTESIAN_POINT('Ctrl Pts',(-1.53074825105566,-2.83617857605774,
22.4005007344283));
#17272=CARTESIAN_POINT('Ctrl Pts',(-1.50310616526436,-2.85092453600792,
22.4023607307207));
#17273=CARTESIAN_POINT('Ctrl Pts',(-1.47525540254685,-2.86526422163059,
22.4042343665403));
#17274=CARTESIAN_POINT('Origin',(0.,0.,4.68922655072688));
#17275=CARTESIAN_POINT('',(-1.47525540579296,-2.86526421995924,23.9007338658376));
#17276=CARTESIAN_POINT('',(-1.47525500221108,-2.86526442775378,23.6562919783988));
#17277=CARTESIAN_POINT('',(-1.47525540501186,-2.86526422036142,4.68922655072688));
#17278=CARTESIAN_POINT('Ctrl Pts',(-1.47525540579296,-2.86526421995924,
23.9007338658376));
#17279=CARTESIAN_POINT('Ctrl Pts',(-1.48875271027542,-2.85831478358173,
23.8997646385843));
#17280=CARTESIAN_POINT('Ctrl Pts',(-1.50220145552381,-2.85126969437684,
23.8988004124447));
#17281=CARTESIAN_POINT('Ctrl Pts',(-1.52589489557367,-2.83864375982311,
23.897105029872));
#17282=CARTESIAN_POINT('Ctrl Pts',(-1.53615950369407,-2.83310211897691,
23.8963716693393));
#17283=CARTESIAN_POINT('Ctrl Pts',(-1.55210108942648,-2.82438348745219,
23.8952347368373));
#17284=CARTESIAN_POINT('Ctrl Pts',(-1.55779879517731,-2.82124490101643,
23.894828789153));
#17285=CARTESIAN_POINT('Ctrl Pts',(-1.56836922331773,-2.81538038542728,
23.8940764818429));
#17286=CARTESIAN_POINT('Ctrl Pts',(-1.57324431774014,-2.81265907153875,
23.893729844854));
#17287=CARTESIAN_POINT('Ctrl Pts',(-1.58428490758782,-2.80645844629098,
23.8929455404901));
#17288=CARTESIAN_POINT('Ctrl Pts',(-1.59044601114441,-2.80297148880649,
23.892508372258));
#17289=CARTESIAN_POINT('Ctrl Pts',(-1.60870730267693,-2.79255667502932,
23.891213974424));
#17290=CARTESIAN_POINT('Ctrl Pts',(-1.62077426029396,-2.78557045906161,
23.8903604146455));
#17291=CARTESIAN_POINT('Ctrl Pts',(-1.71243620091211,-2.73170509875028,
23.8838872560959));
#17292=CARTESIAN_POINT('Ctrl Pts',(-1.79003590821606,-2.68149685281321,
23.8784678993994));
#17293=CARTESIAN_POINT('Ctrl Pts',(-2.0630153805818,-2.48773493809652,23.859225156025));
#17294=CARTESIAN_POINT('Ctrl Pts',(-2.24420385971488,-2.32560089572219,
23.8460479142645));
#17295=CARTESIAN_POINT('Ctrl Pts',(-2.46669661789865,-2.07604890384023,
23.8270142340914));
#17296=CARTESIAN_POINT('Ctrl Pts',(-2.52491456150852,-2.00483809378753,
23.8217073091781));
#17297=CARTESIAN_POINT('Ctrl Pts',(-2.6136276653639,-1.88632338112434,23.8129779418232));
#17298=CARTESIAN_POINT('Ctrl Pts',(-2.64606908504447,-1.84053885911269,
23.8096290323431));
#17299=CARTESIAN_POINT('Ctrl Pts',(-2.6868592157698,-1.7796629384393,23.8051947559183));
#17300=CARTESIAN_POINT('Ctrl Pts',(-2.69630647563498,-1.76531696629811,
23.8041511034358));
#17301=CARTESIAN_POINT('Ctrl Pts',(-2.71153419442991,-1.7417857611663,23.8024410694734));
#17302=CARTESIAN_POINT('Ctrl Pts',(-2.71738381780613,-1.73264552275831,
23.8017772867525));
#17303=CARTESIAN_POINT('Ctrl Pts',(-2.72857912661839,-1.71495631756338,
23.8004934355404));
#17304=CARTESIAN_POINT('Ctrl Pts',(-2.73393108272204,-1.70641145466359,
23.7998736102047));
#17305=CARTESIAN_POINT('Ctrl Pts',(-2.74614298890772,-1.68670916070973,
23.7984451695837));
#17306=CARTESIAN_POINT('Ctrl Pts',(-2.75297516010459,-1.6755348006101,23.7976355412705));
#17307=CARTESIAN_POINT('Ctrl Pts',(-2.7710547481496,-1.64555561019883,23.7954646653593));
#17308=CARTESIAN_POINT('Ctrl Pts',(-2.78217866129356,-1.62667745476488,
23.7940989353455));
#17309=CARTESIAN_POINT('Ctrl Pts',(-2.87493272628677,-1.46553159785942,
23.7824498804748));
#17310=CARTESIAN_POINT('Ctrl Pts',(-2.94577183589392,-1.31735895194564,
23.771778508006));
#17311=CARTESIAN_POINT('Ctrl Pts',(-3.09699272308924,-0.927116093120989,
23.7438635566282));
#17312=CARTESIAN_POINT('Ctrl Pts',(-3.1605184295348,-0.679725471421503,
23.7262919199643));
#17313=CARTESIAN_POINT('Ctrl Pts',(-3.20166293237947,-0.372253308075372,
23.7060050770208));
#17314=CARTESIAN_POINT('Ctrl Pts',(-3.20761717592135,-0.316876945858572,
23.7024152314184));
#17315=CARTESIAN_POINT('Ctrl Pts',(-3.21307732194036,-0.249773999825745,
23.6981639540094));
#17316=CARTESIAN_POINT('Ctrl Pts',(-3.2139581249819,-0.238172434101687,
23.697432503885));
#17317=CARTESIAN_POINT('Ctrl Pts',(-3.21523294183536,-0.220083894300012,
23.6962978821074));
#17318=CARTESIAN_POINT('Ctrl Pts',(-3.21567018579925,-0.213600207691208,
23.6958923500173));
#17319=CARTESIAN_POINT('Ctrl Pts',(-3.21644668269606,-0.201542751211144,
23.6951404170441));
#17320=CARTESIAN_POINT('Ctrl Pts',(-3.21679105756146,-0.195969476926079,
23.6947937412779));
#17321=CARTESIAN_POINT('Ctrl Pts',(-3.21753972307367,-0.183319223632285,
23.6940088444651));
#17322=CARTESIAN_POINT('Ctrl Pts',(-3.21793515095062,-0.176241805068105,
23.6935711257052));
#17323=CARTESIAN_POINT('Ctrl Pts',(-3.21904132884225,-0.155196901350837,
23.6922735843386));
#17324=CARTESIAN_POINT('Ctrl Pts',(-3.21968452484479,-0.141225818795976,
23.6914174580281));
#17325=CARTESIAN_POINT('Ctrl Pts',(-3.22393620534607,-0.0336317711185114,
23.6848618100823));
#17326=CARTESIAN_POINT('Ctrl Pts',(-3.22355171424692,0.060113775093909,
23.6793683455703));
#17327=CARTESIAN_POINT('Ctrl Pts',(-3.20759897087588,0.394187455297721,
23.6601550106887));
#17328=CARTESIAN_POINT('Ctrl Pts',(-3.16920797392257,0.632620013166034,
23.6470608257321));
#17329=CARTESIAN_POINT('Ctrl Pts',(-3.07991139420277,0.953280937335598,
23.6281122548646));
#17330=CARTESIAN_POINT('Ctrl Pts',(-3.05141588401044,1.04089284080986,23.6227970742574));
#17331=CARTESIAN_POINT('Ctrl Pts',(-2.99956384621368,1.17978367425377,23.6140553680762));
#17332=CARTESIAN_POINT('Ctrl Pts',(-2.97854638125127,1.23188216228027,23.6107026479809));
#17333=CARTESIAN_POINT('Ctrl Pts',(-2.94933581202357,1.29916555280818,23.6062640278208));
#17334=CARTESIAN_POINT('Ctrl Pts',(-2.94236657469603,1.31487329732081,23.605219946086));
#17335=CARTESIAN_POINT('Ctrl Pts',(-2.93079126862344,1.34040960132749,23.6035093854782));
#17336=CARTESIAN_POINT('Ctrl Pts',(-2.92626052308691,1.35027208592793,23.6028455084534));
#17337=CARTESIAN_POINT('Ctrl Pts',(-2.91742512242411,1.369251571109,23.6015615989215));
#17338=CARTESIAN_POINT('Ctrl Pts',(-2.91312732808619,1.37837163951038,23.6009418102373));
#17339=CARTESIAN_POINT('Ctrl Pts',(-2.903149595988,1.39928961865373,23.5995136319135));
#17340=CARTESIAN_POINT('Ctrl Pts',(-2.89744043801717,1.41107331969898,23.598704230462));
#17341=CARTESIAN_POINT('Ctrl Pts',(-2.88199132391127,1.44247119519334,23.596534358403));
#17342=CARTESIAN_POINT('Ctrl Pts',(-2.87212312011212,1.46202116425962,23.595169411892));
#17343=CARTESIAN_POINT('Ctrl Pts',(-2.78694188367448,1.62658321611399,23.5835601028071));
#17344=CARTESIAN_POINT('Ctrl Pts',(-2.70091150987591,1.76575209718652,23.5729307481273));
#17345=CARTESIAN_POINT('Ctrl Pts',(-2.45557125247942,2.10248263817414,23.545146443374));
#17346=CARTESIAN_POINT('Ctrl Pts',(-2.28282668360327,2.2888776074864,23.5276660902053));
#17347=CARTESIAN_POINT('Ctrl Pts',(-2.0463505639998,2.49035386858803,23.507330104981));
#17348=CARTESIAN_POINT('Ctrl Pts',(-2.00166338426604,2.52641201793135,23.5036263665698));
#17349=CARTESIAN_POINT('Ctrl Pts',(-1.94670460576587,2.56838403069828,23.4992590450277));
#17350=CARTESIAN_POINT('Ctrl Pts',(-1.93733660678491,2.57545767452516,23.4985209991513));
#17351=CARTESIAN_POINT('Ctrl Pts',(-1.92270459545324,2.58638108631401,23.4973784011217));
#17352=CARTESIAN_POINT('Ctrl Pts',(-1.91746730860678,2.59026624253812,23.4969714356072));
#17353=CARTESIAN_POINT('Ctrl Pts',(-1.90772531440475,2.59744737035686,23.4962182059047));
#17354=CARTESIAN_POINT('Ctrl Pts',(-1.9032238788766,2.60074750496953,23.4958716582934));
#17355=CARTESIAN_POINT('Ctrl Pts',(-1.89301121552978,2.60819399364402,23.4950887794584));
#17356=CARTESIAN_POINT('Ctrl Pts',(-1.88729494194033,2.61233328175545,23.4946529397857));
#17357=CARTESIAN_POINT('Ctrl Pts',(-1.87032817688808,2.62453455667243,23.4933661131065));
#17358=CARTESIAN_POINT('Ctrl Pts',(-1.85903912693928,2.63254300418508,23.4925187325518));
#17359=CARTESIAN_POINT('Ctrl Pts',(-1.77443800079849,2.69174340063261,23.4862310817583));
#17360=CARTESIAN_POINT('Ctrl Pts',(-1.69906817421084,2.73994219679098,23.4809783123533));
#17361=CARTESIAN_POINT('Ctrl Pts',(-1.40908674704744,2.90880972599167,23.4616610906431));
#17362=CARTESIAN_POINT('Ctrl Pts',(-1.18289324916057,3.00790247008734,23.4482908659303));
#17363=CARTESIAN_POINT('Ctrl Pts',(-0.860129455762939,3.10719688098047,
23.4290622701824));
#17364=CARTESIAN_POINT('Ctrl Pts',(-0.771545523450982,3.13036910503995,
23.4237782834243));
#17365=CARTESIAN_POINT('Ctrl Pts',(-0.627442167056525,3.16157579305901,
23.4150832101366));
#17366=CARTESIAN_POINT('Ctrl Pts',(-0.572488010865,3.17198708610934,23.411744902349));
#17367=CARTESIAN_POINT('Ctrl Pts',(-0.50035837014777,3.18371692151814,23.4073227125596));
#17368=CARTESIAN_POINT('Ctrl Pts',(-0.483402089809228,3.18633556562968,
23.4062802567528));
#17369=CARTESIAN_POINT('Ctrl Pts',(-0.455692701324049,3.19038859576823,
23.4045716909189));
#17370=CARTESIAN_POINT('Ctrl Pts',(-0.444951691057949,3.1919043247132,23.4039081710456));
#17371=CARTESIAN_POINT('Ctrl Pts',(-0.424211089088408,3.19472443339366,
23.4026244817923));
#17372=CARTESIAN_POINT('Ctrl Pts',(-0.414212612275054,3.19603616399614,
23.4020045537042));
#17373=CARTESIAN_POINT('Ctrl Pts',(-0.391204066117126,3.19894494361641,
23.4005753791653));
#17374=CARTESIAN_POINT('Ctrl Pts',(-0.378190147285311,3.20050958098428,
23.3997651162847));
#17375=CARTESIAN_POINT('Ctrl Pts',(-0.343362164731023,3.20448149153999,
23.3975914315978));
#17376=CARTESIAN_POINT('Ctrl Pts',(-0.321532748517927,3.20674536858439,
23.3962235091299));
#17377=CARTESIAN_POINT('Ctrl Pts',(-0.134621460510709,3.22420181814927,
23.3844618970442));
#17378=CARTESIAN_POINT('Ctrl Pts',(0.0313564630761837,3.22685634812576,
23.3736714333013));
#17379=CARTESIAN_POINT('Ctrl Pts',(0.455215587198073,3.20092719503514,23.3453341553017));
#17380=CARTESIAN_POINT('Ctrl Pts',(0.710791378113481,3.15403362566845,23.3274478114267));
#17381=CARTESIAN_POINT('Ctrl Pts',(1.00587878474419,3.06216265899071,23.3073012665032));
#17382=CARTESIAN_POINT('Ctrl Pts',(1.05340769754504,3.04613938704135,23.3040761364205));
#17383=CARTESIAN_POINT('Ctrl Pts',(1.11114255435295,3.02516229162713,23.300199134563));
#17384=CARTESIAN_POINT('Ctrl Pts',(1.12171877131148,3.02125663818086,23.2994906171829));
#17385=CARTESIAN_POINT('Ctrl Pts',(1.13828451505387,3.0150401543997,23.2983837619123));
#17386=CARTESIAN_POINT('Ctrl Pts',(1.14428788259771,3.01276683686317,23.2979832437277));
#17387=CARTESIAN_POINT('Ctrl Pts',(1.15551032170329,3.00847881086517,23.2972357148469));
#17388=CARTESIAN_POINT('Ctrl Pts',(1.16073088063015,3.00646847352917,23.296888459463));
#17389=CARTESIAN_POINT('Ctrl Pts',(1.17266227986133,3.00183820966729,23.2960959058726));
#17390=CARTESIAN_POINT('Ctrl Pts',(1.17936957636924,2.99920937320804,23.2956511500624));
#17391=CARTESIAN_POINT('Ctrl Pts',(1.20005521802352,2.99102178633977,23.2942817530546));
#17392=CARTESIAN_POINT('Ctrl Pts',(1.21400373849476,2.98538754535174,23.2933615402977));
#17393=CARTESIAN_POINT('Ctrl Pts',(1.36499757930785,2.92316316154815,23.2834295072034));
#17394=CARTESIAN_POINT('Ctrl Pts',(1.49803995606594,2.85726956071792,23.274937967947));
#17395=CARTESIAN_POINT('Ctrl Pts',(1.7809426066236,2.69193830402996,23.2564761480718));
#17396=CARTESIAN_POINT('Ctrl Pts',(1.92797198300684,2.58867008066652,23.2465897220523));
#17397=CARTESIAN_POINT('Ctrl Pts',(2.13900779772982,2.41244641903759,23.2309634626143));
#17398=CARTESIAN_POINT('Ctrl Pts',(2.20960228444923,2.34795819939839,23.2254560971678));
#17399=CARTESIAN_POINT('Ctrl Pts',(2.31803511588966,2.23967793582064,23.2164277445039));
#17400=CARTESIAN_POINT('Ctrl Pts',(2.35774326056414,2.19783760717109,23.2129870667544));
#17401=CARTESIAN_POINT('Ctrl Pts',(2.40790540192232,2.14205743894685,23.2084482725536));
#17402=CARTESIAN_POINT('Ctrl Pts',(2.41940060032458,2.12906533793723,23.2073944093924));
#17403=CARTESIAN_POINT('Ctrl Pts',(2.43793988712447,2.1077678354039,23.2056718450925));
#17404=CARTESIAN_POINT('Ctrl Pts',(2.44504785384933,2.09951830879859,23.2050058165746));
#17405=CARTESIAN_POINT('Ctrl Pts',(2.45864792505329,2.08357129455813,23.2037205467818));
#17406=CARTESIAN_POINT('Ctrl Pts',(2.46514603902508,2.07587908161381,23.2031015644378));
#17407=CARTESIAN_POINT('Ctrl Pts',(2.47995895730957,2.05817649263383,23.2016792285407));
#17408=CARTESIAN_POINT('Ctrl Pts',(2.48824935169024,2.04814600568415,23.2008748902739));
#17409=CARTESIAN_POINT('Ctrl Pts',(2.51015308774261,2.02131556056798,23.1987273814628));
#17410=CARTESIAN_POINT('Ctrl Pts',(2.52365830095084,2.00442856259152,23.1973798788996));
#17411=CARTESIAN_POINT('Ctrl Pts',(2.63005464137795,1.86861005134807,23.1865731667816));
#17412=CARTESIAN_POINT('Ctrl Pts',(2.71464438528026,1.74344062173389,23.1767877507673));
#17413=CARTESIAN_POINT('Ctrl Pts',(2.90306114011268,1.4174838026103,23.1517684696872));
#17414=CARTESIAN_POINT('Ctrl Pts',(2.99514153334151,1.21084359295108,23.1362746097849));
#17415=CARTESIAN_POINT('Ctrl Pts',(3.09173564680503,0.913691271382811,23.1154725986853));
#17416=CARTESIAN_POINT('Ctrl Pts',(3.11523825088789,0.830032815332193,23.1097762521839));
#17417=CARTESIAN_POINT('Ctrl Pts',(3.13970055603478,0.727154948565412,23.103043566939));
#17418=CARTESIAN_POINT('Ctrl Pts',(3.14390604538316,0.708751521121015,23.1018496750971));
#17419=CARTESIAN_POINT('Ctrl Pts',(3.14964199882737,0.682594506694165,23.1001686658204));
#17420=CARTESIAN_POINT('Ctrl Pts',(3.15130593303898,0.674871025362513,23.0996742653177));
#17421=CARTESIAN_POINT('Ctrl Pts',(3.15412014314777,0.661570936860086,23.0988263498159));
#17422=CARTESIAN_POINT('Ctrl Pts',(3.15528406786835,0.655997282738108,23.0984720588096));
#17423=CARTESIAN_POINT('Ctrl Pts',(3.15750978518016,0.645196072755283,23.0977875308402));
#17424=CARTESIAN_POINT('Ctrl Pts',(3.15857337140228,0.639968963512682,23.0974571878117));
#17425=CARTESIAN_POINT('Ctrl Pts',(3.16140438853635,0.625876640648765,23.0965690148814));
#17426=CARTESIAN_POINT('Ctrl Pts',(3.16314752195943,0.617006512198318,23.0960125652215));
#17427=CARTESIAN_POINT('Ctrl Pts',(3.16946162142782,0.584146383218771,23.093960347199));
#17428=CARTESIAN_POINT('Ctrl Pts',(3.17379731526415,0.560111284524072,23.0924773961873));
#17429=CARTESIAN_POINT('Ctrl Pts',(3.20756711307151,0.359906082999947,23.0802577253081));
#17430=CARTESIAN_POINT('Ctrl Pts',(3.22258585402157,0.181594249522542,23.0702174695967));
#17431=CARTESIAN_POINT('Ctrl Pts',(3.22284147777808,-0.0989148519579887,
23.0545274662005));
#17432=CARTESIAN_POINT('Ctrl Pts',(3.21810585105701,-0.200713015188227,
23.0488570418605));
#17433=CARTESIAN_POINT('Ctrl Pts',(3.19226216798212,-0.475181664647695,
23.0333220153033));
#17434=CARTESIAN_POINT('Ctrl Pts',(3.161993280815,-0.646623485682562,23.0233364748469));
#17435=CARTESIAN_POINT('Ctrl Pts',(3.11246721164436,-0.836154088841001,
23.0115559094806));
#17436=CARTESIAN_POINT('Ctrl Pts',(3.10666124681708,-0.857474002019736,
23.0102202533736));
#17437=CARTESIAN_POINT('Ctrl Pts',(3.09705070864397,-0.8913851173586,23.0080782917782));
#17438=CARTESIAN_POINT('Ctrl Pts',(3.0933874288049,-0.904015888481335,23.0072765880475));
#17439=CARTESIAN_POINT('Ctrl Pts',(3.08677684194699,-0.926298073510278,
23.005855248115));
#17440=CARTESIAN_POINT('Ctrl Pts',(3.08386130371733,-0.93595878580489,23.0052366597524));
#17441=CARTESIAN_POINT('Ctrl Pts',(3.07772312887552,-0.955957722521362,
23.003951154834));
#17442=CARTESIAN_POINT('Ctrl Pts',(3.07449366567224,-0.966293702981811,
23.0032840202717));
#17443=CARTESIAN_POINT('Ctrl Pts',(3.06603862197241,-0.992882771972261,
23.0015606358833));
#17444=CARTESIAN_POINT('Ctrl Pts',(3.06073592314277,-1.00911080710241,23.0005018524689));
#17445=CARTESIAN_POINT('Ctrl Pts',(3.03775570048504,-1.0775901547028,22.9960039567947));
#17446=CARTESIAN_POINT('Ctrl Pts',(3.01886802422476,-1.12942263245547,22.9925249697677));
#17447=CARTESIAN_POINT('Ctrl Pts',(2.96576367896452,-1.26428854014951,22.9832694525274));
#17448=CARTESIAN_POINT('Ctrl Pts',(2.92939239713902,-1.34641655279006,22.9774250204547));
#17449=CARTESIAN_POINT('Ctrl Pts',(2.7775155876934,-1.65398231035852,22.9547564098506));
#17450=CARTESIAN_POINT('Ctrl Pts',(2.63902914746187,-1.86701855753947,22.937310216342));
#17451=CARTESIAN_POINT('Ctrl Pts',(2.42248544806351,-2.1271944469441,22.9148472242023));
#17452=CARTESIAN_POINT('Ctrl Pts',(2.36533777002322,-2.19056431023942,22.9092782688143));
#17453=CARTESIAN_POINT('Ctrl Pts',(2.2961755887461,-2.26138951720568,22.9030097420775));
#17454=CARTESIAN_POINT('Ctrl Pts',(2.28655093236064,-2.27112080970236,22.9021474495248));
#17455=CARTESIAN_POINT('Ctrl Pts',(2.27189308446883,-2.2857534245131,22.9008497392909));
#17456=CARTESIAN_POINT('Ctrl Pts',(2.26690552636812,-2.29069994579695,22.9004108569802));
#17457=CARTESIAN_POINT('Ctrl Pts',(2.25792754650664,-2.29954601727544,22.8996257034039));
#17458=CARTESIAN_POINT('Ctrl Pts',(2.25394315354121,-2.30345153041103,22.8992789654171));
#17459=CARTESIAN_POINT('Ctrl Pts',(2.24526196853389,-2.31191675972358,22.8985272077707));
#17460=CARTESIAN_POINT('Ctrl Pts',(2.24056143511393,-2.31647250545193,22.898122497205));
#17461=CARTESIAN_POINT('Ctrl Pts',(2.22731035954894,-2.32923734801768,22.896988032879));
#17462=CARTESIAN_POINT('Ctrl Pts',(2.21872825697574,-2.33741374022947,22.8962607814737));
#17463=CARTESIAN_POINT('Ctrl Pts',(2.16687451582886,-2.38627322480307,22.8919100020742));
#17464=CARTESIAN_POINT('Ctrl Pts',(2.12252703318354,-2.42580401137874,22.888369035569));
#17465=CARTESIAN_POINT('Ctrl Pts',(1.88456453261065,-2.62639499312878,22.8701312708296));
#17466=CARTESIAN_POINT('Ctrl Pts',(1.67364355903417,-2.76558799224177,22.8564605816914));
#17467=CARTESIAN_POINT('Ctrl Pts',(1.30336323045572,-2.95191703952021,22.8330393530403));
#17468=CARTESIAN_POINT('Ctrl Pts',(1.15277208258352,-3.01391376466645,22.8236635865327));
#17469=CARTESIAN_POINT('Ctrl Pts',(0.977349803980756,-3.07105581845121,
22.8125666016822));
#17470=CARTESIAN_POINT('Ctrl Pts',(0.95647365042571,-3.07762158155267,22.8112435862415));
#17471=CARTESIAN_POINT('Ctrl Pts',(0.923006754674466,-3.08777386302082,
22.809118089944));
#17472=CARTESIAN_POINT('Ctrl Pts',(0.910457990425474,-3.09149723242082,
22.8083200988784));
#17473=CARTESIAN_POINT('Ctrl Pts',(0.888204862771429,-3.09795276235891,
22.8069030603088));
#17474=CARTESIAN_POINT('Ctrl Pts',(0.878509652988541,-3.10071604343185,
22.8062850398243));
#17475=CARTESIAN_POINT('Ctrl Pts',(0.85834826725502,-3.10636019375571,22.8049984420609));
#17476=CARTESIAN_POINT('Ctrl Pts',(0.847880195402882,-3.10923375944567,
22.8043296354802));
#17477=CARTESIAN_POINT('Ctrl Pts',(0.820795351329398,-3.11652180430177,
22.8025970533432));
#17478=CARTESIAN_POINT('Ctrl Pts',(0.804157577363971,-3.12085625073552,
22.8015306923564));
#17479=CARTESIAN_POINT('Ctrl Pts',(0.732940287609785,-3.13880236361801,
22.7969568415844));
#17480=CARTESIAN_POINT('Ctrl Pts',(0.678046882550519,-3.15111623472367,
22.7934077796714));
#17481=CARTESIAN_POINT('Ctrl Pts',(0.532324772573121,-3.17982121514614,
22.7839182756014));
#17482=CARTESIAN_POINT('Ctrl Pts',(0.441070830339947,-3.19375744201291,
22.7779055800829));
#17483=CARTESIAN_POINT('Ctrl Pts',(0.112155686638735,-3.22962372138143,
22.7560140286166));
#17484=CARTESIAN_POINT('Ctrl Pts',(-0.127153782166928,-3.2290657790248,
22.7396144245407));
#17485=CARTESIAN_POINT('Ctrl Pts',(-0.390190164926113,-3.19914888458184,
22.721979896988));
#17486=CARTESIAN_POINT('Ctrl Pts',(-0.416147008387024,-3.19587604228232,
22.7202448461282));
#17487=CARTESIAN_POINT('Ctrl Pts',(-0.512369581614551,-3.18255133010016,
22.7138383990972));
#17488=CARTESIAN_POINT('Ctrl Pts',(-0.582342889367659,-3.17049428846126,
22.7092298097286));
#17489=CARTESIAN_POINT('Ctrl Pts',(-0.66350721219585,-3.15373065283494,
22.7039859813775));
#17490=CARTESIAN_POINT('Ctrl Pts',(-0.675134832243465,-3.15126194084545,
22.7032372189929));
#17491=CARTESIAN_POINT('Ctrl Pts',(-0.693781405861316,-3.14719505822461,
22.7020407323728));
#17492=CARTESIAN_POINT('Ctrl Pts',(-0.700808997814038,-3.14563763402576,
22.7015907705632));
#17493=CARTESIAN_POINT('Ctrl Pts',(-0.713301301468496,-3.14282520229928,
22.7007927225703));
#17494=CARTESIAN_POINT('Ctrl Pts',(-0.718768019083035,-3.14157946508569,
22.7004441113043));
#17495=CARTESIAN_POINT('Ctrl Pts',(-0.730417322589379,-3.13889286147994,
22.6997025800503));
#17496=CARTESIAN_POINT('Ctrl Pts',(-0.736598896133194,-3.13744799619852,
22.6993098935338));
#17497=CARTESIAN_POINT('Ctrl Pts',(-0.753432967160025,-3.13346074872979,
22.6982425815647));
#17498=CARTESIAN_POINT('Ctrl Pts',(-0.764076954978999,-3.13088229014925,
22.6975700035096));
#17499=CARTESIAN_POINT('Ctrl Pts',(-0.819092971003341,-3.11725763072769,
22.694104409404));
#17500=CARTESIAN_POINT('Ctrl Pts',(-0.863241875330294,-3.10532162499291,
22.6913597319615));
#17501=CARTESIAN_POINT('Ctrl Pts',(-0.993858879870399,-3.06700705535381,
22.6833074784171));
#17502=CARTESIAN_POINT('Ctrl Pts',(-1.0794912669506,-3.03792507448772,22.6781177175005));
#17503=CARTESIAN_POINT('Ctrl Pts',(-1.27010386193754,-2.96411041299132,
22.6665399313435));
#17504=CARTESIAN_POINT('Ctrl Pts',(-1.3740659605566,-2.91736423536877,22.6602050979509));
#17505=CARTESIAN_POINT('Ctrl Pts',(-1.47525567074797,-2.86526408354028,
22.6538402050192));
#17506=CARTESIAN_POINT('Ctrl Pts',(-1.47525540254685,-2.86526422163059,
22.4042343665403));
#17507=CARTESIAN_POINT('Ctrl Pts',(-1.45322971877909,-2.87660471467408,
22.4057161252439));
#17508=CARTESIAN_POINT('Ctrl Pts',(-1.43107352007128,-2.88769110816536,
22.4072064089249));
#17509=CARTESIAN_POINT('Ctrl Pts',(-1.39334536297762,-2.90602842271961,
22.4097448328548));
#17510=CARTESIAN_POINT('Ctrl Pts',(-1.37784003467455,-2.91341197143045,
22.4107882650628));
#17511=CARTESIAN_POINT('Ctrl Pts',(-1.35244495756436,-2.92525689314817,
22.4124978773526));
#17512=CARTESIAN_POINT('Ctrl Pts',(-1.34259025589495,-2.92979293711636,
22.4131614594788));
#17513=CARTESIAN_POINT('Ctrl Pts',(-1.32353623876708,-2.93844703382913,
22.4144448792718));
#17514=CARTESIAN_POINT('Ctrl Pts',(-1.3143401267935,-2.94257186375562,22.4150644737297));
#17515=CARTESIAN_POINT('Ctrl Pts',(-1.29315479607141,-2.95195522121264,
22.4164923187807));
#17516=CARTESIAN_POINT('Ctrl Pts',(-1.28115264258673,-2.95718393964771,
22.4173015812674));
#17517=CARTESIAN_POINT('Ctrl Pts',(-1.24898913782493,-2.97096335986562,
22.4194713299308));
#17518=CARTESIAN_POINT('Ctrl Pts',(-1.22877220429694,-2.97938181235266,
22.4208362930542));
#17519=CARTESIAN_POINT('Ctrl Pts',(-1.05674718003269,-3.0489653534888,22.432462148492));
#17520=CARTESIAN_POINT('Ctrl Pts',(-0.900592327912983,-3.09868087281126,
22.44310933739));
#17521=CARTESIAN_POINT('Ctrl Pts',(-0.494677170092165,-3.19463046798923,
22.4709270680005));
#17522=CARTESIAN_POINT('Ctrl Pts',(-0.241991377949537,-3.22363220156942,
22.4884224802909));
#17523=CARTESIAN_POINT('Ctrl Pts',(0.0684599282487246,-3.22252663922272,
22.5087397288792));
#17524=CARTESIAN_POINT('Ctrl Pts',(0.125432129728662,-3.22081238668123,
22.5124155379076));
#17525=CARTESIAN_POINT('Ctrl Pts',(0.194024557188503,-3.2169254217495,22.5167542553459));
#17526=CARTESIAN_POINT('Ctrl Pts',(0.205712796867072,-3.21619914697916,
22.5174905288601));
#17527=CARTESIAN_POINT('Ctrl Pts',(0.223895667099289,-3.2149697849469,22.5186308973221));
#17528=CARTESIAN_POINT('Ctrl Pts',(0.230393027895031,-3.21451070030062,
22.5190373918159));
#17529=CARTESIAN_POINT('Ctrl Pts',(0.242454076700921,-3.21362174520985,
22.519790057545));
#17530=CARTESIAN_POINT('Ctrl Pts',(0.248017987581257,-3.21319712734198,
22.5201365100683));
#17531=CARTESIAN_POINT('Ctrl Pts',(0.260620812775867,-3.21220239454543,
22.5209195573232));
#17532=CARTESIAN_POINT('Ctrl Pts',(0.267658955773023,-3.21162359519485,
22.5213556584787));
#17533=CARTESIAN_POINT('Ctrl Pts',(0.288512380968579,-3.20983963457576,
22.5226443897481));
#17534=CARTESIAN_POINT('Ctrl Pts',(0.302322058350977,-3.20856841328594,
22.5234933962686));
#17535=CARTESIAN_POINT('Ctrl Pts',(0.405958338277836,-3.19835334426186,
22.5298345006264));
#17536=CARTESIAN_POINT('Ctrl Pts',(0.495390763805186,-3.18572715539188,
22.5351354525269));
#17537=CARTESIAN_POINT('Ctrl Pts',(0.82513642869662,-3.12494774557831,22.5544292372362));
#17538=CARTESIAN_POINT('Ctrl Pts',(1.06024714340263,-3.0532013308953,22.5677420892157));
#17539=CARTESIAN_POINT('Ctrl Pts',(1.36904463361923,-2.91894494336931,22.5869140683537));
#17540=CARTESIAN_POINT('Ctrl Pts',(1.45151829549291,-2.87882189653155,22.5922064237613));
#17541=CARTESIAN_POINT('Ctrl Pts',(1.58142040089381,-2.80862272796431,22.6009137863255));
#17542=CARTESIAN_POINT('Ctrl Pts',(1.62997103252234,-2.78072759767424,22.6042557332862));
#17543=CARTESIAN_POINT('Ctrl Pts',(1.69241992837157,-2.74264959980722,22.6086818479368));
#17544=CARTESIAN_POINT('Ctrl Pts',(1.70699964601392,-2.73359913521743,22.609724488767));
#17545=CARTESIAN_POINT('Ctrl Pts',(1.73067483450581,-2.71863933031513,22.6114331301467));
#17546=CARTESIAN_POINT('Ctrl Pts',(1.73981410325174,-2.71279967426767,22.6120965384314));
#17547=CARTESIAN_POINT('Ctrl Pts',(1.7573901449328,-2.70144388162747,22.6133798509383));
#17548=CARTESIAN_POINT('Ctrl Pts',(1.7658308682519,-2.69593406969343,22.6139995131828));
#17549=CARTESIAN_POINT('Ctrl Pts',(1.78518017991956,-2.68317365352163,22.615427842815));
#17550=CARTESIAN_POINT('Ctrl Pts',(1.79607063487128,-2.67589599875276,22.6162375243417));
#17551=CARTESIAN_POINT('Ctrl Pts',(1.82506886688489,-2.65626086585125,22.6184091275367));
#17552=CARTESIAN_POINT('Ctrl Pts',(1.84309517689008,-2.6437848412629,22.6197755381873));
#17553=CARTESIAN_POINT('Ctrl Pts',(1.99555464559333,-2.53595043628054,22.6314752691923));
#17554=CARTESIAN_POINT('Ctrl Pts',(2.12259614317261,-2.43060766860434,22.6422005871061));
#17555=CARTESIAN_POINT('Ctrl Pts',(2.42498203397414,-2.13801623190877,22.6702716084906));
#17556=CARTESIAN_POINT('Ctrl Pts',(2.58707952297347,-1.9387280699498,22.6879478879665));
#17557=CARTESIAN_POINT('Ctrl Pts',(2.75256116690646,-1.67702198786059,22.7081735603941));
#17558=CARTESIAN_POINT('Ctrl Pts',(2.78009839957447,-1.63096579200221,22.711629231731));
#17559=CARTESIAN_POINT('Ctrl Pts',(2.81213002539656,-1.57422191485976,22.7157431282652));
#17560=CARTESIAN_POINT('Ctrl Pts',(2.81773184586419,-1.5641729991261,22.716466302724));
#17561=CARTESIAN_POINT('Ctrl Pts',(2.82639911570345,-1.54842740960731,22.7175908240267));
#17562=CARTESIAN_POINT('Ctrl Pts',(2.82950136289644,-1.54275125771672,22.7179944660571));
#17563=CARTESIAN_POINT('Ctrl Pts',(2.8352503489719,-1.53215672031368,22.7187445744796));
#17564=CARTESIAN_POINT('Ctrl Pts',(2.83790136472362,-1.52724084600527,22.7190913051145));
#17565=CARTESIAN_POINT('Ctrl Pts',(2.84390506021006,-1.51603836712711,22.7198784731553));
#17566=CARTESIAN_POINT('Ctrl Pts',(2.84724967412906,-1.50974753437871,22.7203183951823));
#17567=CARTESIAN_POINT('Ctrl Pts',(2.85740604107431,-1.49049078840475,22.7216587308275));
#17568=CARTESIAN_POINT('Ctrl Pts',(2.8641504039159,-1.47748927456935,22.7225549821171));
#17569=CARTESIAN_POINT('Ctrl Pts',(2.95591769727314,-1.29759405893309,22.7348426695496));
#17570=CARTESIAN_POINT('Ctrl Pts',(3.02633539781646,-1.12361696688319,22.7453982109505));
#17571=CARTESIAN_POINT('Ctrl Pts',(3.1293267469082,-0.787622524820779,22.7650658293388));
#17572=CARTESIAN_POINT('Ctrl Pts',(3.16535963327044,-0.627320475467666,
22.774168184583));
#17573=CARTESIAN_POINT('Ctrl Pts',(3.20663054694032,-0.344266472164632,
22.790545412426));
#17574=CARTESIAN_POINT('Ctrl Pts',(3.21736139637587,-0.222664446991262,
22.7976735473106));
#17575=CARTESIAN_POINT('Ctrl Pts',(3.22185521262994,-0.0789966814373223,
22.8063364478945));
#17576=CARTESIAN_POINT('Ctrl Pts',(3.22231531574506,-0.0572316074707122,
22.8076551765737));
#17577=CARTESIAN_POINT('Ctrl Pts',(3.22268533933331,-0.0236081262736721,
22.8097028226332));
#17578=CARTESIAN_POINT('Ctrl Pts',(3.22275038269521,-0.0117518040262375,
22.8104268650091));
#17579=CARTESIAN_POINT('Ctrl Pts',(3.2227497082,0.0090526696822713,22.8117009667173));
#17580=CARTESIAN_POINT('Ctrl Pts',(3.2227121502267,0.0180007428272791,22.8122501348685));
#17581=CARTESIAN_POINT('Ctrl Pts',(3.22254193397476,0.038356080270456,22.8135021183827));
#17582=CARTESIAN_POINT('Ctrl Pts',(3.22238597089199,0.049762981753632,22.8142056593519));
#17583=CARTESIAN_POINT('Ctrl Pts',(3.22179545835401,0.0808692748110246,
22.8161296118064));
#17584=CARTESIAN_POINT('Ctrl Pts',(3.22124080728934,0.10056564379393,22.8173537785317));
#17585=CARTESIAN_POINT('Ctrl Pts',(3.21734128608028,0.204997011659307,22.8238767937529));
#17586=CARTESIAN_POINT('Ctrl Pts',(3.2108337955714,0.289573637821328,22.8292741629082));
#17587=CARTESIAN_POINT('Ctrl Pts',(3.16499073090659,0.682157441107763,22.8548818038269));
#17588=CARTESIAN_POINT('Ctrl Pts',(3.08460691186131,0.983690953556932,22.8763613576528));
#17589=CARTESIAN_POINT('Ctrl Pts',(2.92951063011695,1.34575621022412,22.9024810845322));
#17590=CARTESIAN_POINT('Ctrl Pts',(2.89365089797501,1.42122462742229,22.9079304255786));
#17591=CARTESIAN_POINT('Ctrl Pts',(2.84858017312797,1.50728029147035,22.91408131592));
#17592=CARTESIAN_POINT('Ctrl Pts',(2.84218777350976,1.51929969239818,22.9149389292062));
#17593=CARTESIAN_POINT('Ctrl Pts',(2.8323898255087,1.53744415824987,22.9162309139965));
#17594=CARTESIAN_POINT('Ctrl Pts',(2.82904024007949,1.54359903653728,22.9166687067913));
#17595=CARTESIAN_POINT('Ctrl Pts',(2.82298903246918,1.55463229763009,22.917452586366));
#17596=CARTESIAN_POINT('Ctrl Pts',(2.82029481243083,1.55951461382646,22.9177991343051));
#17597=CARTESIAN_POINT('Ctrl Pts',(2.81440600240956,1.57012081772729,22.9185512492832));
#17598=CARTESIAN_POINT('Ctrl Pts',(2.81120662775958,1.5758419421079,22.9189565032595));
#17599=CARTESIAN_POINT('Ctrl Pts',(2.80214943465217,1.59192265550082,22.9200944299139));
#17600=CARTESIAN_POINT('Ctrl Pts',(2.79625158380103,1.60225974348419,22.920824574595));
#17601=CARTESIAN_POINT('Ctrl Pts',(2.76012656288475,1.66476858811073,22.9252330921424));
#17602=CARTESIAN_POINT('Ctrl Pts',(2.72849522372141,1.71612003983682,22.9288263234556));
#17603=CARTESIAN_POINT('Ctrl Pts',(2.55623141859803,1.97896270108199,22.9472312328831));
#17604=CARTESIAN_POINT('Ctrl Pts',(2.39239369164449,2.17418734575289,22.9610081970418));
#17605=CARTESIAN_POINT('Ctrl Pts',(2.09099404675542,2.45750872924679,22.9843988896392));
#17606=CARTESIAN_POINT('Ctrl Pts',(1.96672143661653,2.55804656304713,22.9936107804568));
#17607=CARTESIAN_POINT('Ctrl Pts',(1.81758991005193,2.66138318731217,23.004524376293));
#17608=CARTESIAN_POINT('Ctrl Pts',(1.79953180769067,2.67362652367145,23.0058433965151));
#17609=CARTESIAN_POINT('Ctrl Pts',(1.77046118004956,2.69290837859514,23.0079635453069));
#17610=CARTESIAN_POINT('Ctrl Pts',(1.7595275370096,2.7000650296207,23.0087602183328));
#17611=CARTESIAN_POINT('Ctrl Pts',(1.74008756295458,2.71262130486216,23.0101755588696));
#17612=CARTESIAN_POINT('Ctrl Pts',(1.73159882021473,2.71804793786105,23.0107932059048));
#17613=CARTESIAN_POINT('Ctrl Pts',(1.71390818691025,2.72924059211383,23.0120796677778));
#17614=CARTESIAN_POINT('Ctrl Pts',(1.70470233228443,2.73500007979567,23.0127487149544));
#17615=CARTESIAN_POINT('Ctrl Pts',(1.68082210430534,2.74977293469941,23.0144833014221));
#17616=CARTESIAN_POINT('Ctrl Pts',(1.66610442334965,2.75871531163775,23.0155514391407));
#17617=CARTESIAN_POINT('Ctrl Pts',(1.60275878491916,2.7965119462749,23.0201454239629));
#17618=CARTESIAN_POINT('Ctrl Pts',(1.55345015803031,2.82420019499376,23.0237133071182));
#17619=CARTESIAN_POINT('Ctrl Pts',(1.42121651061605,2.89394242332094,23.0332666167134));
#17620=CARTESIAN_POINT('Ctrl Pts',(1.33716089620935,2.93372753619857,23.0393255236725));
#17621=CARTESIAN_POINT('Ctrl Pts',(1.04136394055334,3.05837902265784,23.0605704412725));
#17622=CARTESIAN_POINT('Ctrl Pts',(0.822415701266829,3.12437841206829,23.0762177835746));
#17623=CARTESIAN_POINT('Ctrl Pts',(0.573999951462098,3.17131779024787,23.0931085944807));
#17624=CARTESIAN_POINT('Ctrl Pts',(0.549580979137327,3.17564060693655,23.0947592266122));
#17625=CARTESIAN_POINT('Ctrl Pts',(0.445160801710962,3.19288526264021,23.1017702736428));
#17626=CARTESIAN_POINT('Ctrl Pts',(0.364730125412771,3.20307021839355,23.1070528435679));
#17627=CARTESIAN_POINT('Ctrl Pts',(0.270535637951425,3.21140321009051,23.1130395310566));
#17628=CARTESIAN_POINT('Ctrl Pts',(0.25706958178469,3.21250919911265,23.113890631234));
#17629=CARTESIAN_POINT('Ctrl Pts',(0.236631518856113,3.21405847476445,23.1151747665248));
#17630=CARTESIAN_POINT('Ctrl Pts',(0.229664568085354,3.21456381850995,23.115611162306));
#17631=CARTESIAN_POINT('Ctrl Pts',(0.217134250674989,3.21543175337516,23.1163935569701));
#17632=CARTESIAN_POINT('Ctrl Pts',(0.21157156659384,3.21580256189583,23.1167400091665));
#17633=CARTESIAN_POINT('Ctrl Pts',(0.199449049380686,3.21657905748449,23.1174930897281));
#17634=CARTESIAN_POINT('Ctrl Pts',(0.192888949202968,3.21697911268353,23.1178993986197));
#17635=CARTESIAN_POINT('Ctrl Pts',(0.174366564217251,3.21805180350586,23.1190432783253));
#17636=CARTESIAN_POINT('Ctrl Pts',(0.162401537999565,3.21867781234849,23.1197782786353));
#17637=CARTESIAN_POINT('Ctrl Pts',(0.0887405114761992,3.22211994937534,
23.1242806168026));
#17638=CARTESIAN_POINT('Ctrl Pts',(0.0269730687194685,3.22322904189556,
23.1279585490219));
#17639=CARTESIAN_POINT('Ctrl Pts',(-0.303325724759565,3.21966295143925,
23.1472856278898));
#17640=CARTESIAN_POINT('Ctrl Pts',(-0.570464585437034,3.18321141872032,
23.1617933982917));
#17641=CARTESIAN_POINT('Ctrl Pts',(-0.96930712064195,3.07690504461795,23.1852360772557));
#17642=CARTESIAN_POINT('Ctrl Pts',(-1.10594368261036,3.0304755125018,23.1935946473569));
#17643=CARTESIAN_POINT('Ctrl Pts',(-1.25879865212571,2.96681703591995,23.2035577791438));
#17644=CARTESIAN_POINT('Ctrl Pts',(-1.27851060878884,2.95837589909697,23.204854493787));
#17645=CARTESIAN_POINT('Ctrl Pts',(-1.30999681723802,2.94451928369802,23.2069455564645));
#17646=CARTESIAN_POINT('Ctrl Pts',(-1.32182540470833,2.93922831114069,23.2077356426877));
#17647=CARTESIAN_POINT('Ctrl Pts',(-1.34277843906696,2.92970387552569,23.2091433928295));
#17648=CARTESIAN_POINT('Ctrl Pts',(-1.3519156302161,2.92549873693816,23.2097600730665));
#17649=CARTESIAN_POINT('Ctrl Pts',(-1.37092116156382,2.91664391612797,23.211048674904));
#17650=CARTESIAN_POINT('Ctrl Pts',(-1.38078586454126,2.91198677131387,23.2117208495585));
#17651=CARTESIAN_POINT('Ctrl Pts',(-1.40636545964738,2.8997513931425,23.2134726117019));
#17652=CARTESIAN_POINT('Ctrl Pts',(-1.4220426351027,2.89209555042265,23.2145548956032));
#17653=CARTESIAN_POINT('Ctrl Pts',(-1.49014442177158,2.85815090288789,23.2192948656409));
#17654=CARTESIAN_POINT('Ctrl Pts',(-1.54190529446969,2.83056254407517,23.222997977272));
#17655=CARTESIAN_POINT('Ctrl Pts',(-1.67795808770123,2.7532075694892,23.2330101747358));
#17656=CARTESIAN_POINT('Ctrl Pts',(-1.7607791835209,2.70099036201501,23.2394018164512));
#17657=CARTESIAN_POINT('Ctrl Pts',(-1.99724843279668,2.53639815068872,23.2585137970964));
#17658=CARTESIAN_POINT('Ctrl Pts',(-2.14346854841691,2.41409430318514,23.2714967982452));
#17659=CARTESIAN_POINT('Ctrl Pts',(-2.37287063611332,2.18485183189304,23.293324933616));
#17660=CARTESIAN_POINT('Ctrl Pts',(-2.46171182421877,2.08424471841882,23.3022304452959));
#17661=CARTESIAN_POINT('Ctrl Pts',(-2.55321365195604,1.9665810858594,23.3116810594943));
#17662=CARTESIAN_POINT('Ctrl Pts',(-2.56231025316098,1.9547141240218,23.3126238880156));
#17663=CARTESIAN_POINT('Ctrl Pts',(-2.57565531422471,1.93705159573314,23.3140114499348));
#17664=CARTESIAN_POINT('Ctrl Pts',(-2.57996735778249,1.93130464126623,23.3144604894685));
#17665=CARTESIAN_POINT('Ctrl Pts',(-2.58760051863936,1.92106022126617,23.3152565408995));
#17666=CARTESIAN_POINT('Ctrl Pts',(-2.59092918167654,1.91656849473916,23.3156040768049));
#17667=CARTESIAN_POINT('Ctrl Pts',(-2.59805988422804,1.90689373530676,23.3163494093141));
#17668=CARTESIAN_POINT('Ctrl Pts',(-2.60185810040356,1.90170799726412,23.3167469406906));
#17669=CARTESIAN_POINT('Ctrl Pts',(-2.61230190729453,1.8873591159388,23.3178415785149));
#17670=CARTESIAN_POINT('Ctrl Pts',(-2.61891485326957,1.87817216664992,23.3185364563075));
#17671=CARTESIAN_POINT('Ctrl Pts',(-2.65496455115509,1.82752997849801,23.3223353897162));
#17672=CARTESIAN_POINT('Ctrl Pts',(-2.68346734418187,1.78541487472923,23.3253793433852));
#17673=CARTESIAN_POINT('Ctrl Pts',(-2.85058457376423,1.52543655327208,23.3435947394204));
#17674=CARTESIAN_POINT('Ctrl Pts',(-2.96361104755742,1.29221865707019,23.3575973108754));
#17675=CARTESIAN_POINT('Ctrl Pts',(-3.1014722915409,0.891312107713129,23.3815331415055));
#17676=CARTESIAN_POINT('Ctrl Pts',(-3.14318038357564,0.730735256595542,
23.3910750167604));
#17677=CARTESIAN_POINT('Ctrl Pts',(-3.1762234250391,0.546080278224665,23.4023575552931));
#17678=CARTESIAN_POINT('Ctrl Pts',(-3.17986732999179,0.524445081228607,
23.4036838866644));
#17679=CARTESIAN_POINT('Ctrl Pts',(-3.18533421847902,0.48983178616469,23.405813561776));
#17680=CARTESIAN_POINT('Ctrl Pts',(-3.18729947627955,0.476876611609087,
23.4066123856015));
#17681=CARTESIAN_POINT('Ctrl Pts',(-3.19063675225289,0.453934244447489,
23.4080302141841));
#17682=CARTESIAN_POINT('Ctrl Pts',(-3.19204102731129,0.443951866087993,
23.408648186422));
#17683=CARTESIAN_POINT('Ctrl Pts',(-3.19485857372319,0.423218427691894,
23.4099339964793));
#17684=CARTESIAN_POINT('Ctrl Pts',(-3.19626446314255,0.412466508557065,
23.4106020600329));
#17685=CARTESIAN_POINT('Ctrl Pts',(-3.19975381011422,0.384691116111979,
23.4123312385098));
#17686=CARTESIAN_POINT('Ctrl Pts',(-3.20175566604097,0.3676579073031,23.4133949212816));
#17687=CARTESIAN_POINT('Ctrl Pts',(-3.20970259377268,0.295044567339758,
23.4179438840133));
#17688=CARTESIAN_POINT('Ctrl Pts',(-3.21433676661224,0.239333567620247,
23.4214701832064));
#17689=CARTESIAN_POINT('Ctrl Pts',(-3.22272915547479,0.0922064123224363,
23.4308840257047));
#17690=CARTESIAN_POINT('Ctrl Pts',(-3.22404749420441,0.000707038482247822,
23.4368424113532));
#17691=CARTESIAN_POINT('Ctrl Pts',(-3.21452647127309,-0.33739220971479,
23.4592128334957));
#17692=CARTESIAN_POINT('Ctrl Pts',(-3.17927327264488,-0.582425782554848,
23.4761971399821));
#17693=CARTESIAN_POINT('Ctrl Pts',(-3.09375545997647,-0.907030975617503,
23.4985045490449));
#17694=CARTESIAN_POINT('Ctrl Pts',(-3.06754393824343,-0.992071242905942,
23.5043198767823));
#17695=CARTESIAN_POINT('Ctrl Pts',(-3.03323088349472,-1.08895315502894,
23.5108291816523));
#17696=CARTESIAN_POINT('Ctrl Pts',(-3.02853304113299,-1.10195108843948,
23.511700014462));
#17697=CARTESIAN_POINT('Ctrl Pts',(-3.02131207321517,-1.12153495057391,
23.5130079146903));
#17698=CARTESIAN_POINT('Ctrl Pts',(-3.01885077921384,-1.1281432817695,23.5134485279367));
#17699=CARTESIAN_POINT('Ctrl Pts',(-3.01440326990669,-1.13996562148953,
23.5142354247814));
#17700=CARTESIAN_POINT('Ctrl Pts',(-3.01242519481193,-1.14518257889654,
23.5145821853487));
#17701=CARTESIAN_POINT('Ctrl Pts',(-3.00810580697121,-1.15648585789314,
23.5153324389512));
#17702=CARTESIAN_POINT('Ctrl Pts',(-3.00575957414438,-1.16257019988449,
23.5157356315296));
#17703=CARTESIAN_POINT('Ctrl Pts',(-2.99913589097792,-1.17959290091133,
23.5168619546224));
#17704=CARTESIAN_POINT('Ctrl Pts',(-2.99481703801444,-1.19051519231958,
23.5175826390556));
#17705=CARTESIAN_POINT('Ctrl Pts',(-2.96897885107539,-1.25482900932327,
23.5218158049831));
#17706=CARTESIAN_POINT('Ctrl Pts',(-2.94609034479315,-1.30766352404179,
23.5252508200958));
#17707=CARTESIAN_POINT('Ctrl Pts',(-2.81503165242162,-1.58925638332999,
23.5434734793986));
#17708=CARTESIAN_POINT('Ctrl Pts',(-2.6816134242665,-1.8053019174713,23.5572067219746));
#17709=CARTESIAN_POINT('Ctrl Pts',(-2.42266749240785,-2.13155217463521,
23.5807364962922));
#17710=CARTESIAN_POINT('Ctrl Pts',(-2.31147676360101,-2.25164323143822,
23.5901563358516));
#17711=CARTESIAN_POINT('Ctrl Pts',(-2.17561538761024,-2.37766580007576,
23.6013023089783));
#17712=CARTESIAN_POINT('Ctrl Pts',(-2.15941163707981,-2.39239175660236,
23.6026259955672));
#17713=CARTESIAN_POINT('Ctrl Pts',(-2.13328259973132,-2.41565607505237,
23.6047522249843));
#17714=CARTESIAN_POINT('Ctrl Pts',(-2.12345297697207,-2.42430121270163,
23.6055502712333));
#17715=CARTESIAN_POINT('Ctrl Pts',(-2.10596257794367,-2.4394960058312,23.6069671997905));
#17716=CARTESIAN_POINT('Ctrl Pts',(-2.09832319094735,-2.44607009810282,
23.6075850539353));
#17717=CARTESIAN_POINT('Ctrl Pts',(-2.08239667358617,-2.45964618579822,
23.6088710970561));
#17718=CARTESIAN_POINT('Ctrl Pts',(-2.07410478265755,-2.46664237606973,
23.6095395141452));
#17719=CARTESIAN_POINT('Ctrl Pts',(-2.05259453974916,-2.48460625272461,
23.611270636752));
#17720=CARTESIAN_POINT('Ctrl Pts',(-2.03932368092161,-2.49551026479727,
23.6123359210962));
#17721=CARTESIAN_POINT('Ctrl Pts',(-1.98231557615219,-2.54159260307848,
23.6169010180691));
#17722=CARTESIAN_POINT('Ctrl Pts',(-1.937752691411,-2.57572938624767,23.6204422127806));
#17723=CARTESIAN_POINT('Ctrl Pts',(-1.81784856679591,-2.66270711685815,
23.6299059253152));
#17724=CARTESIAN_POINT('Ctrl Pts',(-1.74110066664023,-2.71351221541542,
23.6359002224553));
#17725=CARTESIAN_POINT('Ctrl Pts',(-1.60108505231167,-2.79781132438933,
23.646712344991));
#17726=CARTESIAN_POINT('Ctrl Pts',(-1.53870409157046,-2.83259603402492,
23.6514881034905));
#17727=CARTESIAN_POINT('Ctrl Pts',(-1.47525500221108,-2.86526442775378,
23.6562919783988));
#17728=CARTESIAN_POINT('Origin',(0.,0.,4.68922655072688));
#17729=CARTESIAN_POINT('',(-1.4752554489605,-2.86526419773332,25.1553455282223));
#17730=CARTESIAN_POINT('',(-1.47525540501177,-2.86526422036146,24.9102129806979));
#17731=CARTESIAN_POINT('',(-1.47525540501186,-2.86526422036142,4.68922655072688));
#17732=CARTESIAN_POINT('',(3.22274971917068,-0.00134539409721628,24.3082009925199));
#17733=CARTESIAN_POINT('Ctrl Pts',(-1.4752554489605,-2.86526419773332,25.1553455282223));
#17734=CARTESIAN_POINT('Ctrl Pts',(-1.6729476371766,-2.76347725671983,25.1405536479666));
#17735=CARTESIAN_POINT('Ctrl Pts',(-1.85960157496954,-2.64149118000024,
25.1252848161754));
#17736=CARTESIAN_POINT('Ctrl Pts',(-2.10472042139451,-2.44233335256714,
25.104262226728));
#17737=CARTESIAN_POINT('Ctrl Pts',(-2.17461939367043,-2.38030970656153,
25.0981454939901));
#17738=CARTESIAN_POINT('Ctrl Pts',(-2.25177214785347,-2.30560948181583,
25.091342864128));
#17739=CARTESIAN_POINT('Ctrl Pts',(-2.26174977643724,-2.29582247874771,
25.0904621128427));
#17740=CARTESIAN_POINT('Ctrl Pts',(-2.27669012753043,-2.28097563375094,
25.089142195969));
#17741=CARTESIAN_POINT('Ctrl Pts',(-2.28170019225532,-2.27596397456147,
25.0886993903266));
#17742=CARTESIAN_POINT('Ctrl Pts',(-2.2906283785988,-2.26697383575064,25.0879100215358));
#17743=CARTESIAN_POINT('Ctrl Pts',(-2.29455271577956,-2.2630016740854,25.0875629696937));
#17744=CARTESIAN_POINT('Ctrl Pts',(-2.30302290155424,-2.25438357977174,
25.0868137188299));
#17745=CARTESIAN_POINT('Ctrl Pts',(-2.30756501123034,-2.24973410218541,
25.0864118116754));
#17746=CARTESIAN_POINT('Ctrl Pts',(-2.32020282131241,-2.23671901497513,
25.0852931019164));
#17747=CARTESIAN_POINT('Ctrl Pts',(-2.32826740325088,-2.22832313468614,
25.0845786912661));
#17748=CARTESIAN_POINT('Ctrl Pts',(-2.37471680402311,-2.17943809116738,
25.0804595282793));
#17749=CARTESIAN_POINT('Ctrl Pts',(-2.41209311506719,-2.13799858941098,
25.0771274479861));
#17750=CARTESIAN_POINT('Ctrl Pts',(-2.61381780098597,-1.90231595568482,
25.058905277118));
#17751=CARTESIAN_POINT('Ctrl Pts',(-2.75580311829823,-1.69009649929761,
25.0450993882415));
#17752=CARTESIAN_POINT('Ctrl Pts',(-2.94581325347143,-1.31726635967942,
25.0214636371805));
#17753=CARTESIAN_POINT('Ctrl Pts',(-3.00900307551504,-1.16571712665636,
25.0120147998813));
#17754=CARTESIAN_POINT('Ctrl Pts',(-3.06725195365497,-0.989223488618128,
25.0008360956684));
#17755=CARTESIAN_POINT('Ctrl Pts',(-3.07390651490528,-0.968347230562795,
24.9995114760654));
#17756=CARTESIAN_POINT('Ctrl Pts',(-3.08419785144542,-0.934886472816387,
24.9973838896407));
#17757=CARTESIAN_POINT('Ctrl Pts',(-3.08797174725157,-0.922344612465189,
24.9965854267481));
#17758=CARTESIAN_POINT('Ctrl Pts',(-3.0945153487017,-0.90010775881865,24.9951678422757));
#17759=CARTESIAN_POINT('Ctrl Pts',(-3.09731622015955,-0.890422062565233,
24.994549750359));
#17760=CARTESIAN_POINT('Ctrl Pts',(-3.10303722031383,-0.870284629476614,
24.9932632951313));
#17761=CARTESIAN_POINT('Ctrl Pts',(-3.10595009718327,-0.85983098115339,
24.9925947039665));
#17762=CARTESIAN_POINT('Ctrl Pts',(-3.11333727880239,-0.832792663152279,
24.9908633062624));
#17763=CARTESIAN_POINT('Ctrl Pts',(-3.11773183896444,-0.816186739216616,
24.9897979209897));
#17764=CARTESIAN_POINT('Ctrl Pts',(-3.13591382390471,-0.745191468872054,
24.9852339221997));
#17765=CARTESIAN_POINT('Ctrl Pts',(-3.14841162837986,-0.690484913627083,
24.9816939588657));
#17766=CARTESIAN_POINT('Ctrl Pts',(-3.17760629628235,-0.545335699095486,
24.9722349572338));
#17767=CARTESIAN_POINT('Ctrl Pts',(-3.19187014628047,-0.454461488905316,
24.9662442416565));
#17768=CARTESIAN_POINT('Ctrl Pts',(-3.22953527826587,-0.122295075124919,
24.9441291584514));
#17769=CARTESIAN_POINT('Ctrl Pts',(-3.22958907876854,0.120804237530324,
24.9274609781128));
#17770=CARTESIAN_POINT('Ctrl Pts',(-3.19203217200052,0.453415756912826,
24.9051884974746));
#17771=CARTESIAN_POINT('Ctrl Pts',(-3.17771971835471,0.544753228201643,
24.8991392126235));
#17772=CARTESIAN_POINT('Ctrl Pts',(-3.15675078290543,0.649027329570261,
24.8924020075446));
#17773=CARTESIAN_POINT('Ctrl Pts',(-3.15391313751876,0.662679347366521,
24.8915233322234));
#17774=CARTESIAN_POINT('Ctrl Pts',(-3.14950126455894,0.683234560676992,
24.8902059106636));
#17775=CARTESIAN_POINT('Ctrl Pts',(-3.14799279164465,0.690151480754959,
24.8897635442948));
#17776=CARTESIAN_POINT('Ctrl Pts',(-3.14525390208734,0.702514502483954,
24.8889746497863));
#17777=CARTESIAN_POINT('Ctrl Pts',(-3.14403211844039,0.707962410433881,
24.8886276354098));
#17778=CARTESIAN_POINT('Ctrl Pts',(-3.14135620704655,0.719750689922282,
24.8878781144852));
#17779=CARTESIAN_POINT('Ctrl Pts',(-3.13989704375085,0.726089823372296,
24.8874759016928));
#17780=CARTESIAN_POINT('Ctrl Pts',(-3.13576774699403,0.743783744039376,
24.8863554775728));
#17781=CARTESIAN_POINT('Ctrl Pts',(-3.13305511408969,0.755128653116896,
24.8856396701029));
#17782=CARTESIAN_POINT('Ctrl Pts',(-3.11692203213957,0.821017490441438,
24.8814961112207));
#17783=CARTESIAN_POINT('Ctrl Pts',(-3.10213811351939,0.875221507299935,
24.8781420420911));
#17784=CARTESIAN_POINT('Ctrl Pts',(-3.01268248788995,1.17236958577065,24.8599187943197));
#17785=CARTESIAN_POINT('Ctrl Pts',(-2.9108864933613,1.40622663247106,24.846127555343));
#17786=CARTESIAN_POINT('Ctrl Pts',(-2.70000639353231,1.76718081087724,24.8225144987084));
#17787=CARTESIAN_POINT('Ctrl Pts',(-2.60669838954595,1.9021239733909,24.8130729713214));
#17788=CARTESIAN_POINT('Ctrl Pts',(-2.48974914338014,2.04639848110886,24.8019024446313));
#17789=CARTESIAN_POINT('Ctrl Pts',(-2.47578041442358,2.0632762402786,24.8005779844864));
#17790=CARTESIAN_POINT('Ctrl Pts',(-2.45318821007887,2.09001356201534,24.7984506058183));
#17791=CARTESIAN_POINT('Ctrl Pts',(-2.44467467129812,2.09996543472617,24.7976521898178));
#17792=CARTESIAN_POINT('Ctrl Pts',(-2.42950004153543,2.11748642653252,24.7962346596094));
#17793=CARTESIAN_POINT('Ctrl Pts',(-2.42286360749482,2.12507674077382,24.7956165748016));
#17794=CARTESIAN_POINT('Ctrl Pts',(-2.40901029674304,2.14077199264923,24.7943301054563));
#17795=CARTESIAN_POINT('Ctrl Pts',(-2.40178788970076,2.1488718581152,24.7936614929211));
#17796=CARTESIAN_POINT('Ctrl Pts',(-2.38302707541794,2.16969920545936,24.7919299777081));
#17797=CARTESIAN_POINT('Ctrl Pts',(-2.37142767854558,2.18237105721132,24.7908644956327));
#17798=CARTESIAN_POINT('Ctrl Pts',(-2.32150312194548,2.23604352947094,24.7862995203618));
#17799=CARTESIAN_POINT('Ctrl Pts',(-2.282213696084,2.27612992099538,24.7827586553437));
#17800=CARTESIAN_POINT('Ctrl Pts',(-2.17581952672817,2.37915701479309,24.773296632497));
#17801=CARTESIAN_POINT('Ctrl Pts',(-2.10703564796589,2.44028214893733,24.7673037404475));
#17802=CARTESIAN_POINT('Ctrl Pts',(-1.84811748796279,2.65125473882761,24.7452086250471));
#17803=CARTESIAN_POINT('Ctrl Pts',(-1.6438952129299,2.78249592997477,24.7285647116915));
#17804=CARTESIAN_POINT('Ctrl Pts',(-1.34383369240142,2.93066808635624,24.7062948952702));
#17805=CARTESIAN_POINT('Ctrl Pts',(-1.25900668477802,2.96809872995206,24.7002275843406));
#17806=CARTESIAN_POINT('Ctrl Pts',(-1.15967553281428,3.00690289742189,24.6934725241263));
#17807=CARTESIAN_POINT('Ctrl Pts',(-1.146641657436,3.01189729272933,24.6925929433587));
#17808=CARTESIAN_POINT('Ctrl Pts',(-1.12694563712223,3.01929813933051,24.6912744333829));
#17809=CARTESIAN_POINT('Ctrl Pts',(-1.12030753341063,3.02176748874773,24.6908318753605));
#17810=CARTESIAN_POINT('Ctrl Pts',(-1.10842178268842,3.02614439329539,24.6900427739945));
#17811=CARTESIAN_POINT('Ctrl Pts',(-1.10317728683387,3.02806020627151,24.689695743342));
#17812=CARTESIAN_POINT('Ctrl Pts',(-1.09181407924996,3.03217774264091,24.6889463405642));
#17813=CARTESIAN_POINT('Ctrl Pts',(-1.08569369323693,3.03437457358939,24.6885442613695));
#17814=CARTESIAN_POINT('Ctrl Pts',(-1.06858563783361,3.04045689341282,24.6874245867104));
#17815=CARTESIAN_POINT('Ctrl Pts',(-1.05758334777731,3.04430137441449,24.6867093898967));
#17816=CARTESIAN_POINT('Ctrl Pts',(-0.993591021593331,3.06627313684402,
24.6825765194278));
#17817=CARTESIAN_POINT('Ctrl Pts',(-0.940152947678015,3.08307758315236,
24.6792320845371));
#17818=CARTESIAN_POINT('Ctrl Pts',(-0.641838643400723,3.16840843410577,
24.661009325323));
#17819=CARTESIAN_POINT('Ctrl Pts',(-0.389937988087602,3.20916571835361,
24.6472116799436));
#17820=CARTESIAN_POINT('Ctrl Pts',(0.0279135230043758,3.2267944853697,24.623588683288));
#17821=CARTESIAN_POINT('Ctrl Pts',(0.191938285503035,3.22120025181376,24.6141439418682));
#17822=CARTESIAN_POINT('Ctrl Pts',(0.37658978821368,3.20074643222523,24.6029698197408));
#17823=CARTESIAN_POINT('Ctrl Pts',(0.398340583107129,3.19811230814808,24.601645289459));
#17824=CARTESIAN_POINT('Ctrl Pts',(0.433047640480566,3.1935495664764,24.5995178194098));
#17825=CARTESIAN_POINT('Ctrl Pts',(0.446022174967081,3.19176335337657,24.5987193827837));
#17826=CARTESIAN_POINT('Ctrl Pts',(0.468965041662789,3.18846216994225,24.5973018287075));
#17827=CARTESIAN_POINT('Ctrl Pts',(0.478937885533747,3.18697940338271,24.5966837407731));
#17828=CARTESIAN_POINT('Ctrl Pts',(0.499630038966506,3.18380356731472,24.5953972776388));
#17829=CARTESIAN_POINT('Ctrl Pts',(0.510348069211088,3.18210310560857,24.5947286745044));
#17830=CARTESIAN_POINT('Ctrl Pts',(0.538009619951665,3.17757113372551,24.5929972109834));
#17831=CARTESIAN_POINT('Ctrl Pts',(0.55493928815878,3.1746582539048,24.5919317714914));
#17832=CARTESIAN_POINT('Ctrl Pts',(0.627071446577371,3.16165275117239,24.5873672257987));
#17833=CARTESIAN_POINT('Ctrl Pts',(0.682025766080417,3.15025505851074,24.5838267574572));
#17834=CARTESIAN_POINT('Ctrl Pts',(0.826187375948994,3.1164066697373,24.5743660637734));
#17835=CARTESIAN_POINT('Ctrl Pts',(0.914774531885293,3.09156289642311,24.5683741292643));
#17836=CARTESIAN_POINT('Ctrl Pts',(1.17885253166699,3.00515923969121,24.5499927190242));
#17837=CARTESIAN_POINT('Ctrl Pts',(1.35019111875876,2.93217500841037,24.5373326160988));
#17838=CARTESIAN_POINT('Ctrl Pts',(1.64427291870194,2.77563938895823,24.5148589401816));
#17839=CARTESIAN_POINT('Ctrl Pts',(1.76939813693502,2.69760045319533,24.5050345372913));
#17840=CARTESIAN_POINT('Ctrl Pts',(1.9009395391703,2.60245508195972,24.494740329168));
#17841=CARTESIAN_POINT('Ctrl Pts',(1.91305950899005,2.59355873673594,24.4937922514419));
#17842=CARTESIAN_POINT('Ctrl Pts',(1.9308930914166,2.58027543184358,24.4923983841245));
#17843=CARTESIAN_POINT('Ctrl Pts',(1.93665475892088,2.57595376157947,24.4919482341003));
#17844=CARTESIAN_POINT('Ctrl Pts',(1.94668006870897,2.56838140013181,24.4911653587003));
#17845=CARTESIAN_POINT('Ctrl Pts',(1.95095013328329,2.56513935010743,24.4908320355451));
#17846=CARTESIAN_POINT('Ctrl Pts',(1.96014725859599,2.55812017465189,24.4901143918472));
#17847=CARTESIAN_POINT('Ctrl Pts',(1.96507149092677,2.55433947243311,24.4897303298131));
#17848=CARTESIAN_POINT('Ctrl Pts',(1.97813132114702,2.54425234516561,24.4887121028772));
#17849=CARTESIAN_POINT('Ctrl Pts',(1.98624776170592,2.53792106958016,24.4880796725364));
#17850=CARTESIAN_POINT('Ctrl Pts',(2.00428239561474,2.52371354138743,24.4866749169837));
#17851=CARTESIAN_POINT('Ctrl Pts',(2.01418483147779,2.51581744900714,24.4859039340546));
#17852=CARTESIAN_POINT('Ctrl Pts',(2.04405939667445,2.49170634999754,24.483578107108));
#17853=CARTESIAN_POINT('Ctrl Pts',(2.06388464684956,2.47531000159465,24.4820348462725));
#17854=CARTESIAN_POINT('Ctrl Pts',(2.1372194358587,2.41316524279882,24.4763178423725));
#17855=CARTESIAN_POINT('Ctrl Pts',(2.18942474387131,2.36590236463068,24.4722308882994));
#17856=CARTESIAN_POINT('Ctrl Pts',(2.29056578578179,2.26811912021095,24.4641800867823));
#17857=CARTESIAN_POINT('Ctrl Pts',(2.33947898128169,2.21763268243842,24.4602181756911));
#17858=CARTESIAN_POINT('Ctrl Pts',(2.57607961297247,1.95687385586951,24.4404725230852));
#17859=CARTESIAN_POINT('Ctrl Pts',(2.73724060734724,1.72425072498668,24.4249599727797));
#17860=CARTESIAN_POINT('Ctrl Pts',(2.88161592510557,1.4434539565627,24.4061058217089));
#17861=CARTESIAN_POINT('Ctrl Pts',(2.89665826072096,1.41302528372264,24.404063191413));
#17862=CARTESIAN_POINT('Ctrl Pts',(2.91684885417585,1.37050455237372,24.4012071157634));
#17863=CARTESIAN_POINT('Ctrl Pts',(2.92240833796023,1.35860938625818,24.4004079489244));
#17864=CARTESIAN_POINT('Ctrl Pts',(2.93185748149023,1.33806546744392,24.3990272677861));
#17865=CARTESIAN_POINT('Ctrl Pts',(2.93578197246169,1.32943284676682,24.3984469638973));
#17866=CARTESIAN_POINT('Ctrl Pts',(2.94381077507445,1.31156313276792,24.397245379705));
#17867=CARTESIAN_POINT('Ctrl Pts',(2.94790983958032,1.30232380945377,24.3966239268906));
#17868=CARTESIAN_POINT('Ctrl Pts',(2.95737658454358,1.28071198523998,24.3951697665496));
#17869=CARTESIAN_POINT('Ctrl Pts',(2.96271016872835,1.26832483976613,24.3943359025323));
#17870=CARTESIAN_POINT('Ctrl Pts',(2.97965479520074,1.22828114036154,24.3916388190147));
#17871=CARTESIAN_POINT('Ctrl Pts',(2.99095725913929,1.20049649483063,24.3897651644836));
#17872=CARTESIAN_POINT('Ctrl Pts',(3.06672367198217,1.00652677323359,24.3766654881088));
#17873=CARTESIAN_POINT('Ctrl Pts',(3.11768058812873,0.835427827277531,24.3649864569444));
#17874=CARTESIAN_POINT('Ctrl Pts',(3.19988227671476,0.443180281133057,24.3381105219092));
#17875=CARTESIAN_POINT('Ctrl Pts',(3.22284262905124,0.221210429567681,24.3228189241854));
#17876=CARTESIAN_POINT('Ctrl Pts',(3.22274971917068,-0.00134539409721628,
24.3082009925199));
#17877=CARTESIAN_POINT('Ctrl Pts',(3.22274971730435,-0.00134985730486836,
24.3082006993672));
#17878=CARTESIAN_POINT('Ctrl Pts',(3.22272611847844,-0.0576914493070022,
24.3045000684272));
#17879=CARTESIAN_POINT('Ctrl Pts',(3.22122503310341,-0.114027358852287,
24.3008485886178));
#17880=CARTESIAN_POINT('Ctrl Pts',(3.21763171638925,-0.181932434322062,
24.2965283935334));
#17881=CARTESIAN_POINT('Ctrl Pts',(3.216953041538,-0.193562421226479,24.2957913636844));
#17882=CARTESIAN_POINT('Ctrl Pts',(3.21574738020973,-0.212460450845194,
24.2945986987601));
#17883=CARTESIAN_POINT('Ctrl Pts',(3.21525878745669,-0.21973071835699,24.2941410634133));
#17884=CARTESIAN_POINT('Ctrl Pts',(3.21435594844119,-0.232516647997579,
24.2933384153753));
#17885=CARTESIAN_POINT('Ctrl Pts',(3.21395215492318,-0.238032984740623,
24.2929928356879));
#17886=CARTESIAN_POINT('Ctrl Pts',(3.21312678841451,-0.248923405379457,
24.2923120331622));
#17887=CARTESIAN_POINT('Ctrl Pts',(3.21270592952824,-0.25429752705337,24.2919767729835));
#17888=CARTESIAN_POINT('Ctrl Pts',(3.21177217405417,-0.265848604809996,
24.2912576917194));
#17889=CARTESIAN_POINT('Ctrl Pts',(3.21125494200837,-0.272025141616444,
24.2908741176208));
#17890=CARTESIAN_POINT('Ctrl Pts',(3.20983274749543,-0.288438746112081,
24.2898571834809));
#17891=CARTESIAN_POINT('Ctrl Pts',(3.20889662305333,-0.298673143100265,
24.2892255556648));
#17892=CARTESIAN_POINT('Ctrl Pts',(3.20467668553058,-0.34249655741897,24.286530826195));
#17893=CARTESIAN_POINT('Ctrl Pts',(3.20091418699029,-0.376038731325203,
24.2844931858975));
#17894=CARTESIAN_POINT('Ctrl Pts',(3.19574890328151,-0.416358111283861,
24.2820672109328));
#17895=CARTESIAN_POINT('Ctrl Pts',(3.19485054474195,-0.42319632322785,24.2816565748235));
#17896=CARTESIAN_POINT('Ctrl Pts',(3.18845352662548,-0.470708243187338,
24.2788087941088));
#17897=CARTESIAN_POINT('Ctrl Pts',(3.18220002482987,-0.511278227520204,
24.2764042004489));
#17898=CARTESIAN_POINT('Ctrl Pts',(3.13231992230041,-0.798340774617772,
24.2595135074652));
#17899=CARTESIAN_POINT('Ctrl Pts',(3.06087826987678,-1.03914359726351,24.2459311725056));
#17900=CARTESIAN_POINT('Ctrl Pts',(2.92363227638845,-1.35945570862508,24.2261474396549));
#17901=CARTESIAN_POINT('Ctrl Pts',(2.88089121046845,-1.44782909361593,24.2204997571257));
#17902=CARTESIAN_POINT('Ctrl Pts',(2.8062170288156,-1.58578568515502,24.2112628227676));
#17903=CARTESIAN_POINT('Ctrl Pts',(2.77683940710086,-1.63668338424854,24.2077588242451));
#17904=CARTESIAN_POINT('Ctrl Pts',(2.7369487043779,-1.70162695297487,24.2031480172696));
#17905=CARTESIAN_POINT('Ctrl Pts',(2.72768846474372,-1.7164317982755,24.2020872596129));
#17906=CARTESIAN_POINT('Ctrl Pts',(2.71244543505698,-1.74036675915395,24.2003562313325));
#17907=CARTESIAN_POINT('Ctrl Pts',(2.70653569253712,-1.74954315034476,24.1996886836483));
#17908=CARTESIAN_POINT('Ctrl Pts',(2.69508894200696,-1.76712036576084,24.1984024204139));
#17909=CARTESIAN_POINT('Ctrl Pts',(2.68955897647542,-1.77552564070816,24.1977839743252));
#17910=CARTESIAN_POINT('Ctrl Pts',(2.67681702397765,-1.79469665829309,24.1963656067243));
#17911=CARTESIAN_POINT('Ctrl Pts',(2.66957931922211,-1.80544502149589,24.1955647189245));
#17912=CARTESIAN_POINT('Ctrl Pts',(2.65019728662681,-1.83385697006,24.1934324056417));
#17913=CARTESIAN_POINT('Ctrl Pts',(2.63794137482374,-1.85144330505086,24.192096744609));
#17914=CARTESIAN_POINT('Ctrl Pts',(2.54217306659655,-1.985982334368,24.1817543975051));
#17915=CARTESIAN_POINT('Ctrl Pts',(2.45110923366623,-2.0973371635772,24.1724530051659));
#17916=CARTESIAN_POINT('Ctrl Pts',(2.21079083088228,-2.35410047327926,24.1491339007185));
#17917=CARTESIAN_POINT('Ctrl Pts',(2.05428412735991,-2.4918450984332,24.1349007799878));
#17918=CARTESIAN_POINT('Ctrl Pts',(1.81911399923169,-2.66151580122257,24.1154524185763));
#17919=CARTESIAN_POINT('Ctrl Pts',(1.75080032782474,-2.70694332886011,24.1100094466256));
#17920=CARTESIAN_POINT('Ctrl Pts',(1.65651091706464,-2.7645797371878,24.1028383669054));
#17921=CARTESIAN_POINT('Ctrl Pts',(1.63200121828692,-2.7791188685191,24.1010042582028));
#17922=CARTESIAN_POINT('Ctrl Pts',(1.59549065752063,-2.8001272812595,24.0983196034499));
#17923=CARTESIAN_POINT('Ctrl Pts',(1.58363707821053,-2.80684820551168,24.09745529088));
#17924=CARTESIAN_POINT('Ctrl Pts',(1.56211690328792,-2.81887031844465,24.0958997672088));
#17925=CARTESIAN_POINT('Ctrl Pts',(1.55246512261849,-2.8241974334514,24.0952070320824));
#17926=CARTESIAN_POINT('Ctrl Pts',(1.53723218844534,-2.83250327040854,24.0941216665714));
#17927=CARTESIAN_POINT('Ctrl Pts',(1.53166938281182,-2.83551520564763,24.0937269671112));
#17928=CARTESIAN_POINT('Ctrl Pts',(1.52608297889153,-2.83851868134005,24.0933322802369));
#17929=CARTESIAN_POINT('Ctrl Pts',(1.52606826931835,-2.83852658965151,24.0933312409977));
#17930=CARTESIAN_POINT('Ctrl Pts',(1.52603876597003,-2.83854245124831,24.0933291565938));
#17931=CARTESIAN_POINT('Ctrl Pts',(1.52602397223478,-2.83855040451053,24.0933281114321));
#17932=CARTESIAN_POINT('Ctrl Pts',(1.52599429994296,-2.83856635633676,24.09332601514));
#17933=CARTESIAN_POINT('Ctrl Pts',(1.52597942145734,-2.83857435486092,24.0933249640146));
#17934=CARTESIAN_POINT('Ctrl Pts',(1.52594957915564,-2.83859039747959,24.0933228557596));
#17935=CARTESIAN_POINT('Ctrl Pts',(1.52593461528087,-2.83859844160393,24.0933217986259));
#17936=CARTESIAN_POINT('Ctrl Pts',(1.52590460158884,-2.83861457574676,24.0933196783114));
#17937=CARTESIAN_POINT('Ctrl Pts',(1.52588955181141,-2.83862266574209,24.0933186151335));
#17938=CARTESIAN_POINT('Ctrl Pts',(1.52585936573625,-2.83863889193224,24.0933164826902));
#17939=CARTESIAN_POINT('Ctrl Pts',(1.52584422940474,-2.83864702814344,24.0933154134225));
#17940=CARTESIAN_POINT('Ctrl Pts',(1.52581386970112,-2.83866334703966,24.0933132687632));
#17941=CARTESIAN_POINT('Ctrl Pts',(1.52579864621495,-2.8386715297842,24.0933121933637));
#17942=CARTESIAN_POINT('Ctrl Pts',(1.52576811152512,-2.83868794210552,24.0933100363934));
#17943=CARTESIAN_POINT('Ctrl Pts',(1.52575280035856,-2.83869617166053,24.0933089548254));
#17944=CARTESIAN_POINT('Ctrl Pts',(1.52572208969444,-2.83871267792711,24.0933067854752));
#17945=CARTESIAN_POINT('Ctrl Pts',(1.52570669016765,-2.83872095465252,24.093305697691));
#17946=CARTESIAN_POINT('Ctrl Pts',(1.52567580207615,-2.83873755563428,24.0933035158591));
#17947=CARTESIAN_POINT('Ctrl Pts',(1.52566031365799,-2.83874587980999,24.0933024218218));
#17948=CARTESIAN_POINT('Ctrl Pts',(1.52562924723898,-2.83876257597951,24.0933002274456));
#17949=CARTESIAN_POINT('Ctrl Pts',(1.52561366918939,-2.83877094799761,24.0932991271033));
#17950=CARTESIAN_POINT('Ctrl Pts',(1.52558242299352,-2.83878774012247,24.0932969200811));
#17951=CARTESIAN_POINT('Ctrl Pts',(1.52556675473582,-2.83879616028718,24.0932958133936));
#17952=CARTESIAN_POINT('Ctrl Pts',(1.52553532736088,-2.83881304910943,24.0932935936275));
#17953=CARTESIAN_POINT('Ctrl Pts',(1.52551956836973,-2.83882151769728,24.093292480558));
#17954=CARTESIAN_POINT('Ctrl Pts',(1.52081608179185,-2.84134903316195,24.0929602737499));
#17955=CARTESIAN_POINT('Ctrl Pts',(1.51612218716979,-2.84385643043855,24.0926299394626));
#17956=CARTESIAN_POINT('Ctrl Pts',(1.505127765827,-2.84969450276225,24.0918589687811));
#17957=CARTESIAN_POINT('Ctrl Pts',(1.49882239364927,-2.85301591042443,24.0914189239173));
#17958=CARTESIAN_POINT('Ctrl Pts',(1.47952275217551,-2.8631005180928,24.0900783058564));
#17959=CARTESIAN_POINT('Ctrl Pts',(1.46649313046066,-2.86979617186681,24.0891818961851));
#17960=CARTESIAN_POINT('Ctrl Pts',(1.3534305405323,-2.92692558378284,24.0814742459288));
#17961=CARTESIAN_POINT('Ctrl Pts',(1.25086482383982,-2.97220633841499,24.074958445455));
#17962=CARTESIAN_POINT('Ctrl Pts',(0.938878597766879,-3.09092231841185,
24.0559336421543));
#17963=CARTESIAN_POINT('Ctrl Pts',(0.724030821360556,-3.14818670966018,
24.043817715302));
#17964=CARTESIAN_POINT('Ctrl Pts',(0.414149559277967,-3.197351884165,24.0259558215109));
#17965=CARTESIAN_POINT('Ctrl Pts',(0.32273079920224,-3.20786873594387,24.0206465905525));
#17966=CARTESIAN_POINT('Ctrl Pts',(0.175012104098916,-3.21848384762885,
24.0119137764077));
#17967=CARTESIAN_POINT('Ctrl Pts',(0.118939287106756,-3.22104336867269,
24.0085638022479));
#17968=CARTESIAN_POINT('Ctrl Pts',(0.045654698846357,-3.22247239507271,
24.0041283121576));
#17969=CARTESIAN_POINT('Ctrl Pts',(0.0284765932823386,-3.22266997292476,
24.0030845396962));
#17970=CARTESIAN_POINT('Ctrl Pts',(0.000445749918927757,-3.22276824116028,
24.001374358534));
#17971=CARTESIAN_POINT('Ctrl Pts',(-0.0104065000985307,-3.22275146964891,
24.0007105494556));
#17972=CARTESIAN_POINT('Ctrl Pts',(-0.0313405787650945,-3.22261337834556,
23.9994266819546));
#17973=CARTESIAN_POINT('Ctrl Pts',(-0.0414223426062536,-3.22249955841968,
23.9988068668742));
#17974=CARTESIAN_POINT('Ctrl Pts',(-0.0645981823043494,-3.22212913407854,
23.997378499618));
#17975=CARTESIAN_POINT('Ctrl Pts',(-0.0776914929905667,-3.22184001862488,
23.9965689347545));
#17976=CARTESIAN_POINT('Ctrl Pts',(-0.112682024448718,-3.22085396949826,
23.994398339621));
#17977=CARTESIAN_POINT('Ctrl Pts',(-0.134574211536866,-3.22001355195475,
23.9930328287572));
#17978=CARTESIAN_POINT('Ctrl Pts',(-0.320111452152123,-3.21099559303374,
23.9813949179584));
#17979=CARTESIAN_POINT('Ctrl Pts',(-0.48289642428386,-3.19057367892996,
23.9707353284948));
#17980=CARTESIAN_POINT('Ctrl Pts',(-0.892458755343471,-3.10712708071275,
23.9428577648043));
#17981=CARTESIAN_POINT('Ctrl Pts',(-1.1346241356111,-3.02710168051018,23.9253125334914));
#17982=CARTESIAN_POINT('Ctrl Pts',(-1.40200467514313,-2.90209940887585,
23.9060049343196));
#17983=CARTESIAN_POINT('Ctrl Pts',(-1.43880709431877,-2.88403057601107,
23.9033511807881));
#17984=CARTESIAN_POINT('Ctrl Pts',(-1.47525540579296,-2.86526421995924,
23.9007338658376));
#17985=CARTESIAN_POINT('',(3.22274871883436,0.00294606298623907,24.0644510358235));
#17986=CARTESIAN_POINT('Ctrl Pts',(-1.47525500221108,-2.86526442775378,
23.6562919783988));
#17987=CARTESIAN_POINT('Ctrl Pts',(-1.35501449326435,-2.92717334288701,
23.66539566089));
#17988=CARTESIAN_POINT('Ctrl Pts',(-1.23093834006357,-2.98148176035773,
23.6746058007793));
#17989=CARTESIAN_POINT('Ctrl Pts',(-1.06125504918383,-3.04333723869333,
23.6867427906442));
#17990=CARTESIAN_POINT('Ctrl Pts',(-1.01843236752905,-3.05793387479908,
23.6897675694313));
#17991=CARTESIAN_POINT('Ctrl Pts',(-0.896131251797879,-3.09676744961024,
23.6982752342562));
#17992=CARTESIAN_POINT('Ctrl Pts',(-0.815996610383085,-3.11884145230336,
23.7036952953616));
#17993=CARTESIAN_POINT('Ctrl Pts',(-0.721854105060323,-3.14089621823618,
23.7098174001187));
#17994=CARTESIAN_POINT('Ctrl Pts',(-0.708597134893948,-3.14391356727594,
23.7106738953522));
#17995=CARTESIAN_POINT('Ctrl Pts',(-0.688482717532451,-3.14835800983582,
23.7119645330641));
#17996=CARTESIAN_POINT('Ctrl Pts',(-0.681639256307718,-3.14984674816108,
23.7124020863922));
#17997=CARTESIAN_POINT('Ctrl Pts',(-0.669338399808847,-3.15248073145383,
23.7131857109715));
#17998=CARTESIAN_POINT('Ctrl Pts',(-0.663882863291371,-3.15363412604507,
23.7135322420379));
#17999=CARTESIAN_POINT('Ctrl Pts',(-0.652004743979297,-3.15611317622217,
23.7142845204303));
#18000=CARTESIAN_POINT('Ctrl Pts',(-0.64558111997756,-3.15743338593735,
23.7146899536029));
#18001=CARTESIAN_POINT('Ctrl Pts',(-0.627495999504634,-3.1610928162827,
23.7158276049144));
#18002=CARTESIAN_POINT('Ctrl Pts',(-0.615825375341265,-3.16338713089543,
23.7165573005808));
#18003=CARTESIAN_POINT('Ctrl Pts',(-0.545596904617962,-3.17678988256905,
23.7209230150544));
#18004=CARTESIAN_POINT('Ctrl Pts',(-0.486748636447364,-3.18633751389046,
23.7244759221006));
#18005=CARTESIAN_POINT('Ctrl Pts',(-0.178351781968121,-3.22762754863927,
23.7427058563803));
#18006=CARTESIAN_POINT('Ctrl Pts',(0.0740337350894962,-3.23170749934384,
23.756361700223));
#18007=CARTESIAN_POINT('Ctrl Pts',(0.48616298444265,-3.19001820592334,23.7797667809561));
#18008=CARTESIAN_POINT('Ctrl Pts',(0.646489030090305,-3.16142567068359,
23.7891427035139));
#18009=CARTESIAN_POINT('Ctrl Pts',(0.825147708080403,-3.11540166303046,
23.8002395684217));
#18010=CARTESIAN_POINT('Ctrl Pts',(0.846278637719261,-3.10972807385802,
23.8015622885838));
#18011=CARTESIAN_POINT('Ctrl Pts',(0.879952695819982,-3.10031805667791,
23.8036872587954));
#18012=CARTESIAN_POINT('Ctrl Pts',(0.892533907208071,-3.09671955720899,
23.8044850207787));
#18013=CARTESIAN_POINT('Ctrl Pts',(0.914765038984831,-3.09021424025871,
23.8059016204532));
#18014=CARTESIAN_POINT('Ctrl Pts',(0.924423949925147,-3.08733857624765,
23.8065194315728));
#18015=CARTESIAN_POINT('Ctrl Pts',(0.944454518431882,-3.08127262228611,
23.8078055606249));
#18016=CARTESIAN_POINT('Ctrl Pts',(0.954823855481484,-3.07807516325195,
23.8084741075427));
#18017=CARTESIAN_POINT('Ctrl Pts',(0.981573251099225,-3.0696786232762,23.8102059439827));
#18018=CARTESIAN_POINT('Ctrl Pts',(0.997928063356344,-3.06440083203845,
23.8112718163663));
#18019=CARTESIAN_POINT('Ctrl Pts',(1.06661739791045,-3.04162619505369,23.8157785566935));
#18020=CARTESIAN_POINT('Ctrl Pts',(1.11853767362501,-3.02291836625736,23.819259273343));
#18021=CARTESIAN_POINT('Ctrl Pts',(1.25406706855988,-2.97011500583209,23.8285482522597));
#18022=CARTESIAN_POINT('Ctrl Pts',(1.33676343911608,-2.93382488745419,23.834425563345));
#18023=CARTESIAN_POINT('Ctrl Pts',(1.59670386779309,-2.80648049592037,23.8535589079507));
#18024=CARTESIAN_POINT('Ctrl Pts',(1.76706723784177,-2.70245417439077,23.8671501579441));
#18025=CARTESIAN_POINT('Ctrl Pts',(2.03630191168107,-2.50165529906279,23.8897674708355));
#18026=CARTESIAN_POINT('Ctrl Pts',(2.140585387477,-2.41302877311659,23.8988554990754));
#18027=CARTESIAN_POINT('Ctrl Pts',(2.24970502970148,-2.30763278737043,23.9084746082637));
#18028=CARTESIAN_POINT('Ctrl Pts',(2.26040347840411,-2.29715431289018,23.9094188920179));
#18029=CARTESIAN_POINT('Ctrl Pts',(2.27612957281539,-2.28153531948098,23.9108081763813));
#18030=CARTESIAN_POINT('Ctrl Pts',(2.28121349740218,-2.27645211413106,23.911257498303));
#18031=CARTESIAN_POINT('Ctrl Pts',(2.29022094497711,-2.26738546476366,23.9120538598688));
#18032=CARTESIAN_POINT('Ctrl Pts',(2.29415114698657,-2.26340878745183,23.9124014250934));
#18033=CARTESIAN_POINT('Ctrl Pts',(2.30257549373215,-2.25484033533461,23.9131466079634));
#18034=CARTESIAN_POINT('Ctrl Pts',(2.30706624983459,-2.25024535612596,23.9135439615046));
#18035=CARTESIAN_POINT('Ctrl Pts',(2.31626327062054,-2.24077841545018,23.9143580627839));
#18036=CARTESIAN_POINT('Ctrl Pts',(2.32096798053656,-2.23590498036585,23.9147746906139));
#18037=CARTESIAN_POINT('Ctrl Pts',(2.34278176513552,-2.2131658460865,23.9167074534881));
#18038=CARTESIAN_POINT('Ctrl Pts',(2.3597007016229,-2.19511779775449,23.9182094898553));
#18039=CARTESIAN_POINT('Ctrl Pts',(2.4603058140135,-2.0852911203896,23.9271722835486));
#18040=CARTESIAN_POINT('Ctrl Pts',(2.5388459193516,-1.98892229591896,23.9343035936125));
#18041=CARTESIAN_POINT('Ctrl Pts',(2.67497785140488,-1.80063858862975,23.9474288538256));
#18042=CARTESIAN_POINT('Ctrl Pts',(2.73387462724788,-1.70989363532544,23.953442110129));
#18043=CARTESIAN_POINT('Ctrl Pts',(2.89936381633995,-1.42443695814654,23.9718991429425));
#18044=CARTESIAN_POINT('Ctrl Pts',(2.99049838142456,-1.22156937410308,23.9844482723722));
#18045=CARTESIAN_POINT('Ctrl Pts',(3.06700682795415,-0.989987288220592,
23.9991153671845));
#18046=CARTESIAN_POINT('Ctrl Pts',(3.07372163147684,-0.968938082916184,
24.0004509022121));
#18047=CARTESIAN_POINT('Ctrl Pts',(3.08408632943807,-0.935255021296776,
24.0025925643959));
#18048=CARTESIAN_POINT('Ctrl Pts',(3.08787632344865,-0.92266475240612,24.0033940899914));
#18049=CARTESIAN_POINT('Ctrl Pts',(3.09443776181317,-0.900374513825484,
24.0048150503338));
#18050=CARTESIAN_POINT('Ctrl Pts',(3.0972409212201,-0.890684006326842,24.0054334374104));
#18051=CARTESIAN_POINT('Ctrl Pts',(3.10295746209706,-0.870568616125252,
24.006718460023));
#18052=CARTESIAN_POINT('Ctrl Pts',(3.1058639082949,-0.860141910117466,24.0073853131027));
#18053=CARTESIAN_POINT('Ctrl Pts',(3.11321653887819,-0.833241557047083,
24.0091078315793));
#18054=CARTESIAN_POINT('Ctrl Pts',(3.11758447447725,-0.816747045776657,
24.010166027344));
#18055=CARTESIAN_POINT('Ctrl Pts',(3.12675520766976,-0.780970098158403,
24.0124658587325));
#18056=CARTESIAN_POINT('Ctrl Pts',(3.13151103668481,-0.761676454577913,
24.0137089685928));
#18057=CARTESIAN_POINT('Ctrl Pts',(3.14484963700839,-0.705326261651034,
24.0173484380911));
#18058=CARTESIAN_POINT('Ctrl Pts',(3.15295492175332,-0.668161236810485,
24.0197598422052));
#18059=CARTESIAN_POINT('Ctrl Pts',(3.20206604532974,-0.422131776493012,
24.0357991765311));
#18060=CARTESIAN_POINT('Ctrl Pts',(3.22294311519104,-0.209825326838229,
24.0500514525995));
#18061=CARTESIAN_POINT('Ctrl Pts',(3.22274865402096,0.00294542120983694,
24.0644511057929));
#18062=CARTESIAN_POINT('Ctrl Pts',(3.22274865344138,0.00294605528672446,
24.0644511487053));
#18063=CARTESIAN_POINT('Ctrl Pts',(3.22257424051969,0.193739829951134,24.0773634697639));
#18064=CARTESIAN_POINT('Ctrl Pts',(3.20545713209499,0.38416323532263,24.0903280746391));
#18065=CARTESIAN_POINT('Ctrl Pts',(3.1680420070958,0.591630312469549,24.1038803127039));
#18066=CARTESIAN_POINT('Ctrl Pts',(3.16431396051559,0.611255911091983,24.1051562853375));
#18067=CARTESIAN_POINT('Ctrl Pts',(3.1583337291344,0.6412155863569,24.1070936217749));
#18068=CARTESIAN_POINT('Ctrl Pts',(3.15621283004422,0.651574977527513,24.1077615797314));
#18069=CARTESIAN_POINT('Ctrl Pts',(3.15263594041671,0.668618713616982,24.1088571419945));
#18070=CARTESIAN_POINT('Ctrl Pts',(3.15120960487839,0.675309103398219,24.109286333799));
#18071=CARTESIAN_POINT('Ctrl Pts',(3.14839236198354,0.688320408276996,24.1101192671277));
#18072=CARTESIAN_POINT('Ctrl Pts',(3.14700369587475,0.694641770517087,24.1105231315873));
#18073=CARTESIAN_POINT('Ctrl Pts',(3.14438127631797,0.70641003762993,24.1112734370777));
#18074=CARTESIAN_POINT('Ctrl Pts',(3.14315242014287,0.711857862594848,24.1116201436863));
#18075=CARTESIAN_POINT('Ctrl Pts',(3.14032474832309,0.724243553994647,24.1124069797451));
#18076=CARTESIAN_POINT('Ctrl Pts',(3.13871710354107,0.731179319092189,24.112846595562));
#18077=CARTESIAN_POINT('Ctrl Pts',(3.13373785625912,0.752341928964205,24.1141850723056));
#18078=CARTESIAN_POINT('Ctrl Pts',(3.13029235685533,0.766551439356025,24.1150797877288));
#18079=CARTESIAN_POINT('Ctrl Pts',(3.08084063353047,0.964599082230346,24.1275004397034));
#18080=CARTESIAN_POINT('Ctrl Pts',(3.01879557047716,1.1440828570201,24.1381704702521));
#18081=CARTESIAN_POINT('Ctrl Pts',(2.89741941620183,1.41513912309252,24.1547879539275));
#18082=CARTESIAN_POINT('Ctrl Pts',(2.84864104414521,1.51092747489552,24.1607653099469));
#18083=CARTESIAN_POINT('Ctrl Pts',(2.7303686184339,1.71701921436141,24.1741611830375));
#18084=CARTESIAN_POINT('Ctrl Pts',(2.65878889794799,1.82589830084581,24.1816066354104));
#18085=CARTESIAN_POINT('Ctrl Pts',(2.54802211060111,1.97400629539456,24.1925187698509));
#18086=CARTESIAN_POINT('Ctrl Pts',(2.51410726639772,2.01702296614655,24.1957891554825));
#18087=CARTESIAN_POINT('Ctrl Pts',(2.4681434522575,2.07236103966723,24.2001423084582));
#18088=CARTESIAN_POINT('Ctrl Pts',(2.4570674392062,2.08548123009915,24.2011855405999));
#18089=CARTESIAN_POINT('Ctrl Pts',(2.43882364003762,2.10674499904715,24.2028949074325));
#18090=CARTESIAN_POINT('Ctrl Pts',(2.43171855068622,2.11494210888023,24.203558445607));
#18091=CARTESIAN_POINT('Ctrl Pts',(2.41793229060742,2.13068594338065,24.2048418382391));
#18092=CARTESIAN_POINT('Ctrl Pts',(2.41125682657882,2.13823751343846,24.2054614497991));
#18093=CARTESIAN_POINT('Ctrl Pts',(2.39582833611797,2.15552675295422,24.2068894171928));
#18094=CARTESIAN_POINT('Ctrl Pts',(2.38705121559434,2.16524259260801,24.2076987854872));
#18095=CARTESIAN_POINT('Ctrl Pts',(2.3634322150114,2.19106950381674,24.2098690023689));
#18096=CARTESIAN_POINT('Ctrl Pts',(2.34848507152311,2.20708296991166,24.2112343309402));
#18097=CARTESIAN_POINT('Ctrl Pts',(2.22028468992882,2.34165222240276,24.2228787541535));
#18098=CARTESIAN_POINT('Ctrl Pts',(2.09831732878074,2.45154011020355,24.2335455738464));
#18099=CARTESIAN_POINT('Ctrl Pts',(1.7673728713867,2.70685483234764,24.2614242813834));
#18100=CARTESIAN_POINT('Ctrl Pts',(1.54857277478894,2.83770814833509,24.2789622729782));
#18101=CARTESIAN_POINT('Ctrl Pts',(1.26547648421944,2.96442813989084,24.2992514917287));
#18102=CARTESIAN_POINT('Ctrl Pts',(1.21367736426211,2.9860095596947,24.3028692077757));
#18103=CARTESIAN_POINT('Ctrl Pts',(1.15051361895523,3.01041037375209,24.3071454164687));
#18104=CARTESIAN_POINT('Ctrl Pts',(1.13966691919165,3.01453338491351,24.307874994511));
#18105=CARTESIAN_POINT('Ctrl Pts',(1.12267045947586,3.02088917357439,24.309010547216));
#18106=CARTESIAN_POINT('Ctrl Pts',(1.1165358969297,3.0231619130095,24.3094188475786));
#18107=CARTESIAN_POINT('Ctrl Pts',(1.10515842710991,3.02733769536926,24.3101731645203));
#18108=CARTESIAN_POINT('Ctrl Pts',(1.09991754618758,3.02924579114625,24.3105194731006));
#18109=CARTESIAN_POINT('Ctrl Pts',(1.08806529401254,3.03352613537252,24.311300057659));
#18110=CARTESIAN_POINT('Ctrl Pts',(1.08145112281534,3.03589037502868,24.3117338532452));
#18111=CARTESIAN_POINT('Ctrl Pts',(1.06192221602457,3.04279907468965,24.3130094840718));
#18112=CARTESIAN_POINT('Ctrl Pts',(1.04898599961458,3.04728295205405,24.3138478043363));
#18113=CARTESIAN_POINT('Ctrl Pts',(0.955073852361015,3.07916534133483,24.3198881296645));
#18114=CARTESIAN_POINT('Ctrl Pts',(0.873057049286566,3.10341738120102,24.3249189096906));
#18115=CARTESIAN_POINT('Ctrl Pts',(0.545200965533929,3.18633318101863,24.3444250860297));
#18116=CARTESIAN_POINT('Ctrl Pts',(0.293791480015071,3.21926484363748,24.3581294537396));
#18117=CARTESIAN_POINT('Ctrl Pts',(-0.048898636982619,3.22363584253016,
24.3776584188829));
#18118=CARTESIAN_POINT('Ctrl Pts',(-0.138902661482797,3.22101278182098,
24.3828583027745));
#18119=CARTESIAN_POINT('Ctrl Pts',(-0.283591862806194,3.21072023353168,
24.3914156364599));
#18120=CARTESIAN_POINT('Ctrl Pts',(-0.338397613738702,3.20540719286101,
24.3947027484781));
#18121=CARTESIAN_POINT('Ctrl Pts',(-0.410085940613719,3.19659852064754,
24.399073436722));
#18122=CARTESIAN_POINT('Ctrl Pts',(-0.427116544299522,3.19436754627795,
24.4001170203681));
#18123=CARTESIAN_POINT('Ctrl Pts',(-0.454873866964155,3.19050545076618,
24.4018268184557));
#18124=CARTESIAN_POINT('Ctrl Pts',(-0.465611761865991,3.18895609077262,
24.4024904338522));
#18125=CARTESIAN_POINT('Ctrl Pts',(-0.486309487350851,3.1858628696838,24.4037738742214));
#18126=CARTESIAN_POINT('Ctrl Pts',(-0.496270313999639,3.18432644584016,
24.4043934557498));
#18127=CARTESIAN_POINT('Ctrl Pts',(-0.519151583812424,3.18068711982856,
24.4058212082679));
#18128=CARTESIAN_POINT('Ctrl Pts',(-0.53206668295296,3.17855217952802,24.4066303907225));
#18129=CARTESIAN_POINT('Ctrl Pts',(-0.566548107276294,3.17263615981567,
24.4087997852522));
#18130=CARTESIAN_POINT('Ctrl Pts',(-0.588089213208508,3.1687139346304,24.4101644719775));
#18131=CARTESIAN_POINT('Ctrl Pts',(-0.770085840178279,3.13365611754573,
24.4217763231803));
#18132=CARTESIAN_POINT('Ctrl Pts',(-0.927973620651493,3.09057975835651,
24.4324087088191));
#18133=CARTESIAN_POINT('Ctrl Pts',(-1.32025717203633,2.9507747803975,24.4601814736142));
#18134=CARTESIAN_POINT('Ctrl Pts',(-1.54777290994755,2.83805299065389,24.4776458692179));
#18135=CARTESIAN_POINT('Ctrl Pts',(-1.8079936417756,2.66844369592543,24.4979804078286));
#18136=CARTESIAN_POINT('Ctrl Pts',(-1.85538233226048,2.63571435154134,24.5016954876566));
#18137=CARTESIAN_POINT('Ctrl Pts',(-1.91135408391638,2.59479885318771,24.5060741613684));
#18138=CARTESIAN_POINT('Ctrl Pts',(-1.92079856470474,2.58781537333286,24.5068126715601));
#18139=CARTESIAN_POINT('Ctrl Pts',(-1.93542694946986,2.57687458191231,24.5079557441687));
#18140=CARTESIAN_POINT('Ctrl Pts',(-1.94063726323917,2.57295299256633,24.5083627241473));
#18141=CARTESIAN_POINT('Ctrl Pts',(-1.95028330828932,2.56564684038222,24.5091158314141));
#18142=CARTESIAN_POINT('Ctrl Pts',(-1.95472211262946,2.56226660503796,24.5094622428762));
#18143=CARTESIAN_POINT('Ctrl Pts',(-1.96475112774461,2.55458808655141,24.5102446173204));
#18144=CARTESIAN_POINT('Ctrl Pts',(-1.97033600920023,2.55028298410312,24.5106800903161));
#18145=CARTESIAN_POINT('Ctrl Pts',(-1.9868240186762,2.53748672037562,24.5119652461032));
#18146=CARTESIAN_POINT('Ctrl Pts',(-1.99768687527023,2.52894359397724,24.5128113351084));
#18147=CARTESIAN_POINT('Ctrl Pts',(-2.07802741129571,2.46491884539269,24.5190671529117));
#18148=CARTESIAN_POINT('Ctrl Pts',(-2.14524427402452,2.40664765655043,24.5242915035578));
#18149=CARTESIAN_POINT('Ctrl Pts',(-2.3895978880475,2.17642966234909,24.5436224866327));
#18150=CARTESIAN_POINT('Ctrl Pts',(-2.54919781335098,1.98711577753219,24.5570263705841));
#18151=CARTESIAN_POINT('Ctrl Pts',(-2.73618867289765,1.70521375745317,24.5762892272467));
#18152=CARTESIAN_POINT('Ctrl Pts',(-2.78347382147463,1.62688475057072,24.5815693907238));
#18153=CARTESIAN_POINT('Ctrl Pts',(-2.8541848172216,1.49762156696859,24.5902585224235));
#18154=CARTESIAN_POINT('Ctrl Pts',(-2.87972632738041,1.44790090747874,24.5935948304297));
#18155=CARTESIAN_POINT('Ctrl Pts',(-2.9113980488819,1.38209011206338,24.5980145159087));
#18156=CARTESIAN_POINT('Ctrl Pts',(-2.9187114480335,1.36657789471678,24.5990565196174));
#18157=CARTESIAN_POINT('Ctrl Pts',(-2.93044621215406,1.34116372530757,24.6007643793668));
#18158=CARTESIAN_POINT('Ctrl Pts',(-2.93494208563866,1.33129639442586,24.6014276477208));
#18159=CARTESIAN_POINT('Ctrl Pts',(-2.94352139200188,1.31221225380076,24.6027108741476));
#18160=CARTESIAN_POINT('Ctrl Pts',(-2.94761154979834,1.30299859248107,24.6033305912352));
#18161=CARTESIAN_POINT('Ctrl Pts',(-2.95691885318268,1.28176447401976,24.6047593122509));
#18162=CARTESIAN_POINT('Ctrl Pts',(-2.9621060211994,1.26973114563209,24.6055693321315));
#18163=CARTESIAN_POINT('Ctrl Pts',(-2.97578197872324,1.23746538673076,24.6077424331641));
#18164=CARTESIAN_POINT('Ctrl Pts',(-2.98413766058743,1.21717761746544,24.609110013031));
#18165=CARTESIAN_POINT('Ctrl Pts',(-3.05384232050255,1.04290029460675,24.6208700248884));
#18166=CARTESIAN_POINT('Ctrl Pts',(-3.10342397328423,0.884498958261372,
24.6316591409857));
#18167=CARTESIAN_POINT('Ctrl Pts',(-3.19858321653192,0.471146846063818,
24.6599636844443));
#18168=CARTESIAN_POINT('Ctrl Pts',(-3.22605645590846,0.213236944793662,
24.6778163764528));
#18169=CARTESIAN_POINT('Ctrl Pts',(-3.22172401930047,-0.0957679684971617,
24.6979667566994));
#18170=CARTESIAN_POINT('Ctrl Pts',(-3.21982357415144,-0.146335201340634,
24.7012211786082));
#18171=CARTESIAN_POINT('Ctrl Pts',(-3.21604275273868,-0.208120908132821,
24.7051282270333));
#18172=CARTESIAN_POINT('Ctrl Pts',(-3.21529309003917,-0.219398390933108,
24.7058385276252));
#18173=CARTESIAN_POINT('Ctrl Pts',(-3.21402429071297,-0.237079501621139,
24.7069474576459));
#18174=CARTESIAN_POINT('Ctrl Pts',(-3.21354531693471,-0.243485788293864,
24.7073482816055));
#18175=CARTESIAN_POINT('Ctrl Pts',(-3.21261364118703,-0.255465099830885,
24.7080959297796));
#18176=CARTESIAN_POINT('Ctrl Pts',(-3.21216559704645,-0.261038316189161,
24.7084430012344));
#18177=CARTESIAN_POINT('Ctrl Pts',(-3.21110819325681,-0.273776251626151,
24.7092345413308));
#18178=CARTESIAN_POINT('Ctrl Pts',(-3.21048935919157,-0.280940103289656,
24.7096784717646));
#18179=CARTESIAN_POINT('Ctrl Pts',(-3.20850728258521,-0.30302312887516,
24.7110432743543));
#18180=CARTESIAN_POINT('Ctrl Pts',(-3.20706396082666,-0.31793516684402,
24.711959759517));
#18181=CARTESIAN_POINT('Ctrl Pts',(-3.19131590654687,-0.469602983688038,
24.7212338855888));
#18182=CARTESIAN_POINT('Ctrl Pts',(-3.16837484478286,-0.605338543827791,
24.7291446796844));
#18183=CARTESIAN_POINT('Ctrl Pts',(-3.07645205249276,-0.995412548454738,
24.7517891888525));
#18184=CARTESIAN_POINT('Ctrl Pts',(-2.98492084996148,-1.24324188511642,
24.7661457550968));
#18185=CARTESIAN_POINT('Ctrl Pts',(-2.82896886549267,-1.54563396641735,
24.7859969054275));
#18186=CARTESIAN_POINT('Ctrl Pts',(-2.79122723321879,-1.61279208315098,
24.7905614757138));
#18187=CARTESIAN_POINT('Ctrl Pts',(-2.74115883796554,-1.69485440751456,
24.7963681591959));
#18188=CARTESIAN_POINT('Ctrl Pts',(-2.73105412203849,-1.71108930091418,
24.7975284408806));
#18189=CARTESIAN_POINT('Ctrl Pts',(-2.71476026594254,-1.73675602643589,
24.7993816360599));
#18190=CARTESIAN_POINT('Ctrl Pts',(-2.70866495111433,-1.74624711149348,
24.8000710586049));
#18191=CARTESIAN_POINT('Ctrl Pts',(-2.69708500631615,-1.76407186918021,
24.8013737606688));
#18192=CARTESIAN_POINT('Ctrl Pts',(-2.69161124864599,-1.77241247273957,
24.8019866273004));
#18193=CARTESIAN_POINT('Ctrl Pts',(-2.67919474143217,-1.79114187815173,
24.8033703942696));
#18194=CARTESIAN_POINT('Ctrl Pts',(-2.67223015257595,-1.8015159435289,24.8041421137755));
#18195=CARTESIAN_POINT('Ctrl Pts',(-2.65427230438663,-1.82793169459387,
24.8061208047689));
#18196=CARTESIAN_POINT('Ctrl Pts',(-2.64319397347033,-1.84391467746543,
24.8073310015509));
#18197=CARTESIAN_POINT('Ctrl Pts',(-2.57560407308937,-1.93956748158224,
24.8146532787511));
#18198=CARTESIAN_POINT('Ctrl Pts',(-2.51564431600867,-2.01672723703995,
24.8208980368232));
#18199=CARTESIAN_POINT('Ctrl Pts',(-2.29286218676216,-2.27799627353853,
24.8432841146092));
#18200=CARTESIAN_POINT('Ctrl Pts',(-2.11260008273383,-2.44609423178966,
24.8600822154122));
#18201=CARTESIAN_POINT('Ctrl Pts',(-1.84204021754391,-2.64598590899664,
24.8827048183809));
#18202=CARTESIAN_POINT('Ctrl Pts',(-1.76679712149156,-2.69680994220845,
24.8887499449085));
#18203=CARTESIAN_POINT('Ctrl Pts',(-1.65046625954378,-2.76842558155146,
24.8976314203449));
#18204=CARTESIAN_POINT('Ctrl Pts',(-1.61091764544294,-2.79162388744239,
24.9005739217351));
#18205=CARTESIAN_POINT('Ctrl Pts',(-1.56131714403665,-2.81931311054701,
24.904157648408));
#18206=CARTESIAN_POINT('Ctrl Pts',(-1.55172175648461,-2.82460567835484,
24.9048460720236));
#18207=CARTESIAN_POINT('Ctrl Pts',(-1.53652518306164,-2.83288690619727,
24.9059284729544));
#18208=CARTESIAN_POINT('Ctrl Pts',(-1.53094194720685,-2.83590807633515,
24.9063244780817));
#18209=CARTESIAN_POINT('Ctrl Pts',(-1.52041282290657,-2.8415653820085,24.9070680905975));
#18210=CARTESIAN_POINT('Ctrl Pts',(-1.51546904594834,-2.84420508113547,
24.9074159157253));
#18211=CARTESIAN_POINT('Ctrl Pts',(-1.50416561272706,-2.85020264020476,
24.9082081927912));
#18212=CARTESIAN_POINT('Ctrl Pts',(-1.49780159394352,-2.85355211416973,
24.9086521101939));
#18213=CARTESIAN_POINT('Ctrl Pts',(-1.48604397850216,-2.859690144328,24.909468398825));
#18214=CARTESIAN_POINT('Ctrl Pts',(-1.48065364408144,-2.86248479733007,
24.9098411429068));
#18215=CARTESIAN_POINT('Ctrl Pts',(-1.47525540501177,-2.86526422036146,
24.9102129806979));
#18216=CARTESIAN_POINT('Origin',(0.,0.,4.68922655072688));
#18217=CARTESIAN_POINT('',(-1.47525541363878,-2.86526421591962,26.4061645232028));
#18218=CARTESIAN_POINT('',(-1.47525540475399,-2.86526422049419,26.1560859507638));
#18219=CARTESIAN_POINT('',(-1.47525540501186,-2.86526422036142,4.68922655072688));
#18220=CARTESIAN_POINT('Ctrl Pts',(-1.47525541363878,-2.86526421591962,
26.4061645232028));
#18221=CARTESIAN_POINT('Ctrl Pts',(-1.49437271054214,-2.85542118099316,
26.4049081860839));
#18222=CARTESIAN_POINT('Ctrl Pts',(-1.51339234256502,-2.84538638249555,
26.4036461231082));
#18223=CARTESIAN_POINT('Ctrl Pts',(-1.58152110791012,-2.8085650247018,26.3990792002463));
#18224=CARTESIAN_POINT('Ctrl Pts',(-1.6300275542405,-2.78069345911704,26.3957401893084));
#18225=CARTESIAN_POINT('Ctrl Pts',(-1.69243203781556,-2.74264211624054,
26.3913171978019));
#18226=CARTESIAN_POINT('Ctrl Pts',(-1.70701021100412,-2.73359252673386,
26.3902746625154));
#18227=CARTESIAN_POINT('Ctrl Pts',(-1.73068561384604,-2.71863247652253,
26.3885659991755));
#18228=CARTESIAN_POINT('Ctrl Pts',(-1.73982661520454,-2.71279165820974,
26.387902461847));
#18229=CARTESIAN_POINT('Ctrl Pts',(-1.75740785646367,-2.70143237511691,
26.3866187618656));
#18230=CARTESIAN_POINT('Ctrl Pts',(-1.7658520368185,-2.69592021982569,26.3859988406283));
#18231=CARTESIAN_POINT('Ctrl Pts',(-1.78521192476018,-2.68315257480135,
26.3845697149569));
#18232=CARTESIAN_POINT('Ctrl Pts',(-1.79610946193147,-2.67586997975815,
26.3837594943195));
#18233=CARTESIAN_POINT('Ctrl Pts',(-1.82513239980708,-2.6562173908634,26.3815859966515));
#18234=CARTESIAN_POINT('Ctrl Pts',(-1.84317614086882,-2.64372857525326,
26.3802182201753));
#18235=CARTESIAN_POINT('Ctrl Pts',(-1.99459951884756,-2.53661852262063,
26.368597475364));
#18236=CARTESIAN_POINT('Ctrl Pts',(-2.12070576701038,-2.43217047499999,
26.357958917567));
#18237=CARTESIAN_POINT('Ctrl Pts',(-2.42083720081386,-2.14243240948653,
26.3301372753071));
#18238=CARTESIAN_POINT('Ctrl Pts',(-2.58189619254346,-1.94532169329057,
26.3126277107222));
#18239=CARTESIAN_POINT('Ctrl Pts',(-2.74871538784876,-1.6834229981886,26.2923078985636));
#18240=CARTESIAN_POINT('Ctrl Pts',(-2.77798441571817,-1.63467207753564,
26.2886410349935));
#18241=CARTESIAN_POINT('Ctrl Pts',(-2.81170771435265,-1.5749775564791,26.2843112435461));
#18242=CARTESIAN_POINT('Ctrl Pts',(-2.81740967441512,-1.5647547126614,26.283575305766));
#18243=CARTESIAN_POINT('Ctrl Pts',(-2.82619781648782,-1.54879498095685,
26.2824352565669));
#18244=CARTESIAN_POINT('Ctrl Pts',(-2.82932244802206,-1.54307954359416,
26.282028748756));
#18245=CARTESIAN_POINT('Ctrl Pts',(-2.83509271784213,-1.53244836985969,
26.2812759348151));
#18246=CARTESIAN_POINT('Ctrl Pts',(-2.83774288742173,-1.52753527967774,
26.2809293479846));
#18247=CARTESIAN_POINT('Ctrl Pts',(-2.84371932136872,-1.51638647109498,
26.2801458325333));
#18248=CARTESIAN_POINT('Ctrl Pts',(-2.84703784000565,-1.51014669759899,
26.2797093988586));
#18249=CARTESIAN_POINT('Ctrl Pts',(-2.85681593115487,-1.49161426989157,
26.2784191897046));
#18250=CARTESIAN_POINT('Ctrl Pts',(-2.86321670628529,-1.47929054062845,
26.277569048921));
#18251=CARTESIAN_POINT('Ctrl Pts',(-2.91082968553497,-1.38615204423006,
26.2711998180889));
#18252=CARTESIAN_POINT('Ctrl Pts',(-2.94869692591549,-1.30366278618734,
26.2658737775924));
#18253=CARTESIAN_POINT('Ctrl Pts',(-3.07554994633257,-0.993411060313955,
26.2465909873751));
#18254=CARTESIAN_POINT('Ctrl Pts',(-3.14202378558033,-0.75734613622741,
26.2333069327312));
#18255=CARTESIAN_POINT('Ctrl Pts',(-3.19585665350666,-0.425478441997348,
26.2141647708085));
#18256=CARTESIAN_POINT('Ctrl Pts',(-3.20667074374613,-0.334353818609813,
26.2088697659733));
#18257=CARTESIAN_POINT('Ctrl Pts',(-3.21780506728464,-0.187044021619061,
26.2001582178935));
#18258=CARTESIAN_POINT('Ctrl Pts',(-3.22056964652205,-0.131093459642534,
26.1968148151285));
#18259=CARTESIAN_POINT('Ctrl Pts',(-3.22227486113773,-0.057939481492352,
26.1923868164082));
#18260=CARTESIAN_POINT('Ctrl Pts',(-3.22253776982305,-0.0407746068155915,
26.191343785054));
#18261=CARTESIAN_POINT('Ctrl Pts',(-3.22274300451921,-0.0127594163426344,
26.1896345131272));
#18262=CARTESIAN_POINT('Ctrl Pts',(-3.22276769618982,-0.00190990202893975,
26.1889708668458));
#18263=CARTESIAN_POINT('Ctrl Pts',(-3.22270963174659,0.0190228131898359,
26.187687099813));
#18264=CARTESIAN_POINT('Ctrl Pts',(-3.22263433849987,0.029105920484238,
26.1870672212501));
#18265=CARTESIAN_POINT('Ctrl Pts',(-3.22235239782335,0.0522902485944937,
26.1856384001866));
#18266=CARTESIAN_POINT('Ctrl Pts',(-3.22211316955261,0.0653908273462473,
26.1848284428948));
#18267=CARTESIAN_POINT('Ctrl Pts',(-3.22125996871502,0.10041258012561,26.1826561109859));
#18268=CARTESIAN_POINT('Ctrl Pts',(-3.22050213272348,0.122329256601399,
26.1812892444995));
#18269=CARTESIAN_POINT('Ctrl Pts',(-3.21213918072427,0.30900030424193,26.1695820796339));
#18270=CARTESIAN_POINT('Ctrl Pts',(-3.19212199837172,0.472928631508612,
26.1588492419612));
#18271=CARTESIAN_POINT('Ctrl Pts',(-3.10912343611939,0.886186050045341,
26.1307279401542));
#18272=CARTESIAN_POINT('Ctrl Pts',(-3.0287247347511,1.13083886826542,26.1130063861888));
#18273=CARTESIAN_POINT('Ctrl Pts',(-2.89775588321677,1.41135899989619,26.0927917337991));
#18274=CARTESIAN_POINT('Ctrl Pts',(-2.87416576400806,1.45879927303017,26.0893807721315));
#18275=CARTESIAN_POINT('Ctrl Pts',(-2.8440596043192,1.5157750299234,26.08531254131));
#18276=CARTESIAN_POINT('Ctrl Pts',(-2.83864982639682,1.52588208806886,26.0845919773385));
#18277=CARTESIAN_POINT('Ctrl Pts',(-2.83010687907828,1.54164015214328,26.0834705299127));
#18278=CARTESIAN_POINT('Ctrl Pts',(-2.82701051411813,1.54731084805639,26.0830673722838));
#18279=CARTESIAN_POINT('Ctrl Pts',(-2.82120413899288,1.55786905716693,26.082317551557));
#18280=CARTESIAN_POINT('Ctrl Pts',(-2.81849849832215,1.56275878137027,26.0819706278102));
#18281=CARTESIAN_POINT('Ctrl Pts',(-2.81230621662895,1.57388128789339,26.0811822257736));
#18282=CARTESIAN_POINT('Ctrl Pts',(-2.80881157552127,1.58010952152227,26.0807412682462));
#18283=CARTESIAN_POINT('Ctrl Pts',(-2.7996646739533,1.59628511584858,26.0795972624647));
#18284=CARTESIAN_POINT('Ctrl Pts',(-2.79398003779248,1.60621418719133,26.0788962450794));
#18285=CARTESIAN_POINT('Ctrl Pts',(-2.75699408722439,1.67002519823566,26.0743974479795));
#18286=CARTESIAN_POINT('Ctrl Pts',(-2.72418615432642,1.72302395019538,26.0706905155826));
#18287=CARTESIAN_POINT('Ctrl Pts',(-2.67099725941925,1.80362523847452,26.065046009274));
#18288=CARTESIAN_POINT('Ctrl Pts',(-2.65168003124508,1.83190706926713,26.0630640634911));
#18289=CARTESIAN_POINT('Ctrl Pts',(-2.49330237884658,2.05602762619528,26.0473021819558));
#18290=CARTESIAN_POINT('Ctrl Pts',(-2.33319286146725,2.23607459412244,26.0342366444799));
#18291=CARTESIAN_POINT('Ctrl Pts',(-2.08603228759355,2.45826706444388,26.0153175519517));
#18292=CARTESIAN_POINT('Ctrl Pts',(-2.01490339364569,2.51689690658847,26.0099996941659));
#18293=CARTESIAN_POINT('Ctrl Pts',(-1.89651154265684,2.60624617539733,26.0012539871689));
#18294=CARTESIAN_POINT('Ctrl Pts',(-1.85078334287712,2.63891561001192,25.9979000319302));
#18295=CARTESIAN_POINT('Ctrl Pts',(-1.78998559265168,2.67999338123181,25.9934600038957));
#18296=CARTESIAN_POINT('Ctrl Pts',(-1.77566816281349,2.68950097659732,25.9924157831253));
#18297=CARTESIAN_POINT('Ctrl Pts',(-1.75218593978261,2.70482528143308,25.9907050519338));
#18298=CARTESIAN_POINT('Ctrl Pts',(-1.7430664779944,2.71071109109505,25.9900411443617));
#18299=CARTESIAN_POINT('Ctrl Pts',(-1.72541925539808,2.72197494465727,25.9887572159145));
#18300=CARTESIAN_POINT('Ctrl Pts',(-1.71689563762671,2.72735926713962,25.9881374390785));
#18301=CARTESIAN_POINT('Ctrl Pts',(-1.69724507644035,2.7396437968091,25.9867093456047));
#18302=CARTESIAN_POINT('Ctrl Pts',(-1.68610112445136,2.74651633399251,25.9859000175483));
#18303=CARTESIAN_POINT('Ctrl Pts',(-1.65620977337386,2.76470001101707,25.9837304702251));
#18304=CARTESIAN_POINT('Ctrl Pts',(-1.63738871685967,2.77588816705966,25.9823657771605));
#18305=CARTESIAN_POINT('Ctrl Pts',(-1.47732507113802,2.86884357390341,25.9707692663852));
#18306=CARTESIAN_POINT('Ctrl Pts',(-1.33019516362041,2.93995223189422,25.960153437564));
#18307=CARTESIAN_POINT('Ctrl Pts',(-0.942959360718093,3.09206976477965,
25.9324097068884));
#18308=CARTESIAN_POINT('Ctrl Pts',(-0.697533641748336,3.15650272467688,
25.9149571458457));
#18309=CARTESIAN_POINT('Ctrl Pts',(-0.38972318356811,3.19962353091047,25.8946053717871));
#18310=CARTESIAN_POINT('Ctrl Pts',(-0.332130243342614,3.20611375231449,
25.8908661657931));
#18311=CARTESIAN_POINT('Ctrl Pts',(-0.262662480216537,3.21204989268341,
25.8864627831021));
#18312=CARTESIAN_POINT('Ctrl Pts',(-0.250929763105865,3.212987761519,25.8857227337543));
#18313=CARTESIAN_POINT('Ctrl Pts',(-0.232682182355056,3.21434583958339,
25.8845777138272));
#18314=CARTESIAN_POINT('Ctrl Pts',(-0.226170879295409,3.21481055578477,
25.884170313712));
#18315=CARTESIAN_POINT('Ctrl Pts',(-0.214090159539857,3.21563588007138,
25.883416687781));
#18316=CARTESIAN_POINT('Ctrl Pts',(-0.208521269174806,3.21600180203053,
25.88307017596));
#18317=CARTESIAN_POINT('Ctrl Pts',(-0.195917006706123,3.21679712875393,
25.8822878950178));
#18318=CARTESIAN_POINT('Ctrl Pts',(-0.188881177474731,3.21721791989632,
25.8818526142516));
#18319=CARTESIAN_POINT('Ctrl Pts',(-0.168068098858618,3.21839417361032,
25.8805689663746));
#18320=CARTESIAN_POINT('Ctrl Pts',(-0.154287108349068,3.21908425589985,
25.8797241792717));
#18321=CARTESIAN_POINT('Ctrl Pts',(-0.0523551337836735,3.22353240064719,
25.873510975362));
#18322=CARTESIAN_POINT('Ctrl Pts',(0.0359211975048042,3.22375788540087,
25.8683250717388));
#18323=CARTESIAN_POINT('Ctrl Pts',(0.371646429713838,3.21081998576538,25.8489730159192));
#18324=CARTESIAN_POINT('Ctrl Pts',(0.617272739477642,3.17277090328384,25.8355214044319));
#18325=CARTESIAN_POINT('Ctrl Pts',(0.944158300769834,3.08269696195949,25.8162124459223));
#18326=CARTESIAN_POINT('Ctrl Pts',(1.03111293246459,3.05471106301876,25.8109404613762));
#18327=CARTESIAN_POINT('Ctrl Pts',(1.16912857282546,3.00372650825073,25.8022633386962));
#18328=CARTESIAN_POINT('Ctrl Pts',(1.22098529756291,2.98302344792547,25.7989305863978));
#18329=CARTESIAN_POINT('Ctrl Pts',(1.28802998936638,2.95421568644553,25.7945147312533));
#18330=CARTESIAN_POINT('Ctrl Pts',(1.30372954555167,2.94732095807808,25.7934729039606));
#18331=CARTESIAN_POINT('Ctrl Pts',(1.32926776931012,2.93586143703773,25.7917651091758));
#18332=CARTESIAN_POINT('Ctrl Pts',(1.3391398651957,2.93137162381514,25.7911017273223));
#18333=CARTESIAN_POINT('Ctrl Pts',(1.35814802523645,2.92261068428971,25.7898181227612));
#18334=CARTESIAN_POINT('Ctrl Pts',(1.36728708424706,2.91834632899168,25.7891981403655));
#18335=CARTESIAN_POINT('Ctrl Pts',(1.38826279639535,2.90843874298913,25.7877685787723));
#18336=CARTESIAN_POINT('Ctrl Pts',(1.40008526271293,2.90276605370462,25.7869579813511));
#18337=CARTESIAN_POINT('Ctrl Pts',(1.43161731489114,2.88739880746558,25.784782815391));
#18338=CARTESIAN_POINT('Ctrl Pts',(1.4512626906602,2.8775747729237,25.7834137365536));
#18339=CARTESIAN_POINT('Ctrl Pts',(1.61819188513292,2.79195452590625,25.7716593513023));
#18340=CARTESIAN_POINT('Ctrl Pts',(1.75950712511285,2.70512006808577,25.7608779760199));
#18341=CARTESIAN_POINT('Ctrl Pts',(2.10278566920486,2.45587006619376,25.7325699925155));
#18342=CARTESIAN_POINT('Ctrl Pts',(2.29300298319346,2.27928474748005,25.7147045927497));
#18343=CARTESIAN_POINT('Ctrl Pts',(2.49268967147371,2.04332222545695,25.6945500088097));
#18344=CARTESIAN_POINT('Ctrl Pts',(2.52440207495043,2.00401156563133,25.6913018536659));
#18345=CARTESIAN_POINT('Ctrl Pts',(2.56206467587449,1.95501145997342,25.6874010961321));
#18346=CARTESIAN_POINT('Ctrl Pts',(2.56890286016903,1.94601729590215,25.6866910429428));
#18347=CARTESIAN_POINT('Ctrl Pts',(2.57955514038087,1.93185250882174,25.6855823265757));
#18348=CARTESIAN_POINT('Ctrl Pts',(2.58340123618463,1.92670622895617,25.6851814712272));
#18349=CARTESIAN_POINT('Ctrl Pts',(2.59056706332564,1.91705793870523,25.6844336530476));
#18350=CARTESIAN_POINT('Ctrl Pts',(2.5938904261035,1.91255883776215,25.6840864434813));
#18351=CARTESIAN_POINT('Ctrl Pts',(2.60146245635767,1.90225193655187,25.6832944359735));
#18352=CARTESIAN_POINT('Ctrl Pts',(2.60570338954346,1.8964385542495,25.6828501775964));
#18353=CARTESIAN_POINT('Ctrl Pts',(2.61872516459041,1.87846243151777,25.6814838357579));
#18354=CARTESIAN_POINT('Ctrl Pts',(2.62744073267527,1.86625234380372,25.6805661522207));
#18355=CARTESIAN_POINT('Ctrl Pts',(2.71641383109504,1.73974655704221,25.6711598212987));
#18356=CARTESIAN_POINT('Ctrl Pts',(2.78925709261912,1.62039414413956,25.6631322666994));
#18357=CARTESIAN_POINT('Ctrl Pts',(2.97876577006997,1.25900496468641,25.640089116359));
#18358=CARTESIAN_POINT('Ctrl Pts',(3.07321818239486,1.00671122790793,25.6254510885371));
#18359=CARTESIAN_POINT('Ctrl Pts',(3.15166239159618,0.676859120536802,25.6056083701586));
#18360=CARTESIAN_POINT('Ctrl Pts',(3.16574868803345,0.607575694019345,25.6014102747691));
#18361=CARTESIAN_POINT('Ctrl Pts',(3.18064994066027,0.519547459453553,25.5960148388657));
#18362=CARTESIAN_POINT('Ctrl Pts',(3.18359581662186,0.501179869437657,25.594885736852));
#18363=CARTESIAN_POINT('Ctrl Pts',(3.18805537691094,0.471746946906356,25.5930707229158));
#18364=CARTESIAN_POINT('Ctrl Pts',(3.18967087233505,0.460697286062864,25.5923880524716));
#18365=CARTESIAN_POINT('Ctrl Pts',(3.19262393919032,0.439738471302244,25.591090657871));
#18366=CARTESIAN_POINT('Ctrl Pts',(3.1939728895837,0.429831033367234,25.5904763030397));
#18367=CARTESIAN_POINT('Ctrl Pts',(3.19692897016848,0.407337350763026,25.5890789997735));
#18368=CARTESIAN_POINT('Ctrl Pts',(3.19850791154475,0.394747628261893,25.5882951677072));
#18369=CARTESIAN_POINT('Ctrl Pts',(3.20239255516062,0.36221867696752,25.5862652378278));
#18370=CARTESIAN_POINT('Ctrl Pts',(3.20458637018652,0.342266875186208,25.5850156266128));
#18371=CARTESIAN_POINT('Ctrl Pts',(3.21743641385172,0.214419066251236,25.5769781240502));
#18372=CARTESIAN_POINT('Ctrl Pts',(3.2228273664416,0.106075080822275,25.5700256830872));
#18373=CARTESIAN_POINT('Ctrl Pts',(3.22253004394657,-0.306044497767057,
25.5430379482098));
#18374=CARTESIAN_POINT('Ctrl Pts',(3.17938233664151,-0.608154744361235,
25.5219614943874));
#18375=CARTESIAN_POINT('Ctrl Pts',(3.07682501481297,-0.9608965408928,25.4978213706456));
#18376=CARTESIAN_POINT('Ctrl Pts',(3.05723242423208,-1.02152117786369,25.4936982065713));
#18377=CARTESIAN_POINT('Ctrl Pts',(3.03198943907334,-1.09237824555657,25.4889413528803));
#18378=CARTESIAN_POINT('Ctrl Pts',(3.02806643335732,-1.10320617952953,25.4882161867629));
#18379=CARTESIAN_POINT('Ctrl Pts',(3.02160887787926,-1.12073577615488,25.4870453056268));
#18380=CARTESIAN_POINT('Ctrl Pts',(3.0191099164248,-1.12745031186814,25.4865975541884));
#18381=CARTESIAN_POINT('Ctrl Pts',(3.01462115357479,-1.13938936104428,25.4858028075223));
#18382=CARTESIAN_POINT('Ctrl Pts',(3.01264013315002,-1.14461707371888,25.4854552959889));
#18383=CARTESIAN_POINT('Ctrl Pts',(3.00834582421124,-1.15586093790372,25.4847089125904));
#18384=CARTESIAN_POINT('Ctrl Pts',(3.00602809456509,-1.16187529547134,25.4843103119873));
#18385=CARTESIAN_POINT('Ctrl Pts',(2.99956368114646,-1.17850120194175,25.4832101015586));
#18386=CARTESIAN_POINT('Ctrl Pts',(2.9953786994894,-1.18909790006061,25.4825107569396));
#18387=CARTESIAN_POINT('Ctrl Pts',(2.97181891517139,-1.24783940086567,25.4786433417351));
#18388=CARTESIAN_POINT('Ctrl Pts',(2.95133834891464,-1.29553598827984,25.4755379483662));
#18389=CARTESIAN_POINT('Ctrl Pts',(2.82245084429516,-1.57675873404769,25.4573187184982));
#18390=CARTESIAN_POINT('Ctrl Pts',(2.68752086255833,-1.79712500200104,25.4433557999287));
#18391=CARTESIAN_POINT('Ctrl Pts',(2.42527693164959,-2.1287225013982,25.4194844173228));
#18392=CARTESIAN_POINT('Ctrl Pts',(2.31296150564206,-2.25025023270954,25.4099656748329));
#18393=CARTESIAN_POINT('Ctrl Pts',(2.17575163625645,-2.37754150098549,25.3987087397883));
#18394=CARTESIAN_POINT('Ctrl Pts',(2.15951824532447,-2.39229590210928,25.3973826054119));
#18395=CARTESIAN_POINT('Ctrl Pts',(2.1333485937216,-2.41559787128308,25.3952530454883));
#18396=CARTESIAN_POINT('Ctrl Pts',(2.1235084433974,-2.42425270566822,25.3944541372393));
#18397=CARTESIAN_POINT('Ctrl Pts',(2.10600369936517,-2.43946052695069,25.3930360372909));
#18398=CARTESIAN_POINT('Ctrl Pts',(2.09836057881077,-2.44603804588409,25.3924178777503));
#18399=CARTESIAN_POINT('Ctrl Pts',(2.08243068585523,-2.45961738807783,25.3911315560763));
#18400=CARTESIAN_POINT('Ctrl Pts',(2.07413918615,-2.46661344539334,25.3904631674521));
#18401=CARTESIAN_POINT('Ctrl Pts',(2.05263946229159,-2.48456905064676,25.3887328835356));
#18402=CARTESIAN_POINT('Ctrl Pts',(2.03937886019739,-2.4954650820639,25.3876684158016));
#18403=CARTESIAN_POINT('Ctrl Pts',(1.98250036970407,-2.54144510725271,25.3831136621017));
#18404=CARTESIAN_POINT('Ctrl Pts',(1.93806160108567,-2.57549365081135,25.3795822343522));
#18405=CARTESIAN_POINT('Ctrl Pts',(1.81858447788489,-2.66219222654825,25.370151814655));
#18406=CARTESIAN_POINT('Ctrl Pts',(1.74215191392776,-2.71282531005347,25.3641816828319));
#18407=CARTESIAN_POINT('Ctrl Pts',(1.45363185537698,-2.88673111548388,25.3418989449745));
#18408=CARTESIAN_POINT('Ctrl Pts',(1.22985105380373,-2.9889317710809,25.3250240770169));
#18409=CARTESIAN_POINT('Ctrl Pts',(0.910962818808793,-3.09263396318484,
25.3027303509747));
#18410=CARTESIAN_POINT('Ctrl Pts',(0.824126256946801,-3.11689865661018,
25.2968357138401));
#18411=CARTESIAN_POINT('Ctrl Pts',(0.722880128331746,-3.14066141647,25.2902488795338));
#18412=CARTESIAN_POINT('Ctrl Pts',(0.709360904013251,-3.14374250487621,
25.2893751749596));
#18413=CARTESIAN_POINT('Ctrl Pts',(0.68892575259181,-3.14826122686638,25.2880637304746));
#18414=CARTESIAN_POINT('Ctrl Pts',(0.682024499934543,-3.14976348777506,
25.2876224179387));
#18415=CARTESIAN_POINT('Ctrl Pts',(0.669660180402132,-3.15241240378854,
25.2868346589009));
#18416=CARTESIAN_POINT('Ctrl Pts',(0.66419904253405,-3.15356755980093,25.2864877320594));
#18417=CARTESIAN_POINT('Ctrl Pts',(0.652355374406069,-3.15604063653776,
25.2857375525362));
#18418=CARTESIAN_POINT('Ctrl Pts',(0.645971858863781,-3.15735338429617,
25.2853345981811));
#18419=CARTESIAN_POINT('Ctrl Pts',(0.628097095651578,-3.16097278824571,
25.2842100112925));
#18420=CARTESIAN_POINT('Ctrl Pts',(0.616597043908371,-3.16323616330999,
25.2834908116318));
#18421=CARTESIAN_POINT('Ctrl Pts',(0.548997496520677,-3.1761580613752,25.2792872152649));
#18422=CARTESIAN_POINT('Ctrl Pts',(0.492631200712093,-3.18538752932543,
25.2758790184597));
#18423=CARTESIAN_POINT('Ctrl Pts',(0.184918369037335,-3.22740819305677,
25.257652545334));
#18424=CARTESIAN_POINT('Ctrl Pts',(-0.0694002118302224,-3.23196052668063,
25.243896944248));
#18425=CARTESIAN_POINT('Ctrl Pts',(-0.484336893456944,-3.19034014590634,
25.2203396369695));
#18426=CARTESIAN_POINT('Ctrl Pts',(-0.645529871143418,-3.16166621710592,
25.2109164908922));
#18427=CARTESIAN_POINT('Ctrl Pts',(-0.825048781025056,-3.11542802100435,
25.1997665247601));
#18428=CARTESIAN_POINT('Ctrl Pts',(-0.846201556099869,-3.10974920778379,
25.1984424665445));
#18429=CARTESIAN_POINT('Ctrl Pts',(-0.879905957921855,-3.10033135925477,
25.196315611554));
#18430=CARTESIAN_POINT('Ctrl Pts',(-0.892495757754961,-3.09673058989817,
25.1955173137582));
#18431=CARTESIAN_POINT('Ctrl Pts',(-0.914739517777484,-3.09022180866905,
25.1940999203274));
#18432=CARTESIAN_POINT('Ctrl Pts',(-0.924402487324136,-3.08734501633968,
25.1934818534303));
#18433=CARTESIAN_POINT('Ctrl Pts',(-0.944439002983095,-3.08127738487787,
25.1921953484504));
#18434=CARTESIAN_POINT('Ctrl Pts',(-0.954810234245806,-3.07807939548043,
25.1915266820076));
#18435=CARTESIAN_POINT('Ctrl Pts',(-0.981559330887052,-3.06968306147691,
25.1897948703804));
#18436=CARTESIAN_POINT('Ctrl Pts',(-0.997911967463315,-3.06440606067968,
25.1887291441229));
#18437=CARTESIAN_POINT('Ctrl Pts',(-1.06752679241671,-3.04132502929298,
25.1841617047714));
#18438=CARTESIAN_POINT('Ctrl Pts',(-1.12035822226353,-3.02226209980034,
25.1806185642969));
#18439=CARTESIAN_POINT('Ctrl Pts',(-1.25841668476385,-2.96832968213159,
25.1711489156346));
#18440=CARTESIAN_POINT('Ctrl Pts',(-1.34268926780302,-2.93117325529551,
25.1651505293845));
#18441=CARTESIAN_POINT('Ctrl Pts',(-1.44199506580101,-2.88220685618616,
25.1578253909253));
#18442=CARTESIAN_POINT('Ctrl Pts',(-1.45866412097157,-2.87380667246934,
25.1565869376027));
#18443=CARTESIAN_POINT('Ctrl Pts',(-1.4752554489605,-2.86526419773332,25.1553455282223));
#18444=CARTESIAN_POINT('Ctrl Pts',(-1.47525540501177,-2.86526422036146,
24.9102129806979));
#18445=CARTESIAN_POINT('Ctrl Pts',(-1.47010109142369,-2.86791805204857,
24.9105680165818));
#18446=CARTESIAN_POINT('Ctrl Pts',(-1.46493957140812,-2.87055799903562,
24.9109222262282));
#18447=CARTESIAN_POINT('Ctrl Pts',(-1.39676361540044,-2.90519597405743,
24.9155837535852));
#18448=CARTESIAN_POINT('Ctrl Pts',(-1.33271501509627,-2.9351294004825,24.9197713314932));
#18449=CARTESIAN_POINT('Ctrl Pts',(-1.25829580640014,-2.96697059226284,
24.924478492948));
#18450=CARTESIAN_POINT('Ctrl Pts',(-1.24884357958254,-2.9709615529812,24.9250734888276));
#18451=CARTESIAN_POINT('Ctrl Pts',(-1.03636170021782,-3.05948335896664,
24.9383877171935));
#18452=CARTESIAN_POINT('Ctrl Pts',(-0.825215433198304,-3.12306210268755,
24.9504081753233));
#18453=CARTESIAN_POINT('Ctrl Pts',(-0.456167805628342,-3.19410767991887,
24.971602815464));
#18454=CARTESIAN_POINT('Ctrl Pts',(-0.301190365982923,-3.21242723253861,
24.9805496897514));
#18455=CARTESIAN_POINT('Ctrl Pts',(-0.111382936911088,-3.22100578062201,
24.9918991759716));
#18456=CARTESIAN_POINT('Ctrl Pts',(-0.0772374843166383,-3.22200537445344,
24.993955607795));
#18457=CARTESIAN_POINT('Ctrl Pts',(-0.0288775855290607,-3.22265193484467,
24.9968914380177));
#18458=CARTESIAN_POINT('Ctrl Pts',(-0.014670698650808,-3.22274792197344,
24.9977567530613));
#18459=CARTESIAN_POINT('Ctrl Pts',(0.00976608084689957,-3.22275143890781,
24.9992502250413));
#18460=CARTESIAN_POINT('Ctrl Pts',(0.0199958329956215,-3.22270420239774,
24.9998769529635));
#18461=CARTESIAN_POINT('Ctrl Pts',(0.0395335503398872,-3.22252095662318,
25.0010769230916));
#18462=CARTESIAN_POINT('Ctrl Pts',(0.0488415053722538,-3.22239332203931,
25.0016498956716));
#18463=CARTESIAN_POINT('Ctrl Pts',(0.0729413329623558,-3.22195841340573,
25.0031368326643));
#18464=CARTESIAN_POINT('Ctrl Pts',(0.0877317500108615,-3.22158960515778,
25.0040527219152));
#18465=CARTESIAN_POINT('Ctrl Pts',(0.137656959396089,-3.22000063003307,
25.0071558590937));
#18466=CARTESIAN_POINT('Ctrl Pts',(0.172773178415079,-3.21830743818157,
25.0093578761422));
#18467=CARTESIAN_POINT('Ctrl Pts',(0.475526297662532,-3.19874041866013,
25.0285162816521));
#18468=CARTESIAN_POINT('Ctrl Pts',(0.739943130008288,-3.14809363678248,
25.046554721667));
#18469=CARTESIAN_POINT('Ctrl Pts',(1.1670624026617,-3.00945485327862,25.0769473875398));
#18470=CARTESIAN_POINT('Ctrl Pts',(1.3341645479222,-2.93919601225401,25.0891515879971));
#18471=CARTESIAN_POINT('Ctrl Pts',(1.50922628807391,-2.84756559677658,25.1017027157977));
#18472=CARTESIAN_POINT('Ctrl Pts',(1.52389249379347,-2.8397439165504,25.1027521812782));
#18473=CARTESIAN_POINT('Ctrl Pts',(1.54508914626236,-2.82822795414327,25.104265258898));
#18474=CARTESIAN_POINT('Ctrl Pts',(1.55166795683564,-2.82462393690155,25.10473435378));
#18475=CARTESIAN_POINT('Ctrl Pts',(1.56316115830566,-2.81827543670574,25.1055528722427));
#18476=CARTESIAN_POINT('Ctrl Pts',(1.56808102009867,-2.81554100668402,25.1059029312325));
#18477=CARTESIAN_POINT('Ctrl Pts',(1.578445402496,-2.80974495076227,25.1066396744275));
#18478=CARTESIAN_POINT('Ctrl Pts',(1.5838881859675,-2.80668038667009,25.1070261655977));
#18479=CARTESIAN_POINT('Ctrl Pts',(1.59845537602588,-2.79842244798054,25.1080595875942));
#18480=CARTESIAN_POINT('Ctrl Pts',(1.60756346484215,-2.79320022557334,25.1087046844843));
#18481=CARTESIAN_POINT('Ctrl Pts',(1.6475532515346,-2.77001124730437,25.1115331455017));
#18482=CARTESIAN_POINT('Ctrl Pts',(1.67816181636323,-2.75157540169006,25.1136878253895));
#18483=CARTESIAN_POINT('Ctrl Pts',(1.71713325622863,-2.72721022269436,25.1164263224175));
#18484=CARTESIAN_POINT('Ctrl Pts',(1.72578183238854,-2.72174563293803,25.1170337372833));
#18485=CARTESIAN_POINT('Ctrl Pts',(1.98767207771296,-2.55452049905674,25.135422108806));
#18486=CARTESIAN_POINT('Ctrl Pts',(2.21710462046362,-2.35815812711824,25.1515142473993));
#18487=CARTESIAN_POINT('Ctrl Pts',(2.47460826050053,-2.06646250324366,25.1737018618524));
#18488=CARTESIAN_POINT('Ctrl Pts',(2.53042811490196,-1.99771997989967,25.1788192749131));
#18489=CARTESIAN_POINT('Ctrl Pts',(2.61598551955279,-1.88300768116648,25.1872645971845));
#18490=CARTESIAN_POINT('Ctrl Pts',(2.64750702368279,-1.83842437772233,25.1905250682591));
#18491=CARTESIAN_POINT('Ctrl Pts',(2.68734100232911,-1.77893369165561,25.1948582181709));
#18492=CARTESIAN_POINT('Ctrl Pts',(2.69669021677924,-1.76472904424039,25.1958915536155));
#18493=CARTESIAN_POINT('Ctrl Pts',(2.71179878197142,-1.74137354358707,25.1975887816865));
#18494=CARTESIAN_POINT('Ctrl Pts',(2.71762535161924,-1.732266404436,25.1982501486094));
#18495=CARTESIAN_POINT('Ctrl Pts',(2.72880226009761,-1.71460130941519,25.1995322305522));
#18496=CARTESIAN_POINT('Ctrl Pts',(2.7341584464433,-1.70604718897399,25.2001527181771));
#18497=CARTESIAN_POINT('Ctrl Pts',(2.74641569090647,-1.6862657239521,25.2015868778526));
#18498=CARTESIAN_POINT('Ctrl Pts',(2.75328820314347,-1.67502098529253,25.2024015910473));
#18499=CARTESIAN_POINT('Ctrl Pts',(2.77155127020434,-1.64472304151933,25.2045955053693));
#18500=CARTESIAN_POINT('Ctrl Pts',(2.7828140970968,-1.62559404152753,25.2059793415106));
#18501=CARTESIAN_POINT('Ctrl Pts',(2.88465072034203,-1.44847260779442,25.218782792207));
#18502=CARTESIAN_POINT('Ctrl Pts',(2.96186256586661,-1.28321197411695,25.2306855246905));
#18503=CARTESIAN_POINT('Ctrl Pts',(3.07170926747236,-0.984514746010875,
25.2520078567417));
#18504=CARTESIAN_POINT('Ctrl Pts',(3.11056663850006,-0.853838636210736,
25.2612689727067));
#18505=CARTESIAN_POINT('Ctrl Pts',(3.17476986617113,-0.574176488503076,
25.280631938811));
#18506=CARTESIAN_POINT('Ctrl Pts',(3.19815401276076,-0.425046380349274,
25.2906947173426));
#18507=CARTESIAN_POINT('Ctrl Pts',(3.21223363682343,-0.260533980371119,
25.3011560356797));
#18508=CARTESIAN_POINT('Ctrl Pts',(3.21336032413091,-0.246248528329243,
25.3020591401973));
#18509=CARTESIAN_POINT('Ctrl Pts',(3.21489996658276,-0.224912500200095,
25.3033995797485));
#18510=CARTESIAN_POINT('Ctrl Pts',(3.21538507255571,-0.21786754077303,25.3038408160532));
#18511=CARTESIAN_POINT('Ctrl Pts',(3.21621205365255,-0.205252833759815,
25.3046283827993));
#18512=CARTESIAN_POINT('Ctrl Pts',(3.21656262130947,-0.199683761425398,
25.304975193697));
#18513=CARTESIAN_POINT('Ctrl Pts',(3.21729106429761,-0.187611827915032,
25.3057250514247));
#18514=CARTESIAN_POINT('Ctrl Pts',(3.21766368898523,-0.181108742865714,
25.3061278005241));
#18515=CARTESIAN_POINT('Ctrl Pts',(3.21863421146345,-0.163221704695553,
25.3072324037904));
#18516=CARTESIAN_POINT('Ctrl Pts',(3.21919143563325,-0.151835509312136,
25.3079320140038));
#18517=CARTESIAN_POINT('Ctrl Pts',(3.2217089439719,-0.094122445573838,25.3114612795503));
#18518=CARTESIAN_POINT('Ctrl Pts',(3.22272978911153,-0.0477574733226213,
25.31424163644));
#18519=CARTESIAN_POINT('Ctrl Pts',(3.22285979380732,0.25498716482006,25.3321310784655));
#18520=CARTESIAN_POINT('Ctrl Pts',(3.19237868881762,0.510483406774052,25.346048409827));
#18521=CARTESIAN_POINT('Ctrl Pts',(3.09152430083769,0.926270538982161,25.3701712204234));
#18522=CARTESIAN_POINT('Ctrl Pts',(3.03789809185504,1.08934073481875,25.3800253101296));
#18523=CARTESIAN_POINT('Ctrl Pts',(2.96303239009753,1.2676919057717,25.3916579564016));
#18524=CARTESIAN_POINT('Ctrl Pts',(2.95429017678988,1.28793370444762,25.3929907891746));
#18525=CARTESIAN_POINT('Ctrl Pts',(2.94000966252351,1.32008836065332,25.3951289324715));
#18526=CARTESIAN_POINT('Ctrl Pts',(2.93460493502323,1.33206004481214,25.3959296654773));
#18527=CARTESIAN_POINT('Ctrl Pts',(2.92492113602611,1.3531650425915,25.3973497063676));
#18528=CARTESIAN_POINT('Ctrl Pts',(2.92067206725409,1.36231198935958,25.3979679710289));
#18529=CARTESIAN_POINT('Ctrl Pts',(2.91177153598466,1.38123907067606,25.3992532210831));
#18530=CARTESIAN_POINT('Ctrl Pts',(2.90711357713681,1.39101599314151,25.3999204264105));
#18531=CARTESIAN_POINT('Ctrl Pts',(2.89497895385345,1.41615904328004,25.4016448835219));
#18532=CARTESIAN_POINT('Ctrl Pts',(2.8874292648706,1.43148936473785,25.4027046765637));
#18533=CARTESIAN_POINT('Ctrl Pts',(2.85491583646753,1.49620700609004,25.4072146919106));
#18534=CARTESIAN_POINT('Ctrl Pts',(2.82880539939994,1.54500460773669,25.4107050646256));
#18535=CARTESIAN_POINT('Ctrl Pts',(2.75686399170324,1.67151268749512,25.419999024889));
#18536=CARTESIAN_POINT('Ctrl Pts',(2.70900648816065,1.74800892101746,25.4258712313088));
#18537=CARTESIAN_POINT('Ctrl Pts',(2.51508350619347,2.0308507388661,25.4485387622528));
#18538=CARTESIAN_POINT('Ctrl Pts',(2.34815043254383,2.22174985186993,25.465950338774));
#18539=CARTESIAN_POINT('Ctrl Pts',(2.09744719467626,2.44828252933649,25.4883716774367));
#18540=CARTESIAN_POINT('Ctrl Pts',(2.03200587536802,2.50286375834532,25.4939327530386));
#18541=CARTESIAN_POINT('Ctrl Pts',(1.95362912244848,2.56313049264066,25.5001933390471));
#18542=CARTESIAN_POINT('Ctrl Pts',(1.94273227991247,2.57139961394655,25.5010551361368));
#18543=CARTESIAN_POINT('Ctrl Pts',(1.9261627860281,2.58380800045034,25.502352160349));
#18544=CARTESIAN_POINT('Ctrl Pts',(1.92052887681625,2.58799839586592,25.5027908479605));
#18545=CARTESIAN_POINT('Ctrl Pts',(1.91039526410906,2.5954842714369,25.5035756820394));
#18546=CARTESIAN_POINT('Ctrl Pts',(1.90590068063647,2.59878649862991,25.503922294686));
#18547=CARTESIAN_POINT('Ctrl Pts',(1.89611379765902,2.60593799850107,25.5046738065878));
#18548=CARTESIAN_POINT('Ctrl Pts',(1.89081835604461,2.60978281317564,25.5050783968277));
#18549=CARTESIAN_POINT('Ctrl Pts',(1.87590046745913,2.62054487389166,25.5062125831724));
#18550=CARTESIAN_POINT('Ctrl Pts',(1.86625140679478,2.6274252980218,25.5069396778203));
#18551=CARTESIAN_POINT('Ctrl Pts',(1.80801314655396,2.66847037035459,25.5112906149421));
#18552=CARTESIAN_POINT('Ctrl Pts',(1.75852151529367,2.70134203194403,25.5148318784238));
#18553=CARTESIAN_POINT('Ctrl Pts',(1.49468842334272,2.86625005101672,25.533063955319));
#18554=CARTESIAN_POINT('Ctrl Pts',(1.26631592072286,2.97421458041884,25.5467295148741));
#18555=CARTESIAN_POINT('Ctrl Pts',(0.873432310175584,3.10639997962796,25.5701504681611));
#18556=CARTESIAN_POINT('Ctrl Pts',(0.71549007624331,3.14653277513683,25.5795321458239));
#18557=CARTESIAN_POINT('Ctrl Pts',(0.533651235126052,3.17833489656605,25.5906354450536));
#18558=CARTESIAN_POINT('Ctrl Pts',(0.512059641735634,3.18188485690694,25.591958292369));
#18559=CARTESIAN_POINT('Ctrl Pts',(0.477500013444488,3.18720607317653,25.5940834282585));
#18560=CARTESIAN_POINT('Ctrl Pts',(0.46455419742577,3.1891187192481,25.5948812276468));
#18561=CARTESIAN_POINT('Ctrl Pts',(0.441618644275081,3.19236465683933,25.5962978705928));
#18562=CARTESIAN_POINT('Ctrl Pts',(0.431633571066053,3.19373004273566,25.5969156873693));
#18563=CARTESIAN_POINT('Ctrl Pts',(0.410884725613852,3.19646821454506,25.5982018050918));
#18564=CARTESIAN_POINT('Ctrl Pts',(0.400120109974482,3.19783351619854,25.5988703349082));
#18565=CARTESIAN_POINT('Ctrl Pts',(0.372290697451221,3.2012204690819,25.6006020773233));
#18566=CARTESIAN_POINT('Ctrl Pts',(0.355216427234059,3.20316002198835,25.6016678722519));
#18567=CARTESIAN_POINT('Ctrl Pts',(0.282235045044691,3.2108596520424,25.6062381249456));
#18568=CARTESIAN_POINT('Ctrl Pts',(0.226200743915026,3.21529297381659,25.6097840811051));
#18569=CARTESIAN_POINT('Ctrl Pts',(0.0780347690067315,3.22312340359168,
25.6192637554885));
#18570=CARTESIAN_POINT('Ctrl Pts',(-0.0141710490152691,3.22403637401961,
25.6252695544228));
#18571=CARTESIAN_POINT('Ctrl Pts',(-0.346175018937811,3.21308129275034,
25.6472472935348));
#18572=CARTESIAN_POINT('Ctrl Pts',(-0.584407122278165,3.17839303284131,
25.6637485455824));
#18573=CARTESIAN_POINT('Ctrl Pts',(-0.848747723883929,3.10915606410736,
25.6819433555861));
#18574=CARTESIAN_POINT('Ctrl Pts',(-0.880795843332628,3.10022949799484,
25.6841458484747));
#18575=CARTESIAN_POINT('Ctrl Pts',(-0.973453389274151,3.07286816634295,
25.6904935795256));
#18576=CARTESIAN_POINT('Ctrl Pts',(-1.03366867620657,3.05313946555433,25.6945936825781));
#18577=CARTESIAN_POINT('Ctrl Pts',(-1.10408097369853,3.02774749603523,25.6993270957404));
#18578=CARTESIAN_POINT('Ctrl Pts',(-1.11487353984538,3.02379012097276,25.7000508940034));
#18579=CARTESIAN_POINT('Ctrl Pts',(-1.13235076515305,3.01727534777119,25.7012199258521));
#18580=CARTESIAN_POINT('Ctrl Pts',(-1.13904837306857,3.01475332088161,25.701667186482));
#18581=CARTESIAN_POINT('Ctrl Pts',(-1.15096053372758,3.01022235690101,25.7024612889562));
#18582=CARTESIAN_POINT('Ctrl Pts',(-1.15617830516967,3.00822215212013,25.7028086448979));
#18583=CARTESIAN_POINT('Ctrl Pts',(-1.16740437658695,3.00388517459287,25.7035549417811));
#18584=CARTESIAN_POINT('Ctrl Pts',(-1.1734108584724,3.00154394929566,25.7039536103394));
#18585=CARTESIAN_POINT('Ctrl Pts',(-1.19002360054986,2.99501109395673,25.7050545931568));
#18586=CARTESIAN_POINT('Ctrl Pts',(-1.20061482088088,2.99078111598788,25.7057546359492));
#18587=CARTESIAN_POINT('Ctrl Pts',(-1.25947415259899,2.96691050650974,25.7096357679536));
#18588=CARTESIAN_POINT('Ctrl Pts',(-1.30728588202886,2.94615638373286,25.7127536468805));
#18589=CARTESIAN_POINT('Ctrl Pts',(-1.58793357505434,2.81615428020016,25.7309669342036));
#18590=CARTESIAN_POINT('Ctrl Pts',(-1.80753628552859,2.68050371676083,25.7449160392112));
#18591=CARTESIAN_POINT('Ctrl Pts',(-2.1379570022102,2.41714328814122,25.7687743877321));
#18592=CARTESIAN_POINT('Ctrl Pts',(-2.25908622280888,2.30433517592237,25.7782955072118));
#18593=CARTESIAN_POINT('Ctrl Pts',(-2.38587579809243,2.16660916269908,25.789554807394));
#18594=CARTESIAN_POINT('Ctrl Pts',(-2.40056498196974,2.15032237553653,25.7908806926979));
#18595=CARTESIAN_POINT('Ctrl Pts',(-2.42376126730017,2.12406933128858,25.7930097866939));
#18596=CARTESIAN_POINT('Ctrl Pts',(-2.43237597160157,2.11419874415947,25.793808479411));
#18597=CARTESIAN_POINT('Ctrl Pts',(-2.44751206631606,2.09664109027487,25.7952261561976));
#18598=CARTESIAN_POINT('Ctrl Pts',(-2.45405806216484,2.08897539479246,25.7958441084824));
#18599=CARTESIAN_POINT('Ctrl Pts',(-2.46757135054734,2.07299946793814,25.7971299576332));
#18600=CARTESIAN_POINT('Ctrl Pts',(-2.47453286803614,2.06468453874194,25.7977980806337));
#18601=CARTESIAN_POINT('Ctrl Pts',(-2.49239810925198,2.04312591689781,25.7995275860462));
#18602=CARTESIAN_POINT('Ctrl Pts',(-2.50323818480358,2.02983014538208,25.8005915381517));
#18603=CARTESIAN_POINT('Ctrl Pts',(-2.5489700786539,1.972814722008,25.8051432101366));
#18604=CARTESIAN_POINT('Ctrl Pts',(-2.58282488921608,1.92827937503314,25.8086720100585));
#18605=CARTESIAN_POINT('Ctrl Pts',(-2.66899821100947,1.80857680826852,25.8180942181685));
#18606=CARTESIAN_POINT('Ctrl Pts',(-2.71929870977416,1.73202585282671,25.8240586253813));
#18607=CARTESIAN_POINT('Ctrl Pts',(-2.89251861697601,1.44222279007025,25.8463898010553));
#18608=CARTESIAN_POINT('Ctrl Pts',(-2.99414926742237,1.21726135352744,25.8633242131051));
#18609=CARTESIAN_POINT('Ctrl Pts',(-3.09648059811592,0.897736045159045,
25.88562480691));
#18610=CARTESIAN_POINT('Ctrl Pts',(-3.12021129328243,0.811422677912189,
25.8914757642803));
#18611=CARTESIAN_POINT('Ctrl Pts',(-3.14343081987345,0.710740297192464,
25.8980198175318));
#18612=CARTESIAN_POINT('Ctrl Pts',(-3.14645400196757,0.697234766103892,
25.8988918562314));
#18613=CARTESIAN_POINT('Ctrl Pts',(-3.15088703937895,0.676814754007573,
25.9002012071683));
#18614=CARTESIAN_POINT('Ctrl Pts',(-3.15236129430654,0.669914635291291,
25.900642076693));
#18615=CARTESIAN_POINT('Ctrl Pts',(-3.1549607840734,0.657549348745187,25.9014292489397));
#18616=CARTESIAN_POINT('Ctrl Pts',(-3.15609449370041,0.652086070591065,
25.9017760300653));
#18617=CARTESIAN_POINT('Ctrl Pts',(-3.15852181317187,0.640234333613007,
25.9025261201796));
#18618=CARTESIAN_POINT('Ctrl Pts',(-3.15981022901334,0.633844905808195,
25.9029291298352));
#18619=CARTESIAN_POINT('Ctrl Pts',(-3.16336323487426,0.615944984740043,
25.9040544250691));
#18620=CARTESIAN_POINT('Ctrl Pts',(-3.16558440157427,0.604425831967209,
25.9047742717628));
#18621=CARTESIAN_POINT('Ctrl Pts',(-3.17828981901766,0.536542783782793,
25.908992360624));
#18622=CARTESIAN_POINT('Ctrl Pts',(-3.18733217787319,0.479915472416386,
25.9124137784638));
#18623=CARTESIAN_POINT('Ctrl Pts',(-3.22809801298606,0.172070089679958,
25.9306354520374));
#18624=CARTESIAN_POINT('Ctrl Pts',(-3.23164476085394,-0.0819980360926485,
25.944377519278));
#18625=CARTESIAN_POINT('Ctrl Pts',(-3.18846563613236,-0.496535652854962,
25.9679212632499));
#18626=CARTESIAN_POINT('Ctrl Pts',(-3.15917021131018,-0.657642721423987,
25.9773458373937));
#18627=CARTESIAN_POINT('Ctrl Pts',(-3.11223764979869,-0.837002902610053,
25.9884971058933));
#18628=CARTESIAN_POINT('Ctrl Pts',(-3.10647887204644,-0.858129377821875,
25.9898208961599));
#18629=CARTESIAN_POINT('Ctrl Pts',(-3.09693401816565,-0.891789562433464,
25.99194726066));
#18630=CARTESIAN_POINT('Ctrl Pts',(-3.09328601480736,-0.904361962489312,
25.9927453374005));
#18631=CARTESIAN_POINT('Ctrl Pts',(-3.0866940265825,-0.926573866471151,
25.99416230124));
#18632=CARTESIAN_POINT('Ctrl Pts',(-3.08378121439741,-0.936222495901261,
25.9947801600045));
#18633=CARTESIAN_POINT('Ctrl Pts',(-3.07763913691372,-0.956228321906986,
25.9960661939311));
#18634=CARTESIAN_POINT('Ctrl Pts',(-3.07440274083129,-0.966583179680249,
25.9967345971128));
#18635=CARTESIAN_POINT('Ctrl Pts',(-3.06590786355911,-0.993288232785968,
25.9984656432495));
#18636=CARTESIAN_POINT('Ctrl Pts',(-3.06057090491577,-1.00961292523463,
25.9995308645988));
#18637=CARTESIAN_POINT('Ctrl Pts',(-3.0372392983666,-1.0790942603101,26.0040953258754));
#18638=CARTESIAN_POINT('Ctrl Pts',(-3.01798922051134,-1.13181597626786,
26.0076359335564));
#18639=CARTESIAN_POINT('Ctrl Pts',(-2.96357926822258,-1.26955766709326,
26.017097678874));
#18640=CARTESIAN_POINT('Ctrl Pts',(-2.92614057401631,-1.35361647611715,
26.0230905587328));
#18641=CARTESIAN_POINT('Ctrl Pts',(-2.77725904504195,-1.65275378951183,
26.0451955829062));
#18642=CARTESIAN_POINT('Ctrl Pts',(-2.64527698026023,-1.85667921391031,
26.0618502977985));
#18643=CARTESIAN_POINT('Ctrl Pts',(-2.43301822012873,-2.11544433817904,
26.0841211590778));
#18644=CARTESIAN_POINT('Ctrl Pts',(-2.37126342539103,-2.18444401198808,
26.090180373709));
#18645=CARTESIAN_POINT('Ctrl Pts',(-2.29687918883406,-2.26067645077101,
26.0969269963779));
#18646=CARTESIAN_POINT('Ctrl Pts',(-2.28707548880475,-2.27059413991579,
26.0978057703499));
#18647=CARTESIAN_POINT('Ctrl Pts',(-2.27219884906777,-2.28544963957684,
26.0991232205506));
#18648=CARTESIAN_POINT('Ctrl Pts',(-2.26717366077266,-2.29043473142491,
26.0995655183789));
#18649=CARTESIAN_POINT('Ctrl Pts',(-2.25815671478434,-2.29932097921762,
26.1003542291657));
#18650=CARTESIAN_POINT('Ctrl Pts',(-2.25417122301862,-2.3032283457979,26.1007011285181));
#18651=CARTESIAN_POINT('Ctrl Pts',(-2.24552123316595,-2.31166481612752,
26.1014503241284));
#18652=CARTESIAN_POINT('Ctrl Pts',(-2.24085318901503,-2.31619015146988,
26.1018523272533));
#18653=CARTESIAN_POINT('Ctrl Pts',(-2.22777861075561,-2.32878849725721,
26.1029719718064));
#18654=CARTESIAN_POINT('Ctrl Pts',(-2.21934182922676,-2.33683017316534,
26.1036872137409));
#18655=CARTESIAN_POINT('Ctrl Pts',(-2.17007105831757,-2.38328600668653,
26.1078236783229));
#18656=CARTESIAN_POINT('Ctrl Pts',(-2.12828112889404,-2.42067777856386,
26.1111715035696));
#18657=CARTESIAN_POINT('Ctrl Pts',(-1.89832407643467,-2.6158713245219,26.1288857019329));
#18658=CARTESIAN_POINT('Ctrl Pts',(-1.69357044304955,-2.75285907548838,
26.1422438874597));
#18659=CARTESIAN_POINT('Ctrl Pts',(-1.47525540475399,-2.86526422049419,
26.1560859507638));
#18660=CARTESIAN_POINT('Origin',(0.,0.,4.68922655072688));
#18661=CARTESIAN_POINT('',(-1.47525554463415,-2.86526414847326,27.6514736540563));
#18662=CARTESIAN_POINT('',(-1.47306432504218,-2.86105893806618,27.4070470808673));
#18663=CARTESIAN_POINT('',(-1.47525540501186,-2.86526422036142,4.68922655072688));
#18664=CARTESIAN_POINT('',(3.22274925660414,0.00218896264416769,26.8128035160936));
#18665=CARTESIAN_POINT('Ctrl Pts',(-1.47525554463428,-2.8652641484732,27.6514736540563));
#18666=CARTESIAN_POINT('Ctrl Pts',(-1.65781619981529,-2.77126806126031,
27.6397127301564));
#18667=CARTESIAN_POINT('Ctrl Pts',(-1.8310890777546,-2.65998124407618,27.6284558794886));
#18668=CARTESIAN_POINT('Ctrl Pts',(-2.12150031454677,-2.43150621874824,
27.6075843331467));
#18669=CARTESIAN_POINT('Ctrl Pts',(-2.24239055477045,-2.32048706666372,
27.5981388813136));
#18670=CARTESIAN_POINT('Ctrl Pts',(-2.3692664448582,-2.1847595100256,27.586963964455));
#18671=CARTESIAN_POINT('Ctrl Pts',(-2.38406442299321,-2.16860194459106,
27.585639418676));
#18672=CARTESIAN_POINT('Ctrl Pts',(-2.40744299694422,-2.1425469215207,27.5835119284357));
#18673=CARTESIAN_POINT('Ctrl Pts',(-2.41613015887314,-2.13274568148426,
27.5827134872523));
#18674=CARTESIAN_POINT('Ctrl Pts',(-2.43139879995696,-2.11530591056285,
27.5812959279024));
#18675=CARTESIAN_POINT('Ctrl Pts',(-2.43800466632634,-2.10768889141537,
27.5806778392771));
#18676=CARTESIAN_POINT('Ctrl Pts',(-2.4516461706162,-2.09180935662655,27.5793913775149));
#18677=CARTESIAN_POINT('Ctrl Pts',(-2.45867602606526,-2.08354206211609,
27.5787227764574));
#18678=CARTESIAN_POINT('Ctrl Pts',(-2.47672561001715,-2.06209672629191,
27.5769913243568));
#18679=CARTESIAN_POINT('Ctrl Pts',(-2.48768186026355,-2.04886593011761,
27.5759258942726));
#18680=CARTESIAN_POINT('Ctrl Pts',(-2.53397552710368,-1.99204281909594,
27.5713614434812));
#18681=CARTESIAN_POINT('Ctrl Pts',(-2.56827512270222,-1.94762132366348,
27.5678210627718));
#18682=CARTESIAN_POINT('Ctrl Pts',(-2.65568252578835,-1.82809350382125,
27.5583606627113));
#18683=CARTESIAN_POINT('Ctrl Pts',(-2.70676205448498,-1.75157420410728,
27.5523689397276));
#18684=CARTESIAN_POINT('Ctrl Pts',(-2.88022666122077,-1.46597166777845,
27.53026304279));
#18685=CARTESIAN_POINT('Ctrl Pts',(-2.98220811835585,-1.2454711537758,27.5136060344059));
#18686=CARTESIAN_POINT('Ctrl Pts',(-3.08768649294699,-0.927831165239926,
27.491334533395));
#18687=CARTESIAN_POINT('Ctrl Pts',(-3.11305367507109,-0.838796060182682,
27.4852767118327));
#18688=CARTESIAN_POINT('Ctrl Pts',(-3.1377963425146,-0.735218477075609,
27.4785312208174));
#18689=CARTESIAN_POINT('Ctrl Pts',(-3.14094892689835,-0.721631451156521,
27.4776522796681));
#18690=CARTESIAN_POINT('Ctrl Pts',(-3.14556877668978,-0.70111679772442,
27.4763345385518));
#18691=CARTESIAN_POINT('Ctrl Pts',(-3.14710153516616,-0.694204308950701,
27.475892115906));
#18692=CARTESIAN_POINT('Ctrl Pts',(-3.14980221429636,-0.681831904779727,
27.4751031606674));
#18693=CARTESIAN_POINT('Ctrl Pts',(-3.15097873466117,-0.676373972630644,
27.4747561415229));
#18694=CARTESIAN_POINT('Ctrl Pts',(-3.15349513424233,-0.664551205778928,
27.4740066553424));
#18695=CARTESIAN_POINT('Ctrl Pts',(-3.1548299272449,-0.658185383245754,
27.4736044818195));
#18696=CARTESIAN_POINT('Ctrl Pts',(-3.15850403298194,-0.640395054282058,
27.4724842780107));
#18697=CARTESIAN_POINT('Ctrl Pts',(-3.16080065070426,-0.628961690493888,
27.4717686500512));
#18698=CARTESIAN_POINT('Ctrl Pts',(-3.17378873323489,-0.562434234991849,
27.4676282369089));
#18699=CARTESIAN_POINT('Ctrl Pts',(-3.18310239484079,-0.507077135994187,
27.4642770033284));
#18700=CARTESIAN_POINT('Ctrl Pts',(-3.22657605741547,-0.199828863328797,
27.446053902051));
#18701=CARTESIAN_POINT('Ctrl Pts',(-3.23229104254463,0.0551957693487739,
27.4322607795362));
#18702=CARTESIAN_POINT('Ctrl Pts',(-3.19229938154424,0.471373402217451,
27.4086447978982));
#18703=CARTESIAN_POINT('Ctrl Pts',(-3.16421096649143,0.633029812475711,
27.399202322738));
#18704=CARTESIAN_POINT('Ctrl Pts',(-3.11857454046651,0.813074652908923,
27.388030735815));
#18705=CARTESIAN_POINT('Ctrl Pts',(-3.11297519364108,0.834255933821996,
27.3867062549834));
#18706=CARTESIAN_POINT('Ctrl Pts',(-3.10368431314574,0.868005052095016,
27.3845788493627));
#18707=CARTESIAN_POINT('Ctrl Pts',(-3.10013130601678,0.880610562982961,
27.3837804272787));
#18708=CARTESIAN_POINT('Ctrl Pts',(-3.09370721945747,0.902881420213494,
27.3823628900305));
#18709=CARTESIAN_POINT('Ctrl Pts',(-3.09086741519973,0.912555662234955,
27.3817448043006));
#18710=CARTESIAN_POINT('Ctrl Pts',(-3.08487683176028,0.932614746954922,
27.3804583367874));
#18711=CARTESIAN_POINT('Ctrl Pts',(-3.08171890510906,0.94299730574905,27.3797897270251));
#18712=CARTESIAN_POINT('Ctrl Pts',(-3.07342671183496,0.969773645987834,
27.3780582270596));
#18713=CARTESIAN_POINT('Ctrl Pts',(-3.06821374650669,0.986142517489724,
27.3769927575448));
#18714=CARTESIAN_POINT('Ctrl Pts',(-3.04541302715994,1.05580618511765,27.3724279089894));
#18715=CARTESIAN_POINT('Ctrl Pts',(-3.026566509117,1.1086756664749,27.3688871609821));
#18716=CARTESIAN_POINT('Ctrl Pts',(-2.97321351935743,1.24682770039801,27.3594255302163));
#18717=CARTESIAN_POINT('Ctrl Pts',(-2.9364213816863,1.33116674010156,27.3534329206279));
#18718=CARTESIAN_POINT('Ctrl Pts',(-2.78988411921005,1.63133627184148,27.3313351882926));
#18719=CARTESIAN_POINT('Ctrl Pts',(-2.65953566533557,1.83618261639722,27.3146880981289));
#18720=CARTESIAN_POINT('Ctrl Pts',(-2.44930034128831,2.09657509953146,27.2924174543771));
#18721=CARTESIAN_POINT('Ctrl Pts',(-2.38801935173462,2.16611780864668,27.2863520406239));
#18722=CARTESIAN_POINT('Ctrl Pts',(-2.31415464812323,2.24298918048435,27.2795991817342));
#18723=CARTESIAN_POINT('Ctrl Pts',(-2.30442290956503,2.25298630036574,27.2787200049193));
#18724=CARTESIAN_POINT('Ctrl Pts',(-2.28965423258522,2.26796190428536,27.2774019805127));
#18725=CARTESIAN_POINT('Ctrl Pts',(-2.28466545230893,2.27298734650806,27.2769595079822));
#18726=CARTESIAN_POINT('Ctrl Pts',(-2.27571351294254,2.28194582390838,27.2761704989037));
#18727=CARTESIAN_POINT('Ctrl Pts',(-2.27175667287515,2.28588502708855,27.275823475525));
#18728=CARTESIAN_POINT('Ctrl Pts',(-2.26316860777285,2.2943904881566,27.2750740201062));
#18729=CARTESIAN_POINT('Ctrl Pts',(-2.25853380585969,2.29895300276161,27.2746718813645));
#18730=CARTESIAN_POINT('Ctrl Pts',(-2.24555188109058,2.3116553030422,27.2735518726754));
#18731=CARTESIAN_POINT('Ctrl Pts',(-2.23717425257016,2.31976396731924,27.2728364036987));
#18732=CARTESIAN_POINT('Ctrl Pts',(-2.18824664750787,2.36660916822393,27.2686987739655));
#18733=CARTESIAN_POINT('Ctrl Pts',(-2.14673239669259,2.40433010348607,27.2653500492854));
#18734=CARTESIAN_POINT('Ctrl Pts',(-1.91170920050757,2.60693476467362,27.2471270757482));
#18735=CARTESIAN_POINT('Ctrl Pts',(-1.70018623211788,2.74956997773852,27.2333322852882));
#18736=CARTESIAN_POINT('Ctrl Pts',(-1.32836325871861,2.94081940147733,27.2097146712626));
#18737=CARTESIAN_POINT('Ctrl Pts',(-1.17716375683939,3.00453702726673,27.2002723556666));
#18738=CARTESIAN_POINT('Ctrl Pts',(-1.00100026283659,3.06342887193728,27.1891003750793));
#18739=CARTESIAN_POINT('Ctrl Pts',(-0.980142726357965,3.07016582275797,
27.1877753174509));
#18740=CARTESIAN_POINT('Ctrl Pts',(-0.946712647478207,3.08058830796385,
27.1856471603357));
#18741=CARTESIAN_POINT('Ctrl Pts',(-0.934183307509532,3.08441091621679,
27.1848485686419));
#18742=CARTESIAN_POINT('Ctrl Pts',(-0.911969338819483,3.09104046441739,
27.1834308351092));
#18743=CARTESIAN_POINT('Ctrl Pts',(-0.902294133196074,3.09387855630155,
27.1828127236548));
#18744=CARTESIAN_POINT('Ctrl Pts',(-0.882179360938241,3.09967657697798,
27.1815263071502));
#18745=CARTESIAN_POINT('Ctrl Pts',(-0.871737858464647,3.10262927341308,
27.1808577746406));
#18746=CARTESIAN_POINT('Ctrl Pts',(-0.844733051331343,3.11011873696422,
27.1791266994719));
#18747=CARTESIAN_POINT('Ctrl Pts',(-0.828148201914945,3.11457589782154,
27.1780615799017));
#18748=CARTESIAN_POINT('Ctrl Pts',(-0.757264618021113,3.13301960038357,
27.1735002602618));
#18749=CARTESIAN_POINT('Ctrl Pts',(-0.702644190887562,3.14571963497021,
27.1699627707197));
#18750=CARTESIAN_POINT('Ctrl Pts',(-0.557733315106304,3.17545117037993,
27.1605120560273));
#18751=CARTESIAN_POINT('Ctrl Pts',(-0.467002854492969,3.19005680256146,
27.1545273096502));
#18752=CARTESIAN_POINT('Ctrl Pts',(-0.13418607197542,3.22913041977734,27.1323597384297));
#18753=CARTESIAN_POINT('Ctrl Pts',(0.109815592445874,3.2300487079109,27.1156274520607));
#18754=CARTESIAN_POINT('Ctrl Pts',(0.44271860617565,3.19351266656144,27.0933490476567));
#18755=CARTESIAN_POINT('Ctrl Pts',(0.533393435017489,3.17962540915764,27.0873484228968));
#18756=CARTESIAN_POINT('Ctrl Pts',(0.637017339159052,3.15919613512662,27.0806584777717));
#18757=CARTESIAN_POINT('Ctrl Pts',(0.650656520955948,3.1564152798355,27.0797813347808));
#18758=CARTESIAN_POINT('Ctrl Pts',(0.671199908990393,3.15208792549332,27.078465755437));
#18759=CARTESIAN_POINT('Ctrl Pts',(0.678117533000828,3.15060696082114,27.0780237136284));
#18760=CARTESIAN_POINT('Ctrl Pts',(0.690485545853977,3.14791652388995,27.0772351691785));
#18761=CARTESIAN_POINT('Ctrl Pts',(0.695937700745256,3.1467156605998,27.0768881821161));
#18762=CARTESIAN_POINT('Ctrl Pts',(0.707739386280071,3.1440841090703,27.0761384599764));
#18763=CARTESIAN_POINT('Ctrl Pts',(0.714087692662342,3.14264835652323,27.0757360200563));
#18764=CARTESIAN_POINT('Ctrl Pts',(0.731817595176636,3.13858200917598,27.0746143214456));
#18765=CARTESIAN_POINT('Ctrl Pts',(0.743189439121718,3.135908718099,27.0738974754793));
#18766=CARTESIAN_POINT('Ctrl Pts',(0.809431389883048,3.11995599682877,27.0697356565637));
#18767=CARTESIAN_POINT('Ctrl Pts',(0.863963231513516,3.10529757549453,27.0663651268802));
#18768=CARTESIAN_POINT('Ctrl Pts',(1.16149695882205,3.01687330508875,27.0481409843214));
#18769=CARTESIAN_POINT('Ctrl Pts',(1.39552806495163,2.91601239501047,27.0343606466419));
#18770=CARTESIAN_POINT('Ctrl Pts',(1.75693146033795,2.70667619707327,27.0107689084841));
#18771=CARTESIAN_POINT('Ctrl Pts',(1.89208228380004,2.6139851596062,27.0013374462024));
#18772=CARTESIAN_POINT('Ctrl Pts',(2.03670462064768,2.49768565046564,26.9901755756113));
#18773=CARTESIAN_POINT('Ctrl Pts',(2.05366783180704,2.48375677561358,26.9888486957158));
#18774=CARTESIAN_POINT('Ctrl Pts',(2.08053237720843,2.46123432875514,26.9867181645616));
#18775=CARTESIAN_POINT('Ctrl Pts',(2.09052603392217,2.45275157469747,26.9859190371874));
#18776=CARTESIAN_POINT('Ctrl Pts',(2.10811572221947,2.43763560804012,26.9845006835427));
#18777=CARTESIAN_POINT('Ctrl Pts',(2.11573293645051,2.43102723016447,26.983882490659));
#18778=CARTESIAN_POINT('Ctrl Pts',(2.12363994420259,2.42410212903047,26.9832365843784));
#18779=CARTESIAN_POINT('Ctrl Pts',(2.12396089129666,2.42382092507454,26.9832103596731));
#18780=CARTESIAN_POINT('Ctrl Pts',(2.12448388156465,2.42336251347108,26.9831676141479));
#18781=CARTESIAN_POINT('Ctrl Pts',(2.12468595658513,2.42318534590571,26.9831510950932));
#18782=CARTESIAN_POINT('Ctrl Pts',(2.12501667403802,2.42289531900333,26.9831240551864));
#18783=CARTESIAN_POINT('Ctrl Pts',(2.12514533144021,2.42278247311706,26.9831135348179));
#18784=CARTESIAN_POINT('Ctrl Pts',(2.12544085444423,2.42252322714103,26.9830893671044));
#18785=CARTESIAN_POINT('Ctrl Pts',(2.12560771661837,2.42237681767885,26.983075719244));
#18786=CARTESIAN_POINT('Ctrl Pts',(2.12592706069774,2.42209655799667,26.9830495959493));
#18787=CARTESIAN_POINT('Ctrl Pts',(2.12607954760934,2.42196270840443,26.9830371204282));
#18788=CARTESIAN_POINT('Ctrl Pts',(2.12637159164145,2.42170630986765,26.983013224081));
#18789=CARTESIAN_POINT('Ctrl Pts',(2.12651115245028,2.42158376181839,26.9830018032192));
#18790=CARTESIAN_POINT('Ctrl Pts',(2.12677863139575,2.42134884816812,26.9829799116317));
#18791=CARTESIAN_POINT('Ctrl Pts',(2.12690654581621,2.42123648924487,26.9829694414299));
#18792=CARTESIAN_POINT('Ctrl Pts',(2.12715185014933,2.42102098159565,26.9829493602763));
#18793=CARTESIAN_POINT('Ctrl Pts',(2.12726924146242,2.42091783446856,26.9829397493917));
#18794=CARTESIAN_POINT('Ctrl Pts',(2.12749449537281,2.42071988368759,26.982921305876));
#18795=CARTESIAN_POINT('Ctrl Pts',(2.12760235914042,2.42062508135858,26.9829124733004));
#18796=CARTESIAN_POINT('Ctrl Pts',(2.12780944186967,2.42044305015498,26.9828955144633));
#18797=CARTESIAN_POINT('Ctrl Pts',(2.12790866180641,2.42035582238697,26.9828873882482));
#18798=CARTESIAN_POINT('Ctrl Pts',(2.128099243805,2.42018825421044,26.9828717780495));
#18799=CARTESIAN_POINT('Ctrl Pts',(2.12819060667789,2.42010791473224,26.9828642941053));
#18800=CARTESIAN_POINT('Ctrl Pts',(2.12836617707482,2.41995351016512,26.9828499112095));
#18801=CARTESIAN_POINT('Ctrl Pts',(2.12845038529192,2.41987944584585,26.9828430122899));
#18802=CARTESIAN_POINT('Ctrl Pts',(2.12861227528996,2.41973704246755,26.9828297481773));
#18803=CARTESIAN_POINT('Ctrl Pts',(2.12868995764406,2.41966870406467,26.9828233830119));
#18804=CARTESIAN_POINT('Ctrl Pts',(2.1288393602953,2.41953725941216,26.9828111403813));
#18805=CARTESIAN_POINT('Ctrl Pts',(2.12891108108067,2.41947415371153,26.9828052629389));
#18806=CARTESIAN_POINT('Ctrl Pts',(2.12904906831265,2.41935273058916,26.9827939543311));
#18807=CARTESIAN_POINT('Ctrl Pts',(2.12911533516649,2.41929441363614,26.9827885231854));
#18808=CARTESIAN_POINT('Ctrl Pts',(2.12924287225998,2.41918216761212,26.9827780698118));
#18809=CARTESIAN_POINT('Ctrl Pts',(2.12930414285475,2.41912823892906,26.9827730475998));
#18810=CARTESIAN_POINT('Ctrl Pts',(2.12945437320062,2.41899600020402,26.9827607329064));
#18811=CARTESIAN_POINT('Ctrl Pts',(2.12954333065476,2.41891768760537,26.9827534403187));
#18812=CARTESIAN_POINT('Ctrl Pts',(2.12971974953185,2.41876236214608,26.9827389766738));
#18813=CARTESIAN_POINT('Ctrl Pts',(2.12980721111147,2.41868534943636,26.9827318056223));
#18814=CARTESIAN_POINT('Ctrl Pts',(2.12998068616536,2.4185325824143,26.9827175811755));
#18815=CARTESIAN_POINT('Ctrl Pts',(2.13006669977602,2.41845682825688,26.9827105277867));
#18816=CARTESIAN_POINT('Ctrl Pts',(2.13023732496138,2.41830653858357,26.98269653494));
#18817=CARTESIAN_POINT('Ctrl Pts',(2.13032193666402,2.41823200321696,26.9826895954886));
#18818=CARTESIAN_POINT('Ctrl Pts',(2.13048980233284,2.41808411288109,26.9826758269335));
#18819=CARTESIAN_POINT('Ctrl Pts',(2.13057305642712,2.41801075804864,26.9826689978354));
#18820=CARTESIAN_POINT('Ctrl Pts',(2.13073824948652,2.41786519198312,26.9826554465398));
#18821=CARTESIAN_POINT('Ctrl Pts',(2.13082018858066,2.41779298087441,26.9826487243471));
#18822=CARTESIAN_POINT('Ctrl Pts',(2.13975179572824,2.40992094663764,26.9819159332282));
#18823=CARTESIAN_POINT('Ctrl Pts',(2.14855847974299,2.40207268198773,26.9811878322361));
#18824=CARTESIAN_POINT('Ctrl Pts',(2.17337713017793,2.37970932694403,26.979119976195));
#18825=CARTESIAN_POINT('Ctrl Pts',(2.18928622110668,2.36508148613681,26.9777754502592));
#18826=CARTESIAN_POINT('Ctrl Pts',(2.22478825923671,2.33177347566321,26.9747313544002));
#18827=CARTESIAN_POINT('Ctrl Pts',(2.24429519063882,2.31300440239998,26.9730280092599));
#18828=CARTESIAN_POINT('Ctrl Pts',(2.3052369928669,2.25287098159566,26.9676072573075));
#18829=CARTESIAN_POINT('Ctrl Pts',(2.3457805017552,2.21062398217785,26.9638519641924));
#18830=CARTESIAN_POINT('Ctrl Pts',(2.46840265004866,2.07567620416749,26.9520167012964));
#18831=CARTESIAN_POINT('Ctrl Pts',(2.54630033850352,1.97934151531673,26.9437873128926));
#18832=CARTESIAN_POINT('Ctrl Pts',(2.76658110839767,1.67233484702046,26.9183583337546));
#18833=CARTESIAN_POINT('Ctrl Pts',(2.88977645563576,1.44909647270064,26.9008597999752));
#18834=CARTESIAN_POINT('Ctrl Pts',(2.99337899916188,1.19425302280171,26.8833020401578));
#18835=CARTESIAN_POINT('Ctrl Pts',(3.00109375128844,1.17473165681126,26.8819720718141));
#18836=CARTESIAN_POINT('Ctrl Pts',(3.01166073617319,1.14720933649259,26.8801193649455));
#18837=CARTESIAN_POINT('Ctrl Pts',(3.01467271529979,1.13927085236154,26.8795875686246));
#18838=CARTESIAN_POINT('Ctrl Pts',(3.01948888966352,1.12642432018076,26.8787312784983));
#18839=CARTESIAN_POINT('Ctrl Pts',(3.02131254998701,1.12152368682939,26.8784056315513));
#18840=CARTESIAN_POINT('Ctrl Pts',(3.02512747309933,1.11119519438116,26.8777214540606));
#18841=CARTESIAN_POINT('Ctrl Pts',(3.02711606903218,1.10576638306868,26.8773630901564));
#18842=CARTESIAN_POINT('Ctrl Pts',(3.03194575885721,1.09247079357676,26.8764884173594));
#18843=CARTESIAN_POINT('Ctrl Pts',(3.03477088212172,1.08459818189439,26.8759730580219));
#18844=CARTESIAN_POINT('Ctrl Pts',(3.0448363611382,1.0562020297449,26.8741230624216));
#18845=CARTESIAN_POINT('Ctrl Pts',(3.05189962312081,1.03561573164215,26.8727985457858));
#18846=CARTESIAN_POINT('Ctrl Pts',(3.09470752271064,0.906606719356821,26.864592628539));
#18847=CARTESIAN_POINT('Ctrl Pts',(3.12488229447489,0.796408584558225,26.8579968505618));
#18848=CARTESIAN_POINT('Ctrl Pts',(3.19792077192141,0.46054610066478,26.8384941356114));
#18849=CARTESIAN_POINT('Ctrl Pts',(3.22259336429628,0.23170490280408,26.8259554958184));
#18850=CARTESIAN_POINT('Ctrl Pts',(3.22274925660414,0.00218896264416769,
26.8128035160936));
#18851=CARTESIAN_POINT('Ctrl Pts',(3.22274925938025,0.00218487163455499,
26.812803281666));
#18852=CARTESIAN_POINT('Ctrl Pts',(3.22282586991472,-0.11081789673651,26.8063278673062));
#18853=CARTESIAN_POINT('Ctrl Pts',(3.21695904115532,-0.22373863276078,26.7997274087064));
#18854=CARTESIAN_POINT('Ctrl Pts',(3.2032990818962,-0.35400002154735,26.791857615261));
#18855=CARTESIAN_POINT('Ctrl Pts',(3.20127368655899,-0.371870659126245,
26.7907724378864));
#18856=CARTESIAN_POINT('Ctrl Pts',(3.19766221446762,-0.40151595118787,26.7889626733654));
#18857=CARTESIAN_POINT('Ctrl Pts',(3.19616039951728,-0.413300606782162,
26.7882407322455));
#18858=CARTESIAN_POINT('Ctrl Pts',(3.19333552719224,-0.43453047307473,26.7869355052361));
#18859=CARTESIAN_POINT('Ctrl Pts',(3.19203562979979,-0.443978666451927,
26.7863529560028));
#18860=CARTESIAN_POINT('Ctrl Pts',(3.18929325563838,-0.46327657895039,26.785159628212));
#18861=CARTESIAN_POINT('Ctrl Pts',(3.18784704306445,-0.473125655139622,
26.7845487372277));
#18862=CARTESIAN_POINT('Ctrl Pts',(3.18462666541318,-0.494371931787416,
26.7832268636517));
#18863=CARTESIAN_POINT('Ctrl Pts',(3.18283690298084,-0.505766594860303,
26.7825153925917));
#18864=CARTESIAN_POINT('Ctrl Pts',(3.17781813311832,-0.536636936309397,
26.780580889161));
#18865=CARTESIAN_POINT('Ctrl Pts',(3.17447132019761,-0.556092706161243,
26.7793541227819));
#18866=CARTESIAN_POINT('Ctrl Pts',(3.15728261115944,-0.650798072895399,
26.773344753271));
#18867=CARTESIAN_POINT('Ctrl Pts',(3.14094366649954,-0.725563850861264,
26.768483090343));
#18868=CARTESIAN_POINT('Ctrl Pts',(3.10621929689288,-0.861129482699843,
26.7594448787204));
#18869=CARTESIAN_POINT('Ctrl Pts',(3.08866707250532,-0.922104778427121,
26.7552952450145));
#18870=CARTESIAN_POINT('Ctrl Pts',(2.99631415848239,-1.21060935231673,26.7352726325752));
#18871=CARTESIAN_POINT('Ctrl Pts',(2.89811279011069,-1.42982528152186,26.7188151032878));
#18872=CARTESIAN_POINT('Ctrl Pts',(2.7306887777384,-1.71394708060185,26.6968304959542));
#18873=CARTESIAN_POINT('Ctrl Pts',(2.68157778680158,-1.78980989015985,26.6908982231299));
#18874=CARTESIAN_POINT('Ctrl Pts',(2.61819748508275,-1.87923676115799,26.6839168555513));
#18875=CARTESIAN_POINT('Ctrl Pts',(2.60691404549134,-1.89485832646647,26.6826978005048));
#18876=CARTESIAN_POINT('Ctrl Pts',(2.5907684981817,-1.91679409845154,26.6809877894722));
#18877=CARTESIAN_POINT('Ctrl Pts',(2.58602231376956,-1.9231925600227,26.6804892123659));
#18878=CARTESIAN_POINT('Ctrl Pts',(2.57783629803442,-1.93414325632453,26.6796363874198));
#18879=CARTESIAN_POINT('Ctrl Pts',(2.57440803011895,-1.9387040547454,26.6792813401163));
#18880=CARTESIAN_POINT('Ctrl Pts',(2.56776165081248,-1.9474973519895,26.6785971106331));
#18881=CARTESIAN_POINT('Ctrl Pts',(2.56454517435413,-1.9517309960804,26.6782678139882));
#18882=CARTESIAN_POINT('Ctrl Pts',(2.55588564643758,-1.96307061650966,26.6773861110432));
#18883=CARTESIAN_POINT('Ctrl Pts',(2.55042339512233,-1.97016197130031,26.6768350490692));
#18884=CARTESIAN_POINT('Ctrl Pts',(2.53030613709133,-1.99605528196499,26.6748237055083));
#18885=CARTESIAN_POINT('Ctrl Pts',(2.5154717655646,-2.01471777424034,26.6733755904247));
#18886=CARTESIAN_POINT('Ctrl Pts',(2.35613980287337,-2.21066296036537,26.6581671547071));
#18887=CARTESIAN_POINT('Ctrl Pts',(2.19334680755055,-2.37227449380517,26.6455566901088));
#18888=CARTESIAN_POINT('Ctrl Pts',(1.89336608041769,-2.61256316101187,26.6240649359234));
#18889=CARTESIAN_POINT('Ctrl Pts',(1.76506558768164,-2.70089973017839,26.6153158363823));
#18890=CARTESIAN_POINT('Ctrl Pts',(1.58558389696391,-2.80620764940771,26.6031906303567));
#18891=CARTESIAN_POINT('Ctrl Pts',(1.53962963072683,-2.83168109577019,26.6000967564946));
#18892=CARTESIAN_POINT('Ctrl Pts',(1.47087546430418,-2.86762452903817,26.5954707591397));
#18893=CARTESIAN_POINT('Ctrl Pts',(1.44854183317959,-2.87897057573071,26.593968553581));
#18894=CARTESIAN_POINT('Ctrl Pts',(1.40782601998691,-2.89906152721095,26.591229433639));
#18895=CARTESIAN_POINT('Ctrl Pts',(1.38948879685016,-2.90789489066779,26.5899956376444));
#18896=CARTESIAN_POINT('Ctrl Pts',(1.36067314126448,-2.92144110569147,26.5880560130512));
#18897=CARTESIAN_POINT('Ctrl Pts',(1.35025088353301,-2.92627272780803,26.5873543139805));
#18898=CARTESIAN_POINT('Ctrl Pts',(1.33973635302105,-2.93107899454848,26.5866461870607));
#18899=CARTESIAN_POINT('Ctrl Pts',(1.33966958388279,-2.93110951243872,26.5866416903202));
#18900=CARTESIAN_POINT('Ctrl Pts',(1.33953387203146,-2.93117153608009,26.5866325504364));
#18901=CARTESIAN_POINT('Ctrl Pts',(1.33946492923982,-2.93120304168481,26.5866279072872));
#18902=CARTESIAN_POINT('Ctrl Pts',(1.33932479338795,-2.93126707524969,26.5866184694192));
#18903=CARTESIAN_POINT('Ctrl Pts',(1.33925360024441,-2.93129960305304,26.5866136746942));
#18904=CARTESIAN_POINT('Ctrl Pts',(1.33910888402373,-2.93136571682251,26.5866039283072));
#18905=CARTESIAN_POINT('Ctrl Pts',(1.33903536085931,-2.93139930262017,26.5865989766387));
#18906=CARTESIAN_POINT('Ctrl Pts',(1.33888589550201,-2.9314675724449,26.5865889103625));
#18907=CARTESIAN_POINT('Ctrl Pts',(1.33880995323971,-2.93150225627913,26.586583795749));
#18908=CARTESIAN_POINT('Ctrl Pts',(1.33865559563525,-2.93157274619029,26.586573399941));
#18909=CARTESIAN_POINT('Ctrl Pts',(1.3385771614073,-2.93160856065243,26.5865681174734));
#18910=CARTESIAN_POINT('Ctrl Pts',(1.3384177031863,-2.9316813643756,26.5865573780954));
#18911=CARTESIAN_POINT('Ctrl Pts',(1.33833668076369,-2.93171835266499,26.58655192129));
#18912=CARTESIAN_POINT('Ctrl Pts',(1.33817195333232,-2.93179354564366,26.5865408269824));
#18913=CARTESIAN_POINT('Ctrl Pts',(1.33808824982571,-2.93183174937478,26.5865351895806));
#18914=CARTESIAN_POINT('Ctrl Pts',(1.33791806393331,-2.93190941635902,26.5865237275923));
#18915=CARTESIAN_POINT('Ctrl Pts',(1.33783158288042,-2.93194887871225,26.5865179030946));
#18916=CARTESIAN_POINT('Ctrl Pts',(1.337655741717,-2.93202910776756,26.5865060601647));
#18917=CARTESIAN_POINT('Ctrl Pts',(1.33756638284808,-2.93206987359099,26.586500041815));
#18918=CARTESIAN_POINT('Ctrl Pts',(1.33738468195895,-2.9321527561265,26.5864878041672));
#18919=CARTESIAN_POINT('Ctrl Pts',(1.33729234107312,-2.93219487198691,26.5864815849445));
#18920=CARTESIAN_POINT('Ctrl Pts',(1.3371045680401,-2.93228050288938,26.5864689382659));
#18921=CARTESIAN_POINT('Ctrl Pts',(1.33700913688059,-2.93232401712314,26.5864625108754));
#18922=CARTESIAN_POINT('Ctrl Pts',(1.33681507096482,-2.93241249490759,26.5864494402919));
#18923=CARTESIAN_POINT('Ctrl Pts',(1.33671643706481,-2.9324574576846,26.5864427971554));
#18924=CARTESIAN_POINT('Ctrl Pts',(1.33651584883393,-2.93254888465101,26.5864292872069));
#18925=CARTESIAN_POINT('Ctrl Pts',(1.33641389529651,-2.93259534806815,26.5864224204471));
#18926=CARTESIAN_POINT('Ctrl Pts',(1.33620654650832,-2.93268983034023,26.5864084550794));
#18927=CARTESIAN_POINT('Ctrl Pts',(1.33610115192091,-2.93273784845299,26.5864013565149));
#18928=CARTESIAN_POINT('Ctrl Pts',(1.33588679290125,-2.93283549715756,26.5863869189032));
#18929=CARTESIAN_POINT('Ctrl Pts',(1.33577782901695,-2.93288512702751,26.5863795798915));
#18930=CARTESIAN_POINT('Ctrl Pts',(1.33557523126474,-2.93297739076114,26.5863659343418));
#18931=CARTESIAN_POINT('Ctrl Pts',(1.33548159238519,-2.93302002882444,26.5863596274726));
#18932=CARTESIAN_POINT('Ctrl Pts',(1.3352795757446,-2.93311200455708,26.5863460209864));
#18933=CARTESIAN_POINT('Ctrl Pts',(1.33517119968111,-2.93316133961647,26.586338721478));
#18934=CARTESIAN_POINT('Ctrl Pts',(1.33493737618472,-2.93326776533605,26.5863229725933));
#18935=CARTESIAN_POINT('Ctrl Pts',(1.33481192986262,-2.93332485302804,26.5863145232839));
#18936=CARTESIAN_POINT('Ctrl Pts',(1.33454126183888,-2.93344800676647,26.5862962926457));
#18937=CARTESIAN_POINT('Ctrl Pts',(1.33439604061519,-2.93351406929371,26.5862865113384));
#18938=CARTESIAN_POINT('Ctrl Pts',(1.33408268889166,-2.93365658791416,26.5862654055879));
#18939=CARTESIAN_POINT('Ctrl Pts',(1.33391455807964,-2.93373303972201,26.5862540811092));
#18940=CARTESIAN_POINT('Ctrl Pts',(1.33355175632577,-2.93389797392922,26.5862296444129));
#18941=CARTESIAN_POINT('Ctrl Pts',(1.33335708414848,-2.93398645095311,26.5862165320925));
#18942=CARTESIAN_POINT('Ctrl Pts',(1.33299563058492,-2.93415068544491,26.5861921859174));
#18943=CARTESIAN_POINT('Ctrl Pts',(1.33282885134609,-2.93422644815883,26.5861809522279));
#18944=CARTESIAN_POINT('Ctrl Pts',(1.32348033633171,-2.93847223148143,26.5855512644567));
#18945=CARTESIAN_POINT('Ctrl Pts',(1.31427916940426,-2.9425991091253,26.5849313286266));
#18946=CARTESIAN_POINT('Ctrl Pts',(1.29307332661465,-2.95199098331864,26.5835020988738));
#18947=CARTESIAN_POINT('Ctrl Pts',(1.28105565545905,-2.95722603009173,26.5826917882655));
#18948=CARTESIAN_POINT('Ctrl Pts',(1.24883077170862,-2.97103029672416,26.5805178922718));
#18949=CARTESIAN_POINT('Ctrl Pts',(1.22856767045543,-2.97946652289181,26.5791498048508));
#18950=CARTESIAN_POINT('Ctrl Pts',(1.05679288327298,-3.04893204777257,26.5675407676242));
#18951=CARTESIAN_POINT('Ctrl Pts',(0.900952952378805,-3.09855886776507,
26.5569151848866));
#18952=CARTESIAN_POINT('Ctrl Pts',(0.495527185882263,-3.19448636872886,
26.5291312511289));
#18953=CARTESIAN_POINT('Ctrl Pts',(0.243006374883721,-3.22354358082419,
26.5116470754176));
#18954=CARTESIAN_POINT('Ctrl Pts',(-0.0676383208765035,-3.22255018002376,
26.4913132309825));
#18955=CARTESIAN_POINT('Ctrl Pts',(-0.124959999337608,-3.22083693580544,
26.4876143413083));
#18956=CARTESIAN_POINT('Ctrl Pts',(-0.193924656320438,-3.21693153131852,
26.4832519524339));
#18957=CARTESIAN_POINT('Ctrl Pts',(-0.205636401191146,-3.21620411821422,
26.4825141822825));
#18958=CARTESIAN_POINT('Ctrl Pts',(-0.223849264150498,-3.21497302938225,
26.4813719175965));
#18959=CARTESIAN_POINT('Ctrl Pts',(-0.230353125159929,-3.21451357319154,
26.4809650119228));
#18960=CARTESIAN_POINT('Ctrl Pts',(-0.242422233832086,-3.21362415017293,
26.4802118366673));
#18961=CARTESIAN_POINT('Ctrl Pts',(-0.247987706845663,-3.21319946720083,
26.4798652840179));
#18962=CARTESIAN_POINT('Ctrl Pts',(-0.26058906060733,-3.21220496388882,
26.4790823223573));
#18963=CARTESIAN_POINT('Ctrl Pts',(-0.267624172065996,-3.2116264872033,
26.4786464053393));
#18964=CARTESIAN_POINT('Ctrl Pts',(-0.288453704431659,-3.20984481764432,
26.4773591384643));
#18965=CARTESIAN_POINT('Ctrl Pts',(-0.302242542533823,-3.20857581403445,
26.4765113987285));
#18966=CARTESIAN_POINT('Ctrl Pts',(-0.405173996976067,-3.19843346836605,
26.4702132736777));
#18967=CARTESIAN_POINT('Ctrl Pts',(-0.49392894998173,-3.18593471000097,
26.4649510967362));
#18968=CARTESIAN_POINT('Ctrl Pts',(-0.823926422260698,-3.12533787396944,
26.4456384830663));
#18969=CARTESIAN_POINT('Ctrl Pts',(-1.0599270876327,-3.05338505479416,26.4322794705481));
#18970=CARTESIAN_POINT('Ctrl Pts',(-1.34969414152482,-2.92734523078933,
26.414286725607));
#18971=CARTESIAN_POINT('Ctrl Pts',(-1.41299276552639,-2.89732175120204,
26.4102562562727));
#18972=CARTESIAN_POINT('Ctrl Pts',(-1.47525541363878,-2.86526421591962,
26.4061645232028));
#18973=CARTESIAN_POINT('',(3.21940908233495,-0.00238856237501944,26.5642265507269));
#18974=CARTESIAN_POINT('Ctrl Pts',(-1.47525540475399,-2.86526422049419,
26.1560859507638));
#18975=CARTESIAN_POINT('Ctrl Pts',(-1.46764044335333,-2.86918498036092,
26.156568770356));
#18976=CARTESIAN_POINT('Ctrl Pts',(-1.46000897820681,-2.87307583278742,
26.1570521035361));
#18977=CARTESIAN_POINT('Ctrl Pts',(-1.30595814504514,-2.95084516714172,
26.16679927672));
#18978=CARTESIAN_POINT('Ctrl Pts',(-1.15414623481615,-3.01346144532023,
26.1762494445484));
#18979=CARTESIAN_POINT('Ctrl Pts',(-0.977417527058379,-3.07103438507643,
26.1874290175851));
#18980=CARTESIAN_POINT('Ctrl Pts',(-0.956525440761596,-3.07760560524402,
26.1887530375465));
#18981=CARTESIAN_POINT('Ctrl Pts',(-0.92304008146664,-3.08776391163117,
26.1908797013164));
#18982=CARTESIAN_POINT('Ctrl Pts',(-0.910488879267811,-3.09148814630701,
26.1916778456073));
#18983=CARTESIAN_POINT('Ctrl Pts',(-0.888235651919161,-3.09794392686131,
26.1930948876133));
#18984=CARTESIAN_POINT('Ctrl Pts',(-0.878542795701445,-3.10070664522986,
26.1937127566156));
#18985=CARTESIAN_POINT('Ctrl Pts',(-0.858390510585305,-3.10634849645055,
26.1949987701897));
#18986=CARTESIAN_POINT('Ctrl Pts',(-0.847929198296684,-3.10922037175426,
26.1956671425741));
#18987=CARTESIAN_POINT('Ctrl Pts',(-0.820870895580562,-3.11650179491454,
26.1973980193688));
#18988=CARTESIAN_POINT('Ctrl Pts',(-0.804252966834529,-3.12083155775106,
26.1984631012167));
#18989=CARTESIAN_POINT('Ctrl Pts',(-0.733203124191961,-3.1387382636165,
26.2030261550677));
#18990=CARTESIAN_POINT('Ctrl Pts',(-0.678459038817052,-3.15102481793287,
26.2065654631099));
#18991=CARTESIAN_POINT('Ctrl Pts',(-0.533223099603586,-3.179660885973,26.2160228537045));
#18992=CARTESIAN_POINT('Ctrl Pts',(-0.442309085280903,-3.19357642378303,
26.2220125964033));
#18993=CARTESIAN_POINT('Ctrl Pts',(-0.109722320735569,-3.23000903986616,
26.2441460620574));
#18994=CARTESIAN_POINT('Ctrl Pts',(0.133673291029568,-3.22910419147909,
26.2608353902054));
#18995=CARTESIAN_POINT('Ctrl Pts',(0.466180526924267,-3.190185896532,26.2831093112432));
#18996=CARTESIAN_POINT('Ctrl Pts',(0.557220002835747,-3.17555028862907,
26.2891421071121));
#18997=CARTESIAN_POINT('Ctrl Pts',(0.661163076989448,-3.15423129277377,
26.2958630832165));
#18998=CARTESIAN_POINT('Ctrl Pts',(0.674792952130234,-3.15134354695577,
26.2967410323165));
#18999=CARTESIAN_POINT('Ctrl Pts',(0.695316189556948,-3.1468560536317,26.2980574909063));
#19000=CARTESIAN_POINT('Ctrl Pts',(0.702223503362877,-3.14532188803192,
26.2984996140915));
#19001=CARTESIAN_POINT('Ctrl Pts',(0.714570140462353,-3.14253690924731,
26.2992881364272));
#19002=CARTESIAN_POINT('Ctrl Pts',(0.720011299888353,-3.14129470779614,
26.2996350209954));
#19003=CARTESIAN_POINT('Ctrl Pts',(0.731785834247685,-3.13857441358129,
26.3003843244804));
#19004=CARTESIAN_POINT('Ctrl Pts',(0.738117951353907,-3.13709128787278,
26.300786449512));
#19005=CARTESIAN_POINT('Ctrl Pts',(0.755794412267653,-3.13289457598759,
26.3019067779972));
#19006=CARTESIAN_POINT('Ctrl Pts',(0.767128713543755,-3.13013852160256,
26.3026225772049));
#19007=CARTESIAN_POINT('Ctrl Pts',(0.832997717855822,-3.11374250859242,
26.3067688093427));
#19008=CARTESIAN_POINT('Ctrl Pts',(0.887186716091496,-3.0987381671683,26.3101254391457));
#19009=CARTESIAN_POINT('Ctrl Pts',(1.18390322436164,-3.0081577439854,26.3283431138471));
#19010=CARTESIAN_POINT('Ctrl Pts',(1.41724969787939,-2.90552411867305,26.3421277450282));
#19011=CARTESIAN_POINT('Ctrl Pts',(1.7773175230257,-2.69334597295007,26.365734231375));
#19012=CARTESIAN_POINT('Ctrl Pts',(1.91192769710494,-2.59951767631807,26.3751767648808));
#19013=CARTESIAN_POINT('Ctrl Pts',(2.0558054133444,-2.4819877530351,26.3863504920979));
#19014=CARTESIAN_POINT('Ctrl Pts',(2.07265749311309,-2.467932329606,26.387677078521));
#19015=CARTESIAN_POINT('Ctrl Pts',(2.09934191257006,-2.44521018093835,26.3898070858959));
#19016=CARTESIAN_POINT('Ctrl Pts',(2.10926738659486,-2.43665352045053,26.3906059846795));
#19017=CARTESIAN_POINT('Ctrl Pts',(2.12673528682884,-2.42140789765445,26.3920239000555));
#19018=CARTESIAN_POINT('Ctrl Pts',(2.13429907633432,-2.41474359635906,26.3926418837084));
#19019=CARTESIAN_POINT('Ctrl Pts',(2.14879599602678,-2.40184933105798,26.3938341396676));
#19020=CARTESIAN_POINT('Ctrl Pts',(2.15573361964947,-2.39562455318779,26.3944081899572));
#19021=CARTESIAN_POINT('Ctrl Pts',(2.17384979557704,-2.37922740930883,26.395916440901));
#19022=CARTESIAN_POINT('Ctrl Pts',(2.18498386242145,-2.36900643886014,26.3968527025562));
#19023=CARTESIAN_POINT('Ctrl Pts',(2.22647069933631,-2.33038063473043,26.4003767636376));
#19024=CARTESIAN_POINT('Ctrl Pts',(2.25634377315805,-2.30146870369513,26.4029863306109));
#19025=CARTESIAN_POINT('Ctrl Pts',(2.32914064679154,-2.22823414681796,26.4095306633531));
#19026=CARTESIAN_POINT('Ctrl Pts',(2.37136526263424,-2.18324289586147,26.4134941670493));
#19027=CARTESIAN_POINT('Ctrl Pts',(2.49236435097461,-2.04666217932373,26.425362428195));
#19028=CARTESIAN_POINT('Ctrl Pts',(2.56730534970951,-1.9518311241881,26.4334000256452));
#19029=CARTESIAN_POINT('Ctrl Pts',(2.7813350911386,-1.6472799421725,26.4584603722913));
#19030=CARTESIAN_POINT('Ctrl Pts',(2.90135541885982,-1.42530937226928,26.4757693486689));
#19031=CARTESIAN_POINT('Ctrl Pts',(3.00219262680771,-1.17192445927172,26.4931785280334));
#19032=CARTESIAN_POINT('Ctrl Pts',(3.00984133775829,-1.15213830956013,26.4945227961182));
#19033=CARTESIAN_POINT('Ctrl Pts',(3.02028996461847,-1.12429479626733,26.4963918564774));
#19034=CARTESIAN_POINT('Ctrl Pts',(3.02325391467622,-1.11630015255855,26.4969259179949));
#19035=CARTESIAN_POINT('Ctrl Pts',(3.02798618761696,-1.10337872355117,26.4977848054628));
#19036=CARTESIAN_POINT('Ctrl Pts',(3.02977427220268,-1.09845929392863,26.4981107984835));
#19037=CARTESIAN_POINT('Ctrl Pts',(3.03350889949543,-1.08810598495214,26.4987947381134));
#19038=CARTESIAN_POINT('Ctrl Pts',(3.03545284031187,-1.08267120253822,26.4991525221424));
#19039=CARTESIAN_POINT('Ctrl Pts',(3.04016430873015,-1.06938665385681,26.5000241203941));
#19040=CARTESIAN_POINT('Ctrl Pts',(3.04291607167315,-1.06153126373979,26.5005369997594));
#19041=CARTESIAN_POINT('Ctrl Pts',(3.05266950472866,-1.03333879748522,26.5023689950491));
#19042=CARTESIAN_POINT('Ctrl Pts',(3.05949815986373,-1.0129418753169,26.5036782465789));
#19043=CARTESIAN_POINT('Ctrl Pts',(3.11626315913772,-0.837574239613999,
26.5148089846184));
#19044=CARTESIAN_POINT('Ctrl Pts',(3.15460002089174,-0.679072388780371,
26.5240365978845));
#19045=CARTESIAN_POINT('Ctrl Pts',(3.20859782668131,-0.347710788668034,
26.5428622399681));
#19046=CARTESIAN_POINT('Ctrl Pts',(3.2226268427006,-0.175138493841783,26.552424709566));
#19047=CARTESIAN_POINT('Ctrl Pts',(3.22274919271196,-0.0022810906157154,
26.5623024648959));
#19048=CARTESIAN_POINT('Ctrl Pts',(3.21940908233495,-0.00238856237501944,
26.5642265507269));
#19049=CARTESIAN_POINT('Ctrl Pts',(3.21459332503562,0.701948265465156,26.607604666478));
#19050=CARTESIAN_POINT('Ctrl Pts',(2.63997125700238,2.4901339051279,26.7172937616837));
#19051=CARTESIAN_POINT('Ctrl Pts',(-0.317098310746752,3.79898125969958,
26.8932938363438));
#19052=CARTESIAN_POINT('Ctrl Pts',(-3.36796503595531,1.78595113785612,27.0922267747072));
#19053=CARTESIAN_POINT('Ctrl Pts',(-3.32895242825944,-1.36033153994631,
27.2634778562151));
#19054=CARTESIAN_POINT('Ctrl Pts',(-2.03006326125809,-2.57117805515723,
27.3684179582684));
#19055=CARTESIAN_POINT('Ctrl Pts',(-1.47306432504222,-2.86105893806616,
27.4070470808673));
#19056=CARTESIAN_POINT('Origin',(0.,0.,4.68922655072688));
#19057=CARTESIAN_POINT('',(-1.4752555406476,-2.86526415052584,28.9026236394039));
#19058=CARTESIAN_POINT('',(-1.47525540425972,-2.86526422074867,28.6587956971472));
#19059=CARTESIAN_POINT('',(-1.47525540501186,-2.86526422036142,4.68922655072688));
#19060=CARTESIAN_POINT('Ctrl Pts',(-1.4752555406476,-2.86526415052584,28.9026236394039));
#19061=CARTESIAN_POINT('Ctrl Pts',(-1.56730140613998,-2.81787195004184,
28.8956334603849));
#19062=CARTESIAN_POINT('Ctrl Pts',(-1.6570868159356,-2.76603248162266,28.8886853090942));
#19063=CARTESIAN_POINT('Ctrl Pts',(-1.79111221064324,-2.6797640429632,28.8782617696498));
#19064=CARTESIAN_POINT('Ctrl Pts',(-1.83714954367225,-2.64841475594034,
28.8746717941389));
#19065=CARTESIAN_POINT('Ctrl Pts',(-1.89179829599422,-2.60909028932208,
28.8704203841509));
#19066=CARTESIAN_POINT('Ctrl Pts',(-1.90120547345437,-2.6022433952295,28.8696889263588));
#19067=CARTESIAN_POINT('Ctrl Pts',(-1.91580878973593,-2.59149309709788,
28.8685542953062));
#19068=CARTESIAN_POINT('Ctrl Pts',(-1.92103043799582,-2.58762475046121,
28.8681487615474));
#19069=CARTESIAN_POINT('Ctrl Pts',(-1.93071717602593,-2.58040305560169,
28.8673968270738));
#19070=CARTESIAN_POINT('Ctrl Pts',(-1.93518520739461,-2.57705392977,28.8670501514661));
#19071=CARTESIAN_POINT('Ctrl Pts',(-1.94530536430558,-2.56942694902911,
28.8662652570443));
#19072=CARTESIAN_POINT('Ctrl Pts',(-1.95095208179233,-2.56514205914806,
28.8658275405044));
#19073=CARTESIAN_POINT('Ctrl Pts',(-1.96769755226864,-2.5523478393405,28.8645300118211));
#19074=CARTESIAN_POINT('Ctrl Pts',(-1.97875527216978,-2.54378472742606,
28.8636738958671));
#19075=CARTESIAN_POINT('Ctrl Pts',(-2.06345495108211,-2.47730668540049,
28.8571185829835));
#19076=CARTESIAN_POINT('Ctrl Pts',(-2.13460316244975,-2.41627143657345,
28.8516254193862));
#19077=CARTESIAN_POINT('Ctrl Pts',(-2.37871511001782,-2.18764541868971,
28.8324119683121));
#19078=CARTESIAN_POINT('Ctrl Pts',(-2.53544491927282,-2.00389856810038,
28.8193174483597));
#19079=CARTESIAN_POINT('Ctrl Pts',(-2.72181609712744,-1.72809599534153,
28.8003685331252));
#19080=CARTESIAN_POINT('Ctrl Pts',(-2.7700805469508,-1.64962130828407,28.7950533843081));
#19081=CARTESIAN_POINT('Ctrl Pts',(-2.84226670632227,-1.52012918119093,
28.7863117256357));
#19082=CARTESIAN_POINT('Ctrl Pts',(-2.86832828819597,-1.47036220366954,
28.7829590202086));
#19083=CARTESIAN_POINT('Ctrl Pts',(-2.90064640220615,-1.40451533067834,
28.7785204167684));
#19084=CARTESIAN_POINT('Ctrl Pts',(-2.90809419787725,-1.38902879135833,
28.777476336685));
#19085=CARTESIAN_POINT('Ctrl Pts',(-2.92004322761825,-1.36366524788142,
28.7757657781034));
#19086=CARTESIAN_POINT('Ctrl Pts',(-2.92461910900727,-1.35382363035624,
28.7751019014415));
#19087=CARTESIAN_POINT('Ctrl Pts',(-2.93334958183195,-1.33479565505211,
28.7738179921341));
#19088=CARTESIAN_POINT('Ctrl Pts',(-2.937510955514,-1.32561253484125,28.7731982033091));
#19089=CARTESIAN_POINT('Ctrl Pts',(-2.9469776713719,-1.30445836206339,28.7717700239772));
#19090=CARTESIAN_POINT('Ctrl Pts',(-2.95225325622351,-1.29247426160268,
28.7709606216537));
#19091=CARTESIAN_POINT('Ctrl Pts',(-2.96615660276967,-1.26036191230788,
28.7687907457362));
#19092=CARTESIAN_POINT('Ctrl Pts',(-2.97465235863254,-1.24017758776531,
28.7674257962138));
#19093=CARTESIAN_POINT('Ctrl Pts',(-3.04479537790896,-1.06866267115801,
28.7558163348866));
#19094=CARTESIAN_POINT('Ctrl Pts',(-3.09504711095917,-0.912955425733579,
28.7451868192979));
#19095=CARTESIAN_POINT('Ctrl Pts',(-3.1925407174096,-0.50788733750899,28.7174020277814));
#19096=CARTESIAN_POINT('Ctrl Pts',(-3.22257121850819,-0.255529787699744,
28.6999213396051));
#19097=CARTESIAN_POINT('Ctrl Pts',(-3.22278954261968,0.0551348078913998,
28.6795855422955));
#19098=CARTESIAN_POINT('Ctrl Pts',(-3.2212963744716,0.112529628370398,28.6758822291109));
#19099=CARTESIAN_POINT('Ctrl Pts',(-3.21765197086125,0.181579560390752,
28.6715153401291));
#19100=CARTESIAN_POINT('Ctrl Pts',(-3.21696926498658,0.193297957757453,
28.6707773184156));
#19101=CARTESIAN_POINT('Ctrl Pts',(-3.21580771864204,0.211520213369535,
28.669634749598));
#19102=CARTESIAN_POINT('Ctrl Pts',(-3.2153731458202,0.21802664715179,28.6692277893272));
#19103=CARTESIAN_POINT('Ctrl Pts',(-3.21452994628046,0.230099851262853,
28.668474564397));
#19104=CARTESIAN_POINT('Ctrl Pts',(-3.21412660988983,0.235666827152145,
28.6681280163452));
#19105=CARTESIAN_POINT('Ctrl Pts',(-3.21318051955694,0.248270660596358,
28.6673451302571));
#19106=CARTESIAN_POINT('Ctrl Pts',(-3.2126291135446,0.255306782552613,28.6669092838105));
#19107=CARTESIAN_POINT('Ctrl Pts',(-3.2109278740279,0.276136434802271,28.6656224185816));
#19108=CARTESIAN_POINT('Ctrl Pts',(-3.20971227091084,0.289924639771291,
28.6647750065724));
#19109=CARTESIAN_POINT('Ctrl Pts',(-3.19998012148806,0.392737296411756,
28.6584864401568));
#19110=CARTESIAN_POINT('Ctrl Pts',(-3.18784924156409,0.481389369630846,
28.6532328483776));
#19111=CARTESIAN_POINT('Ctrl Pts',(-3.12855841077339,0.811672530400887,
28.6339160319763));
#19112=CARTESIAN_POINT('Ctrl Pts',(-3.05746574546789,1.04814477075452,28.6205467893947));
#19113=CARTESIAN_POINT('Ctrl Pts',(-2.92395360223317,1.35830442625515,28.6013191719088));
#19114=CARTESIAN_POINT('Ctrl Pts',(-2.88420043543491,1.44079197707685,28.596035050863));
#19115=CARTESIAN_POINT('Ctrl Pts',(-2.81459010734627,1.57077299908811,28.5873397767587));
#19116=CARTESIAN_POINT('Ctrl Pts',(-2.78690968122773,1.61937615903619,28.5840014068452));
#19117=CARTESIAN_POINT('Ctrl Pts',(-2.74910389112307,1.6819154957271,28.5795791462205));
#19118=CARTESIAN_POINT('Ctrl Pts',(-2.74011083716814,1.69652719438238,28.5785366833908));
#19119=CARTESIAN_POINT('Ctrl Pts',(-2.72524237199105,1.72025848188921,28.576828108941));
#19120=CARTESIAN_POINT('Ctrl Pts',(-2.71943675623714,1.72942156656025,28.5761645875254));
#19121=CARTESIAN_POINT('Ctrl Pts',(-2.70814500026648,1.74704605284769,28.5748808973243));
#19122=CARTESIAN_POINT('Ctrl Pts',(-2.70266518156472,1.75551136877768,28.5742609698417));
#19123=CARTESIAN_POINT('Ctrl Pts',(-2.68997140563666,1.77492062045923,28.5728317996216));
#19124=CARTESIAN_POINT('Ctrl Pts',(-2.68273026819452,1.78584648613132,28.5720215404742));
#19125=CARTESIAN_POINT('Ctrl Pts',(-2.66318747184001,1.81494674485511,28.5698478723153));
#19126=CARTESIAN_POINT('Ctrl Pts',(-2.6507666498961,1.83303991395204,28.5684799627496));
#19127=CARTESIAN_POINT('Ctrl Pts',(-2.54295203211013,1.9867037546689,28.556719018445));
#19128=CARTESIAN_POINT('Ctrl Pts',(-2.43742929097225,2.11483335468626,28.5459292616739));
#19129=CARTESIAN_POINT('Ctrl Pts',(-2.14305584948308,2.42083701885942,28.5175948048162));
#19130=CARTESIAN_POINT('Ctrl Pts',(-1.94175708752973,2.5850949708056,28.4997106673666));
#19131=CARTESIAN_POINT('Ctrl Pts',(-1.68057142571857,2.75033009865859,28.4795632837662));
#19132=CARTESIAN_POINT('Ctrl Pts',(-1.6375381045039,2.77616742812961,28.4763357359406));
#19133=CARTESIAN_POINT('Ctrl Pts',(-1.58411530609293,2.80656790781641,28.4724562387807));
#19134=CARTESIAN_POINT('Ctrl Pts',(-1.57428509144624,2.8120937366892,28.4717475595407));
#19135=CARTESIAN_POINT('Ctrl Pts',(-1.5588131888252,2.82068435302337,28.4706405081177));
#19136=CARTESIAN_POINT('Ctrl Pts',(-1.55319111532613,2.82378401051268,28.4702399543904));
#19137=CARTESIAN_POINT('Ctrl Pts',(-1.54265271608918,2.82955322543462,28.4694923950618));
#19138=CARTESIAN_POINT('Ctrl Pts',(-1.53773875762237,2.83222675150089,28.4691451445569));
#19139=CARTESIAN_POINT('Ctrl Pts',(-1.52648154739398,2.83831350147256,28.468352648757));
#19140=CARTESIAN_POINT('Ctrl Pts',(-1.52013380828977,2.8417182574009,28.4679079455588));
#19141=CARTESIAN_POINT('Ctrl Pts',(-1.50049836641492,2.85216555825527,28.4665388718724));
#19142=CARTESIAN_POINT('Ctrl Pts',(-1.48717251860614,2.85913651992215,28.4656189268024));
#19143=CARTESIAN_POINT('Ctrl Pts',(-1.34343909618597,2.93304894054213,28.4557895320587));
#19144=CARTESIAN_POINT('Ctrl Pts',(-1.20864005544456,2.99112108815557,28.4473884955365));
#19145=CARTESIAN_POINT('Ctrl Pts',(-0.900818392295055,3.09950702296103,
28.4289936604746));
#19146=CARTESIAN_POINT('Ctrl Pts',(-0.726604121829914,3.1449108959695,28.419089350069));
#19147=CARTESIAN_POINT('Ctrl Pts',(-0.419874762316938,3.19798873386393,
28.4014040101522));
#19148=CARTESIAN_POINT('Ctrl Pts',(-0.28899849413919,3.21246024709217,28.3937865778758));
#19149=CARTESIAN_POINT('Ctrl Pts',(-0.126422222750853,3.22042081285705,
28.384044698385));
#19150=CARTESIAN_POINT('Ctrl Pts',(-0.095211274930035,3.2214946064501,28.3821621965311));
#19151=CARTESIAN_POINT('Ctrl Pts',(-0.0502854838666851,3.22238682238048,
28.3794329076833));
#19152=CARTESIAN_POINT('Ctrl Pts',(-0.036579080523726,3.22257155462921,
28.378597613325));
#19153=CARTESIAN_POINT('Ctrl Pts',(-0.0127282929175396,3.22274082958144,
28.377139385869));
#19154=CARTESIAN_POINT('Ctrl Pts',(-0.00258431627414837,3.22276492808057,
28.3765177035535));
#19155=CARTESIAN_POINT('Ctrl Pts',(0.0169836838643136,3.22271902784754,
28.3753155339019));
#19156=CARTESIAN_POINT('Ctrl Pts',(0.0264076303351211,3.22265558383299,
28.3747352590598));
#19157=CARTESIAN_POINT('Ctrl Pts',(0.0487343638289391,3.22240733606204,
28.3733573387506));
#19158=CARTESIAN_POINT('Ctrl Pts',(0.0616365120751564,3.22218637113183,
28.372558564387));
#19159=CARTESIAN_POINT('Ctrl Pts',(0.107109419009939,3.22113437718066,28.3697343063039));
#19160=CARTESIAN_POINT('Ctrl Pts',(0.139667690023879,3.2198869411829,28.3676958127546));
#19161=CARTESIAN_POINT('Ctrl Pts',(0.465678489294179,3.20244235497597,28.3471136937416));
#19162=CARTESIAN_POINT('Ctrl Pts',(0.7555762000239,3.14666881789368,28.3272361943177));
#19163=CARTESIAN_POINT('Ctrl Pts',(1.0958761747199,3.03141307400087,28.302956158424));
#19164=CARTESIAN_POINT('Ctrl Pts',(1.15727564909789,3.00850850121993,28.2985442141292));
#19165=CARTESIAN_POINT('Ctrl Pts',(1.30100887108474,2.94983803926124,28.2881971643166));
#19166=CARTESIAN_POINT('Ctrl Pts',(1.38263763859029,2.91247055332315,28.2823054340372));
#19167=CARTESIAN_POINT('Ctrl Pts',(1.47971836405638,2.86302634781193,28.2753667317354));
#19168=CARTESIAN_POINT('Ctrl Pts',(1.496751822055,2.85415842771832,28.2741519597263));
#19169=CARTESIAN_POINT('Ctrl Pts',(1.52072866172942,2.8414019755943,28.2724468802679));
#19170=CARTESIAN_POINT('Ctrl Pts',(1.52773807629044,2.83763937507344,28.2719490097452));
#19171=CARTESIAN_POINT('Ctrl Pts',(1.53974883055604,2.83113468973272,28.2710970165854));
#19172=CARTESIAN_POINT('Ctrl Pts',(1.54475693186797,2.82840522486325,28.2707420984575));
#19173=CARTESIAN_POINT('Ctrl Pts',(1.55442210340478,2.82310428187572,28.2700578234322));
#19174=CARTESIAN_POINT('Ctrl Pts',(1.55908005719206,2.82053456602478,28.2697283534778));
#19175=CARTESIAN_POINT('Ctrl Pts',(1.57157123910579,2.81360299030571,28.2688455767616));
#19176=CARTESIAN_POINT('Ctrl Pts',(1.57939273289979,2.80921991777122,28.268293620265));
#19177=CARTESIAN_POINT('Ctrl Pts',(1.60802705950632,2.79301618882706,28.2662754953155));
#19178=CARTESIAN_POINT('Ctrl Pts',(1.62872691792977,2.78099607335252,28.2648216002393));
#19179=CARTESIAN_POINT('Ctrl Pts',(1.91319153093075,2.61154568013603,28.2448841753249));
#19180=CARTESIAN_POINT('Ctrl Pts',(2.15330288411082,2.41740014490797,28.2284434616139));
#19181=CARTESIAN_POINT('Ctrl Pts',(2.43075995837453,2.11840690419145,28.2053109327814));
#19182=CARTESIAN_POINT('Ctrl Pts',(2.49570619507922,2.04149209539067,28.1995259562613));
#19183=CARTESIAN_POINT('Ctrl Pts',(2.5933502967196,1.91421755332677,28.1900854965365));
#19184=CARTESIAN_POINT('Ctrl Pts',(2.62842539247341,1.86576361463846,28.1865202649179));
#19185=CARTESIAN_POINT('Ctrl Pts',(2.67203403547143,1.80184917202555,28.1818398975896));
#19186=CARTESIAN_POINT('Ctrl Pts',(2.68181850609958,1.78725370520843,28.1807725865446));
#19187=CARTESIAN_POINT('Ctrl Pts',(2.69749960686758,1.76344353274449,28.1790335109529));
#19188=CARTESIAN_POINT('Ctrl Pts',(2.70346962117239,1.754277408212,28.1783645175095));
#19189=CARTESIAN_POINT('Ctrl Pts',(2.714836822928,1.73662882238479,28.1770772848122));
#19190=CARTESIAN_POINT('Ctrl Pts',(2.7202412176886,1.72815113800746,28.1764593249424));
#19191=CARTESIAN_POINT('Ctrl Pts',(2.73249302874545,1.70873228020672,28.175044619613));
#19192=CARTESIAN_POINT('Ctrl Pts',(2.73931452811414,1.69777503393014,28.1742469248899));
#19193=CARTESIAN_POINT('Ctrl Pts',(2.75719866560456,1.66865969404883,28.1721286418673));
#19194=CARTESIAN_POINT('Ctrl Pts',(2.76814759469602,1.65043282660585,28.1708039061596));
#19195=CARTESIAN_POINT('Ctrl Pts',(2.84851180265212,1.51359965977129,28.1608673305479));
#19196=CARTESIAN_POINT('Ctrl Pts',(2.91044829388982,1.39078585238741,28.1519868885576));
#19197=CARTESIAN_POINT('Ctrl Pts',(3.07225266434821,1.01144220168224,28.1246958417585));
#19198=CARTESIAN_POINT('Ctrl Pts',(3.14731893748563,0.745733117929703,28.1056640971676));
#19199=CARTESIAN_POINT('Ctrl Pts',(3.19690835386103,0.412048353809459,28.0835228103653));
#19200=CARTESIAN_POINT('Ctrl Pts',(3.2042839568045,0.350103425478123,28.0794907410019));
#19201=CARTESIAN_POINT('Ctrl Pts',(3.21093134597867,0.276010592693664,28.07479091633));
#19202=CARTESIAN_POINT('Ctrl Pts',(3.21193818098715,0.264036149225777,28.0740351806047));
#19203=CARTESIAN_POINT('Ctrl Pts',(3.21339276254581,0.245495068481021,28.0728712131674));
#19204=CARTESIAN_POINT('Ctrl Pts',(3.21388739670759,0.238932371501747,28.0724604236894));
#19205=CARTESIAN_POINT('Ctrl Pts',(3.21476401304575,0.226806086757986,28.0717036611553));
#19206=CARTESIAN_POINT('Ctrl Pts',(3.21515165535152,0.221243066530169,28.07135738207));
#19207=CARTESIAN_POINT('Ctrl Pts',(3.21599195248036,0.20871520250622,28.0705795532071));
#19208=CARTESIAN_POINT('Ctrl Pts',(3.21643642170772,0.201749898277124,28.0701484677452));
#19209=CARTESIAN_POINT('Ctrl Pts',(3.21751758941432,0.183894330845261,28.0690467792619));
#19210=CARTESIAN_POINT('Ctrl Pts',(3.21812163422095,0.173002076138211,28.0683779668696));
#19211=CARTESIAN_POINT('Ctrl Pts',(3.22136408164091,0.108622479298039,28.064442927649));
#19212=CARTESIAN_POINT('Ctrl Pts',(3.22272444204836,0.0550756954540183,
28.0612435129122));
#19213=CARTESIAN_POINT('Ctrl Pts',(3.2228698137111,-0.253878048904672,28.0430802842878));
#19214=CARTESIAN_POINT('Ctrl Pts',(3.19263149051261,-0.508405650129438,
28.0292239853636));
#19215=CARTESIAN_POINT('Ctrl Pts',(3.09404473860994,-0.916536046534449,
28.0055111022969));
#19216=CARTESIAN_POINT('Ctrl Pts',(3.04326992817971,-1.07314900636673,27.9960381728304));
#19217=CARTESIAN_POINT('Ctrl Pts',(2.97244162849883,-1.24546730509061,27.9848325130077));
#19218=CARTESIAN_POINT('Ctrl Pts',(2.9639018875871,-1.26565540621398,27.9835073693319));
#19219=CARTESIAN_POINT('Ctrl Pts',(2.94993064919438,-1.29776667241523,27.9813791001097));
#19220=CARTESIAN_POINT('Ctrl Pts',(2.94463113864726,-1.30974677722233,27.9805804831155));
#19221=CARTESIAN_POINT('Ctrl Pts',(2.9351236271155,-1.33089012412469,27.9791627203008));
#19222=CARTESIAN_POINT('Ctrl Pts',(2.93094536261163,-1.34006660530723,27.9785446050068));
#19223=CARTESIAN_POINT('Ctrl Pts',(2.92218138179114,-1.35907736154886,27.9772581960992));
#19224=CARTESIAN_POINT('Ctrl Pts',(2.91758892960006,-1.36890837386063,27.9765896751037));
#19225=CARTESIAN_POINT('Ctrl Pts',(2.90560043784443,-1.3942376243295,27.9748586632506));
#19226=CARTESIAN_POINT('Ctrl Pts',(2.89813008746458,-1.40970012244849,27.9737935958398));
#19227=CARTESIAN_POINT('Ctrl Pts',(2.86574534841454,-1.47538614238162,27.9692328019503));
#19228=CARTESIAN_POINT('Ctrl Pts',(2.8396475232972,-1.52501212372549,27.9656957978354));
#19229=CARTESIAN_POINT('Ctrl Pts',(2.76741372445882,-1.65407819803234,27.9562467089573));
#19230=CARTESIAN_POINT('Ctrl Pts',(2.71915542877751,-1.73226575513604,27.9502631335601));
#19231=CARTESIAN_POINT('Ctrl Pts',(2.53104417150926,-2.00977294184958,27.92808564831));
#19232=CARTESIAN_POINT('Ctrl Pts',(2.37208730220164,-2.19512155269858,27.9113411980645));
#19233=CARTESIAN_POINT('Ctrl Pts',(2.12673200897618,-2.42311969521352,27.8890616081365));
#19234=CARTESIAN_POINT('Ctrl Pts',(2.05703928030839,-2.48255732361178,27.8830701511568));
#19235=CARTESIAN_POINT('Ctrl Pts',(1.97394111242947,-2.54752186798342,27.8763891156045));
#19236=CARTESIAN_POINT('Ctrl Pts',(1.96292313737278,-2.55602111814378,27.8755122645675));
#19237=CARTESIAN_POINT('Ctrl Pts',(1.94622176959726,-2.56873284278501,27.8741970362539));
#19238=CARTESIAN_POINT('Ctrl Pts',(1.94057915915971,-2.57299827504003,27.8737550563143));
#19239=CARTESIAN_POINT('Ctrl Pts',(1.93045794271807,-2.58059699701065,27.8729665785583));
#19240=CARTESIAN_POINT('Ctrl Pts',(1.92598469257059,-2.58393724674888,27.872619596667));
#19241=CARTESIAN_POINT('Ctrl Pts',(1.91627694861952,-2.59114696404619,27.8718698360079));
#19242=CARTESIAN_POINT('Ctrl Pts',(1.91103942048759,-2.59501219037771,27.8714673526652));
#19243=CARTESIAN_POINT('Ctrl Pts',(1.89636739487758,-2.60577144069221,27.8703454103461));
#19244=CARTESIAN_POINT('Ctrl Pts',(1.88690694838235,-2.61263014515534,27.8696283657912));
#19245=CARTESIAN_POINT('Ctrl Pts',(1.83147959453778,-2.65235616708054,27.865463043079));
#19246=CARTESIAN_POINT('Ctrl Pts',(1.78468879618386,-2.68406362557993,27.8620893546808));
#19247=CARTESIAN_POINT('Ctrl Pts',(1.52323049267443,-2.85137654975856,27.8438650317798));
#19248=CARTESIAN_POINT('Ctrl Pts',(1.29393408151033,-2.96248899890195,27.8300867796373));
#19249=CARTESIAN_POINT('Ctrl Pts',(0.899230482662645,-3.09908172474494,
27.8064939488572));
#19250=CARTESIAN_POINT('Ctrl Pts',(0.740674528355421,-3.14075051844045,
27.7970590206089));
#19251=CARTESIAN_POINT('Ctrl Pts',(0.558103498970576,-3.1741326246658,27.7858958758337));
#19252=CARTESIAN_POINT('Ctrl Pts',(0.536515574185392,-3.17785280289918,
27.7845715598268));
#19253=CARTESIAN_POINT('Ctrl Pts',(0.501964126384027,-3.1834448449483,27.7824443689563));
#19254=CARTESIAN_POINT('Ctrl Pts',(0.489023971128397,-3.18545830497288,
27.7816459953445));
#19255=CARTESIAN_POINT('Ctrl Pts',(0.466100322918885,-3.18888220307942,
27.7802285141865));
#19256=CARTESIAN_POINT('Ctrl Pts',(0.456121751412183,-3.19032477349268,
27.7796104358032));
#19257=CARTESIAN_POINT('Ctrl Pts',(0.435388575861488,-3.19322284361722,
27.778323953687));
#19258=CARTESIAN_POINT('Ctrl Pts',(0.424633074340968,-3.19467088892615,
27.7776553218265));
#19259=CARTESIAN_POINT('Ctrl Pts',(0.396832323636302,-3.19827091397259,
27.7759237003514));
#19260=CARTESIAN_POINT('Ctrl Pts',(0.379776981062006,-3.20034094409897,
27.7748581307385));
#19261=CARTESIAN_POINT('Ctrl Pts',(0.306926621458607,-3.20859235250207,
27.7702922722666));
#19262=CARTESIAN_POINT('Ctrl Pts',(0.250994584633007,-3.21345140223122,
27.7667505916761));
#19263=CARTESIAN_POINT('Ctrl Pts',(0.103121815996642,-3.22241368507305,
27.7572858358354));
#19264=CARTESIAN_POINT('Ctrl Pts',(0.0110880832878357,-3.22404382618611,
27.7512909748323));
#19265=CARTESIAN_POINT('Ctrl Pts',(-0.322511287510997,-3.21566869440334,
27.7292143150351));
#19266=CARTESIAN_POINT('Ctrl Pts',(-0.562664986094939,-3.18244119714941,
27.712592776094));
#19267=CARTESIAN_POINT('Ctrl Pts',(-0.886877231683784,-3.09970995953979,
27.6903242884185));
#19268=CARTESIAN_POINT('Ctrl Pts',(-0.975892956717132,-3.07284713220161,
27.6842392585968));
#19269=CARTESIAN_POINT('Ctrl Pts',(-1.07680962772249,-3.03756374251452,
27.6774673688189));
#19270=CARTESIAN_POINT('Ctrl Pts',(-1.08995829745498,-3.03287048694802,
27.6765875863793));
#19271=CARTESIAN_POINT('Ctrl Pts',(-1.10973159759125,-3.02566744934744,
27.6752688339925));
#19272=CARTESIAN_POINT('Ctrl Pts',(-1.11637892962338,-3.02322110016826,
27.6748262332957));
#19273=CARTESIAN_POINT('Ctrl Pts',(-1.12825175385037,-3.01880716805993,
27.674037085855));
#19274=CARTESIAN_POINT('Ctrl Pts',(-1.13348023036993,-3.01684790914915,
27.6736900515636));
#19275=CARTESIAN_POINT('Ctrl Pts',(-1.14478644820545,-3.01257760535221,
27.6729406750253));
#19276=CARTESIAN_POINT('Ctrl Pts',(-1.15086227722091,-3.01026175953171,
27.6725386255255));
#19277=CARTESIAN_POINT('Ctrl Pts',(-1.1678065109035,-3.00374454423159,27.6714191174302));
#19278=CARTESIAN_POINT('Ctrl Pts',(-1.17865933057876,-2.99950254642598,
27.6707040563288));
#19279=CARTESIAN_POINT('Ctrl Pts',(-1.24150512116496,-2.97454450017287,
27.6665735563675));
#19280=CARTESIAN_POINT('Ctrl Pts',(-1.29297790424187,-2.95253432964939,
27.6632312580994));
#19281=CARTESIAN_POINT('Ctrl Pts',(-1.3881557296679,-2.90886866196291,27.6570810831785));
#19282=CARTESIAN_POINT('Ctrl Pts',(-1.43196670842019,-2.8875525283001,27.6542624077881));
#19283=CARTESIAN_POINT('Ctrl Pts',(-1.47525554463427,-2.8652641484732,27.6514736540563));
#19284=CARTESIAN_POINT('',(3.21884143381304,0.00209368326018609,27.8142265507269));
#19285=CARTESIAN_POINT('Ctrl Pts',(-1.47306432504222,-2.86105893806616,
27.4070470808673));
#19286=CARTESIAN_POINT('Ctrl Pts',(-1.07391560553436,-3.06878928672532,
27.4347289377229));
#19287=CARTESIAN_POINT('Ctrl Pts',(0.418901930152219,-3.50240078110557,
27.528721774033));
#19288=CARTESIAN_POINT('Ctrl Pts',(2.67358561891793,-2.43681984067852,27.6644482639862));
#19289=CARTESIAN_POINT('Ctrl Pts',(3.21482490205533,-0.675841793750365,
27.7724928970838));
#19290=CARTESIAN_POINT('Ctrl Pts',(3.21884143381304,0.00209368326018609,
27.8142265507269));
#19291=CARTESIAN_POINT('Ctrl Pts',(3.22274921939152,0.00224308077548155,
27.8119771806639));
#19292=CARTESIAN_POINT('Ctrl Pts',(3.22257607314387,0.251011177117484,27.8282186241532));
#19293=CARTESIAN_POINT('Ctrl Pts',(3.1935980450414,0.498915594153727,27.8452516809599));
#19294=CARTESIAN_POINT('Ctrl Pts',(3.11031910459803,0.851415556667762,27.8695745293279));
#19295=CARTESIAN_POINT('Ctrl Pts',(3.07841230804907,0.960404269788171,27.8770937384884));
#19296=CARTESIAN_POINT('Ctrl Pts',(3.03363325978313,1.08796018786871,27.8857242084574));
#19297=CARTESIAN_POINT('Ctrl Pts',(3.02624122259666,1.10835565049853,27.8870987860038));
#19298=CARTESIAN_POINT('Ctrl Pts',(3.01571870519125,1.13649813074565,27.8889864768415));
#19299=CARTESIAN_POINT('Ctrl Pts',(3.01276339773523,1.14430940876292,27.889509460113));
#19300=CARTESIAN_POINT('Ctrl Pts',(3.0077122949801,1.15750494297383,27.8903911848325));
#19301=CARTESIAN_POINT('Ctrl Pts',(3.00563233826743,1.16289517639047,27.8907508647554));
#19302=CARTESIAN_POINT('Ctrl Pts',(3.00164236546227,1.17315302199276,27.8914343676146));
#19303=CARTESIAN_POINT('Ctrl Pts',(2.9997349884051,1.17802160566625,27.891758351038));
#19304=CARTESIAN_POINT('Ctrl Pts',(2.99469697702712,1.19078956082788,27.892606951605));
#19305=CARTESIAN_POINT('Ctrl Pts',(2.99154691090777,1.19868129462142,27.8931304028289));
#19306=CARTESIAN_POINT('Ctrl Pts',(2.98048912814422,1.22606881118217,27.8949436094309));
#19307=CARTESIAN_POINT('Ctrl Pts',(2.97242155166803,1.24550003840723,27.8962240925894));
#19308=CARTESIAN_POINT('Ctrl Pts',(2.86462766411943,1.49811370527821,27.9128101040785));
#19309=CARTESIAN_POINT('Ctrl Pts',(2.73788882694887,1.71884910249097,27.9266727029701));
#19310=CARTESIAN_POINT('Ctrl Pts',(2.51225204886022,2.02242967384565,27.9478690919664));
#19311=CARTESIAN_POINT('Ctrl Pts',(2.43222102155652,2.11800137929118,27.9549062916998));
#19312=CARTESIAN_POINT('Ctrl Pts',(2.30689457976131,2.25116777397641,27.9655186265763));
#19313=CARTESIAN_POINT('Ctrl Pts',(2.26578064690093,2.29254365810444,27.9689420244304));
#19314=CARTESIAN_POINT('Ctrl Pts',(2.20402952564179,2.35140384540231,27.9740190152276));
#19315=CARTESIAN_POINT('Ctrl Pts',(2.18425782009189,2.36978140426878,27.9756352945981));
#19316=CARTESIAN_POINT('Ctrl Pts',(2.14826715620852,2.40240120467486,27.978562607641));
#19317=CARTESIAN_POINT('Ctrl Pts',(2.13213141452947,2.41673310874959,27.9798698062973));
#19318=CARTESIAN_POINT('Ctrl Pts',(2.10697029466606,2.43863331107665,27.981900827569));
#19319=CARTESIAN_POINT('Ctrl Pts',(2.09804512935101,2.44631618518651,27.9826198682644));
#19320=CARTESIAN_POINT('Ctrl Pts',(2.08899527053964,2.45402044286706,27.9833476023839));
#19321=CARTESIAN_POINT('Ctrl Pts',(2.08891239022315,2.45409099267298,27.9833542669965));
#19322=CARTESIAN_POINT('Ctrl Pts',(2.08874529176614,2.4542332164761,27.9833677035697));
#19323=CARTESIAN_POINT('Ctrl Pts',(2.08866107351799,2.45430489033056,27.9833744755353));
#19324=CARTESIAN_POINT('Ctrl Pts',(2.08849125527679,2.45444939890083,27.9833881303352));
#19325=CARTESIAN_POINT('Ctrl Pts',(2.08840565516912,2.45452223346824,27.9833950131749));
#19326=CARTESIAN_POINT('Ctrl Pts',(2.08823302754129,2.45466910157774,27.9834088933833));
#19327=CARTESIAN_POINT('Ctrl Pts',(2.08814599989535,2.45474313496867,27.9834158907581));
#19328=CARTESIAN_POINT('Ctrl Pts',(2.08797046964609,2.45489244039011,27.9834300038475));
#19329=CARTESIAN_POINT('Ctrl Pts',(2.08788196692128,2.45496771225276,27.9834371195675));
#19330=CARTESIAN_POINT('Ctrl Pts',(2.08770343710085,2.45511953582353,27.9834514733073));
#19331=CARTESIAN_POINT('Ctrl Pts',(2.08761340984913,2.4551960873794,27.9834587113353));
#19332=CARTESIAN_POINT('Ctrl Pts',(2.08746200265783,2.45532481689282,27.9834708839738));
#19333=CARTESIAN_POINT('Ctrl Pts',(2.08740062496582,2.45537699750615,27.9834758184754));
#19334=CARTESIAN_POINT('Ctrl Pts',(2.08727283071188,2.45548563430343,27.9834860924525));
#19335=CARTESIAN_POINT('Ctrl Pts',(2.08720641383123,2.45554209008118,27.983491431943));
#19336=CARTESIAN_POINT('Ctrl Pts',(2.08706807579079,2.45565967072472,27.9835025532808));
#19337=CARTESIAN_POINT('Ctrl Pts',(2.08699615423903,2.45572079512318,27.9835083351472));
#19338=CARTESIAN_POINT('Ctrl Pts',(2.08684629011748,2.45584814969989,27.9835203827395));
#19339=CARTESIAN_POINT('Ctrl Pts',(2.08676834707553,2.45591437933108,27.9835266484884));
#19340=CARTESIAN_POINT('Ctrl Pts',(2.08660586485907,2.45605243012866,27.9835397100328));
#19341=CARTESIAN_POINT('Ctrl Pts',(2.08652132514239,2.45612425062967,27.9835465058541));
#19342=CARTESIAN_POINT('Ctrl Pts',(2.08634500801427,2.45627402472399,27.9835606790614));
#19343=CARTESIAN_POINT('Ctrl Pts',(2.08625322993715,2.45635197754244,27.9835680564799));
#19344=CARTESIAN_POINT('Ctrl Pts',(2.08606171846324,2.45651462165027,27.9835834505016));
#19345=CARTESIAN_POINT('Ctrl Pts',(2.08596198426455,2.45659931202109,27.9835914671443));
#19346=CARTESIAN_POINT('Ctrl Pts',(2.0857537555314,2.45677610987276,27.9836082042443));
#19347=CARTESIAN_POINT('Ctrl Pts',(2.08564526007494,2.45686821622198,27.9836169247457));
#19348=CARTESIAN_POINT('Ctrl Pts',(2.08541860331951,2.45706060882681,27.9836351422523));
#19349=CARTESIAN_POINT('Ctrl Pts',(2.08530044088219,2.45716089375034,27.9836446393129));
#19350=CARTESIAN_POINT('Ctrl Pts',(2.08505342827,2.45737050367132,27.9836644919592));
#19351=CARTESIAN_POINT('Ctrl Pts',(2.08492457674086,2.45747982704971,27.9836748476105));
#19352=CARTESIAN_POINT('Ctrl Pts',(2.08465502725945,2.45770848838087,27.9836965104265));
#19353=CARTESIAN_POINT('Ctrl Pts',(2.08451432765261,2.45782782438952,27.9837078176721));
#19354=CARTESIAN_POINT('Ctrl Pts',(2.08421977720324,2.45807760729837,27.9837314883751));
#19355=CARTESIAN_POINT('Ctrl Pts',(2.08406591899574,2.45820805638353,27.983743852361));
#19356=CARTESIAN_POINT('Ctrl Pts',(2.08374354384588,2.45848133097957,27.9837697574909));
#19357=CARTESIAN_POINT('Ctrl Pts',(2.08357502609899,2.45862415222707,27.983783298622));
#19358=CARTESIAN_POINT('Ctrl Pts',(2.08327991972498,2.45887420704946,27.9838070108846));
#19359=CARTESIAN_POINT('Ctrl Pts',(2.08315334029556,2.45898144581048,27.9838171814793));
#19360=CARTESIAN_POINT('Ctrl Pts',(2.08282680123457,2.45925804811655,27.9838434180564));
#19361=CARTESIAN_POINT('Ctrl Pts',(2.08262683195259,2.4594273947406,27.9838594844227));
#19362=CARTESIAN_POINT('Ctrl Pts',(2.08210727006256,2.4598672837748,27.9839012264972));
#19363=CARTESIAN_POINT('Ctrl Pts',(2.08178764721452,2.46013778673742,27.9839269036214));
#19364=CARTESIAN_POINT('Ctrl Pts',(2.07377182236681,2.46691905276118,27.98457081878));
#19365=CARTESIAN_POINT('Ctrl Pts',(2.06604523529416,2.47339367391275,27.9851905356148));
#19366=CARTESIAN_POINT('Ctrl Pts',(2.04820544090066,2.48820090474618,27.9866192548276));
#19367=CARTESIAN_POINT('Ctrl Pts',(2.03807158744352,2.49650825490682,27.9874292731499));
#19368=CARTESIAN_POINT('Ctrl Pts',(2.01083480395291,2.51855957954558,27.9896023672832));
#19369=CARTESIAN_POINT('Ctrl Pts',(1.99364194249327,2.53219089548667,27.9909699417642));
#19370=CARTESIAN_POINT('Ctrl Pts',(1.84747586323729,2.64566692077758,28.0025635483795));
#19371=CARTESIAN_POINT('Ctrl Pts',(1.71125339721264,2.73574813183232,28.0131730544195));
#19372=CARTESIAN_POINT('Ctrl Pts',(1.34819853107613,2.93807203849513,28.0408887938268));
#19373=CARTESIAN_POINT('Ctrl Pts',(1.11390373337955,3.03465317275966,28.0583184593761));
#19374=CARTESIAN_POINT('Ctrl Pts',(0.814657340601489,3.11862857407769,28.0786729404069));
#19375=CARTESIAN_POINT('Ctrl Pts',(0.758151901353665,3.1328449477799,28.0824325500714));
#19376=CARTESIAN_POINT('Ctrl Pts',(0.689785591019008,3.14808708364392,28.0868564777877));
#19377=CARTESIAN_POINT('Ctrl Pts',(0.678268845443517,3.15058848966412,28.0875974892631));
#19378=CARTESIAN_POINT('Ctrl Pts',(0.660350015807509,3.15437760197879,28.0887435853003));
#19379=CARTESIAN_POINT('Ctrl Pts',(0.653957443689285,3.15570909034423,28.0891511076388));
#19380=CARTESIAN_POINT('Ctrl Pts',(0.642095993973149,3.15814208319243,28.0899047102472));
#19381=CARTESIAN_POINT('Ctrl Pts',(0.636628352748044,3.15924880696951,28.09025107791));
#19382=CARTESIAN_POINT('Ctrl Pts',(0.624253987844057,3.16172011471793,28.0910327101437));
#19383=CARTESIAN_POINT('Ctrl Pts',(0.61734566776465,3.16307626431387,28.0914674886988));
#19384=CARTESIAN_POINT('Ctrl Pts',(0.59691599291627,3.1670172663204,28.0927486971762));
#19385=CARTESIAN_POINT('Ctrl Pts',(0.583382255670844,3.16953817254749,28.0935915660775));
#19386=CARTESIAN_POINT('Ctrl Pts',(0.483748943329586,3.18743690988595,28.0997562607256));
#19387=CARTESIAN_POINT('Ctrl Pts',(0.397062934537069,3.19939229983461,28.1048987659791));
#19388=CARTESIAN_POINT('Ctrl Pts',(0.0623539005114043,3.23173728192384,
28.1242752762209));
#19389=CARTESIAN_POINT('Ctrl Pts',(-0.187229242884563,3.22691404424233,
28.1377811631889));
#19390=CARTESIAN_POINT('Ctrl Pts',(-0.524118949688076,3.18115193908655,
28.1571436545183));
#19391=CARTESIAN_POINT('Ctrl Pts',(-0.613885474878969,3.16505467031161,
28.1624074400635));
#19392=CARTESIAN_POINT('Ctrl Pts',(-0.757263198003658,3.13301441173895,
28.1710720742139));
#19393=CARTESIAN_POINT('Ctrl Pts',(-0.811354530415077,3.11944387908896,
28.1744007979795));
#19394=CARTESIAN_POINT('Ctrl Pts',(-0.881570880155421,3.09987805720281,
28.1788118352579));
#19395=CARTESIAN_POINT('Ctrl Pts',(-0.898040275123139,3.09514698082008,
28.1798529804518));
#19396=CARTESIAN_POINT('Ctrl Pts',(-0.924865532663639,3.08720890426697,
28.1815597870033));
#19397=CARTESIAN_POINT('Ctrl Pts',(-0.935244463482718,3.08408055359756,
28.182222866838));
#19398=CARTESIAN_POINT('Ctrl Pts',(-0.955245465200354,3.07794173248781,
28.1835059776897));
#19399=CARTESIAN_POINT('Ctrl Pts',(-0.964869592864692,3.07493835262666,
28.1841257690598));
#19400=CARTESIAN_POINT('Ctrl Pts',(-0.986976702521,3.06792543115246,28.185555019243));
#19401=CARTESIAN_POINT('Ctrl Pts',(-0.999449561716827,3.06388479350141,
28.1863654964604));
#19402=CARTESIAN_POINT('Ctrl Pts',(-1.03275239016484,3.05287120065304,28.1885406226128));
#19403=CARTESIAN_POINT('Ctrl Pts',(-1.05353601949692,3.04576129796855,28.1899097834372));
#19404=CARTESIAN_POINT('Ctrl Pts',(-1.22782880847757,2.98413981823065,28.2014924303112));
#19405=CARTESIAN_POINT('Ctrl Pts',(-1.37705056332874,2.91828225952964,28.2120883586319));
#19406=CARTESIAN_POINT('Ctrl Pts',(-1.74306767766489,2.72240289107818,28.2397703227242));
#19407=CARTESIAN_POINT('Ctrl Pts',(-1.95073956424826,2.577668002044,28.2571794558204));
#19408=CARTESIAN_POINT('Ctrl Pts',(-2.18326933659519,2.37126396516293,28.2775460223032));
#19409=CARTESIAN_POINT('Ctrl Pts',(-2.22606677235845,2.33113396004733,28.2813322407518));
#19410=CARTESIAN_POINT('Ctrl Pts',(-2.27613796553347,2.28154617693156,28.2857831833612));
#19411=CARTESIAN_POINT('Ctrl Pts',(-2.28448243609273,2.27319093016324,28.2865256720649));
#19412=CARTESIAN_POINT('Ctrl Pts',(-2.29737323038721,2.26014081540648,28.2876735533898));
#19413=CARTESIAN_POINT('Ctrl Pts',(-2.30195141261688,2.25547776777263,28.2880813957598));
#19414=CARTESIAN_POINT('Ctrl Pts',(-2.31041124451165,2.246808527487,28.2888352916699));
#19415=CARTESIAN_POINT('Ctrl Pts',(-2.31429664178473,2.24280621823188,28.2891816344996));
#19416=CARTESIAN_POINT('Ctrl Pts',(-2.32305771646215,2.23373451359271,28.2899628333745));
#19417=CARTESIAN_POINT('Ctrl Pts',(-2.32792718908079,2.22865924622503,28.2903972057273));
#19418=CARTESIAN_POINT('Ctrl Pts',(-2.34225664283052,2.21362599170567,28.2916761079214));
#19419=CARTESIAN_POINT('Ctrl Pts',(-2.35166976523652,2.20362327608519,28.2925170958168));
#19420=CARTESIAN_POINT('Ctrl Pts',(-2.41998729411171,2.13009032611836,28.2986298395416));
#19421=CARTESIAN_POINT('Ctrl Pts',(-2.47637824169873,2.06426185303856,28.3037256803751));
#19422=CARTESIAN_POINT('Ctrl Pts',(-2.68662498248649,1.79779252691876,28.3232922850509));
#19423=CARTESIAN_POINT('Ctrl Pts',(-2.81931375597962,1.58161236519609,28.3370021425064));
#19424=CARTESIAN_POINT('Ctrl Pts',(-2.96278569365995,1.27120688746138,28.356495879952));
#19425=CARTESIAN_POINT('Ctrl Pts',(-2.99681444426538,1.18876718280264,28.3616484392442));
#19426=CARTESIAN_POINT('Ctrl Pts',(-3.04619657884746,1.05347774459922,28.3701464831773));
#19427=CARTESIAN_POINT('Ctrl Pts',(-3.06369206125675,1.00145862039529,28.3734234203789));
#19428=CARTESIAN_POINT('Ctrl Pts',(-3.08486723836728,0.932738945623363,
28.377775370779));
#19429=CARTESIAN_POINT('Ctrl Pts',(-3.08975492775471,0.916418184076646,
28.3788106042556));
#19430=CARTESIAN_POINT('Ctrl Pts',(-3.0975343353287,0.889671649575213,28.3805101598316));
#19431=CARTESIAN_POINT('Ctrl Pts',(-3.10050340540402,0.879268577376793,
28.3811719427035));
#19432=CARTESIAN_POINT('Ctrl Pts',(-3.10614027082547,0.859134441693939,
28.3824542709243));
#19433=CARTESIAN_POINT('Ctrl Pts',(-3.10881486019964,0.849405399237961,
28.3830745858877));
#19434=CARTESIAN_POINT('Ctrl Pts',(-3.11487295958612,0.826956617192837,
28.384507536301));
#19435=CARTESIAN_POINT('Ctrl Pts',(-3.11822430483926,0.814228455365824,
28.3853212072951));
#19436=CARTESIAN_POINT('Ctrl Pts',(-3.12700390657879,0.780034843515834,
28.3875104938558));
#19437=CARTESIAN_POINT('Ctrl Pts',(-3.13228900254007,0.758533686731404,
28.3888907139592));
#19438=CARTESIAN_POINT('Ctrl Pts',(-3.18770001294623,0.522646962907515,
28.4040745982243));
#19439=CARTESIAN_POINT('Ctrl Pts',(-3.21594261043893,0.303760319097149,
28.418601064146));
#19440=CARTESIAN_POINT('Ctrl Pts',(-3.22573092070898,-0.0727969716174191,
28.444009805387));
#19441=CARTESIAN_POINT('Ctrl Pts',(-3.2183852464577,-0.229428189198327,
28.4546842291684));
#19442=CARTESIAN_POINT('Ctrl Pts',(-3.19207297921126,-0.448158922934147,
28.469345485301));
#19443=CARTESIAN_POINT('Ctrl Pts',(-3.18258959060561,-0.51117594651035,
28.4735385197517));
#19444=CARTESIAN_POINT('Ctrl Pts',(-3.16696442362315,-0.59752103879161,
28.4792060028004));
#19445=CARTESIAN_POINT('Ctrl Pts',(-3.16242072979904,-0.621120161174069,
28.4807468889327));
#19446=CARTESIAN_POINT('Ctrl Pts',(-3.15412308036939,-0.661762490831342,
28.4833840558576));
#19447=CARTESIAN_POINT('Ctrl Pts',(-3.15049394862088,-0.6788298107568,28.4844864423929));
#19448=CARTESIAN_POINT('Ctrl Pts',(-3.1450742742891,-0.70333769149491,28.4860612957598));
#19449=CARTESIAN_POINT('Ctrl Pts',(-3.14339564384017,-0.71080231303224,
28.4865398776583));
#19450=CARTESIAN_POINT('Ctrl Pts',(-3.14043101691081,-0.72376966104113,
28.4873692801408));
#19451=CARTESIAN_POINT('Ctrl Pts',(-3.13915710809486,-0.729275083153306,
28.4877207888519));
#19452=CARTESIAN_POINT('Ctrl Pts',(-3.13646068134632,-0.740790182765554,
28.4884546681015));
#19453=CARTESIAN_POINT('Ctrl Pts',(-3.13503536907279,-0.746799127407396,
28.4888368753577));
#19454=CARTESIAN_POINT('Ctrl Pts',(-3.13121430848532,-0.762704526290787,
28.4898466509665));
#19455=CARTESIAN_POINT('Ctrl Pts',(-3.1287888932895,-0.772593882862759,
28.4904725291888));
#19456=CARTESIAN_POINT('Ctrl Pts',(-3.11831393122708,-0.814445935150837,
28.4931135910754));
#19457=CARTESIAN_POINT('Ctrl Pts',(-3.10982083949059,-0.846296931862167,
28.4951045430408));
#19458=CARTESIAN_POINT('Ctrl Pts',(-3.00932650970986,-1.20120819765783,
28.5171336328838));
#19459=CARTESIAN_POINT('Ctrl Pts',(-2.86783908636949,-1.50815085994854,
28.5349257467128));
#19460=CARTESIAN_POINT('Ctrl Pts',(-2.61859242532193,-1.88200172304735,
28.5607348492581));
#19461=CARTESIAN_POINT('Ctrl Pts',(-2.55081475842756,-1.9728904394345,28.5673737263348));
#19462=CARTESIAN_POINT('Ctrl Pts',(-2.46473523618494,-2.07645240823694,
28.5754924658662));
#19463=CARTESIAN_POINT('Ctrl Pts',(-2.45091016842202,-2.0927526610991,28.5767874914401));
#19464=CARTESIAN_POINT('Ctrl Pts',(-2.42922117196581,-2.11781505994916,
28.5788061063841));
#19465=CARTESIAN_POINT('Ctrl Pts',(-2.42146947602971,-2.12667385871358,
28.5795250407584));
#19466=CARTESIAN_POINT('Ctrl Pts',(-2.4077331227778,-2.14219957808712,28.5807947102052));
#19467=CARTESIAN_POINT('Ctrl Pts',(-2.40176884148812,-2.1488844204272,28.5813445862375));
#19468=CARTESIAN_POINT('Ctrl Pts',(-2.38809389098022,-2.16408342609565,
28.5826021947668));
#19469=CARTESIAN_POINT('Ctrl Pts',(-2.38036545228784,-2.17258137139112,
28.583310676397));
#19470=CARTESIAN_POINT('Ctrl Pts',(-2.35936430081158,-2.19542699191894,
28.5852299433384));
#19471=CARTESIAN_POINT('Ctrl Pts',(-2.34600638830898,-2.20969535901384,
28.5864443664798));
#19472=CARTESIAN_POINT('Ctrl Pts',(-2.28121362315127,-2.2776545333578,28.5923056407815));
#19473=CARTESIAN_POINT('Ctrl Pts',(-2.22806435475452,-2.32967240789121,
28.59702695154));
#19474=CARTESIAN_POINT('Ctrl Pts',(-2.12735875441497,-2.42163386167715,
28.6058257864524));
#19475=CARTESIAN_POINT('Ctrl Pts',(-2.08035433042835,-2.46213138061419,
28.6098784692821));
#19476=CARTESIAN_POINT('Ctrl Pts',(-1.86440644164759,-2.6375848025991,28.6282463302184));
#19477=CARTESIAN_POINT('Ctrl Pts',(-1.68331208770662,-2.75668492091963,
28.6430345672061));
#19478=CARTESIAN_POINT('Ctrl Pts',(-1.48621546801644,-2.8596012301885,28.6579680349496));
#19479=CARTESIAN_POINT('Ctrl Pts',(-1.48073943600392,-2.86244062514127,
28.6583820282506));
#19480=CARTESIAN_POINT('Ctrl Pts',(-1.47525540425972,-2.86526422074867,
28.6587956971472));
#19481=CARTESIAN_POINT('Origin',(0.,0.,4.68922655072688));
#19482=CARTESIAN_POINT('',(-1.47525540759407,-2.86526421903189,30.1566970682534));
#19483=CARTESIAN_POINT('',(-1.47525514454518,-2.86526435446941,29.9088139162969));
#19484=CARTESIAN_POINT('',(-1.47525540501186,-2.86526422036142,4.68922655072688));
#19485=CARTESIAN_POINT('',(3.22274868255297,-0.00291403553407739,29.310403850828));
#19486=CARTESIAN_POINT('Ctrl Pts',(-1.47525540759407,-2.86526421903189,
30.1566970682534));
#19487=CARTESIAN_POINT('Ctrl Pts',(-1.50490610286469,-2.84999779150791,
30.154597938539));
#19488=CARTESIAN_POINT('Ctrl Pts',(-1.53431835049294,-2.83427187172883,
30.1524827770642));
#19489=CARTESIAN_POINT('Ctrl Pts',(-1.64400800730423,-2.77341588983146,
30.1444684001732));
#19490=CARTESIAN_POINT('Ctrl Pts',(-1.72257584965478,-2.72531244714196,
30.1384684071173));
#19491=CARTESIAN_POINT('Ctrl Pts',(-1.99881463056546,-2.53946301663847,
30.1164416417455));
#19492=CARTESIAN_POINT('Ctrl Pts',(-2.18293532940145,-2.38304657637613,
30.0998803456669));
#19493=CARTESIAN_POINT('Ctrl Pts',(-2.41203203292022,-2.13938840339235,
30.0776166587306));
#19494=CARTESIAN_POINT('Ctrl Pts',(-2.47316296225755,-2.06841722126229,
30.0714850674834));
#19495=CARTESIAN_POINT('Ctrl Pts',(-2.5397775560768,-1.9838959275375,30.0646680376241));
#19496=CARTESIAN_POINT('Ctrl Pts',(-2.54836160950185,-1.97285737181948,
30.0637868364812));
#19497=CARTESIAN_POINT('Ctrl Pts',(-2.56118825328611,-1.95613970131652,
30.0624663789496));
#19498=CARTESIAN_POINT('Ctrl Pts',(-2.5654842668996,-1.95050205803763,30.0620234781831));
#19499=CARTESIAN_POINT('Ctrl Pts',(-2.57313142474656,-1.94039774611296,
30.0612340066121));
#19500=CARTESIAN_POINT('Ctrl Pts',(-2.57648958087305,-1.93593651326108,
30.060886946582));
#19501=CARTESIAN_POINT('Ctrl Pts',(-2.58373102965776,-1.92626419842136,
30.0601377538574));
#19502=CARTESIAN_POINT('Ctrl Pts',(-2.58761014880304,-1.92105010744374,
30.0597359126225));
#19503=CARTESIAN_POINT('Ctrl Pts',(-2.59839098708726,-1.90646721622962,
30.0586175725132));
#19504=CARTESIAN_POINT('Ctrl Pts',(-2.60525785831271,-1.89707260526927,
30.05790346303));
#19505=CARTESIAN_POINT('Ctrl Pts',(-2.64470485135637,-1.84248676699358,
30.0537895354871));
#19506=CARTESIAN_POINT('Ctrl Pts',(-2.67616186533482,-1.79649096180906,
30.0504621736318));
#19507=CARTESIAN_POINT('Ctrl Pts',(-2.8445781288749,-1.53598686739862,30.0322402161111));
#19508=CARTESIAN_POINT('Ctrl Pts',(-2.95695714947211,-1.30664163470692,
30.0184311705247));
#19509=CARTESIAN_POINT('Ctrl Pts',(-3.09545853092004,-0.911675496904819,
29.9947905460419));
#19510=CARTESIAN_POINT('Ctrl Pts',(-3.13783021194043,-0.753011836779592,
29.9853401520876));
#19511=CARTESIAN_POINT('Ctrl Pts',(-3.17196637725484,-0.570286756058514,
29.9741597063892));
#19512=CARTESIAN_POINT('Ctrl Pts',(-3.17577038064421,-0.548707696021086,
29.9728350528568));
#19513=CARTESIAN_POINT('Ctrl Pts',(-3.18149611941506,-0.514170740524261,
29.970707422226));
#19514=CARTESIAN_POINT('Ctrl Pts',(-3.18355945428613,-0.501236771736976,
29.9699089493559));
#19515=CARTESIAN_POINT('Ctrl Pts',(-3.18707151827445,-0.478324532890017,
29.9684913533374));
#19516=CARTESIAN_POINT('Ctrl Pts',(-3.18855237811255,-0.468351310154998,
29.9678732599077));
#19517=CARTESIAN_POINT('Ctrl Pts',(-3.19152985868076,-0.447629854386223,
29.9665868076826));
#19518=CARTESIAN_POINT('Ctrl Pts',(-3.1930190381003,-0.436880696650159,
29.9659182210636));
#19519=CARTESIAN_POINT('Ctrl Pts',(-3.19672512506709,-0.409097903782639,
29.9641868483567));
#19520=CARTESIAN_POINT('Ctrl Pts',(-3.19886016688344,-0.392053866741262,
29.9631214836763));
#19521=CARTESIAN_POINT('Ctrl Pts',(-3.20738727843857,-0.319268456753296,
29.9585576925809));
#19522=CARTESIAN_POINT('Ctrl Pts',(-3.21245904686602,-0.263385145945472,
29.955017921029));
#19523=CARTESIAN_POINT('Ctrl Pts',(-3.22198659378827,-0.115645711667687,
29.9455595619427));
#19524=CARTESIAN_POINT('Ctrl Pts',(-3.22397393531682,-0.0236871870202732,
29.939569309236));
#19525=CARTESIAN_POINT('Ctrl Pts',(-3.21689571194008,0.310597353811148,
29.91745003743));
#19526=CARTESIAN_POINT('Ctrl Pts',(-3.18443400471036,0.551592131422609,
29.9007767585704));
#19527=CARTESIAN_POINT('Ctrl Pts',(-3.10272593463277,0.876205680846315,
29.8785038258521));
#19528=CARTESIAN_POINT('Ctrl Pts',(-3.07634491150773,0.964753882003094,
29.8724584314665));
#19529=CARTESIAN_POINT('Ctrl Pts',(-3.04164295766476,1.06523239009345,29.8657250030753));
#19530=CARTESIAN_POINT('Ctrl Pts',(-3.03700626142552,1.0783806894635,29.8648464491974));
#19531=CARTESIAN_POINT('Ctrl Pts',(-3.02988673806894,1.09815938237161,29.8635291736297));
#19532=CARTESIAN_POINT('Ctrl Pts',(-3.02746721971465,1.1048121607055,29.8630868329737));
#19533=CARTESIAN_POINT('Ctrl Pts',(-3.02310025304166,1.11669762895154,29.8622979662095));
#19534=CARTESIAN_POINT('Ctrl Pts',(-3.02116111639402,1.12193326219123,29.8619509540083));
#19535=CARTESIAN_POINT('Ctrl Pts',(-3.01693315721173,1.13325822474451,29.861201417195));
#19536=CARTESIAN_POINT('Ctrl Pts',(-3.01463950802597,1.13934565319328,29.8607991864493));
#19537=CARTESIAN_POINT('Ctrl Pts',(-3.00818118580303,1.15633023222274,29.8596786616032));
#19538=CARTESIAN_POINT('Ctrl Pts',(-3.00397570337287,1.16721190698896,29.8589627720606));
#19539=CARTESIAN_POINT('Ctrl Pts',(-2.97917000023897,1.23037445263301,29.8548177738978));
#19540=CARTESIAN_POINT('Ctrl Pts',(-2.9572629226252,1.28213574929113,29.8514624073917));
#19541=CARTESIAN_POINT('Ctrl Pts',(-2.82887585685594,1.56465944789737,29.8332390918432));
#19542=CARTESIAN_POINT('Ctrl Pts',(-2.6967347660721,1.78279182494002,29.8194487141062));
#19543=CARTESIAN_POINT('Ctrl Pts',(-2.43950448500101,2.11229207460431,29.795836995626));
#19544=CARTESIAN_POINT('Ctrl Pts',(-2.32899849705148,2.23354326204648,29.786395902388));
#19545=CARTESIAN_POINT('Ctrl Pts',(-2.19381695475127,2.36088218734613,29.7752258613584));
#19546=CARTESIAN_POINT('Ctrl Pts',(-2.17771735488412,2.37574085695693,29.7739014106908));
#19547=CARTESIAN_POINT('Ctrl Pts',(-2.15175360627969,2.3992176850227,29.7717740443706));
#19548=CARTESIAN_POINT('Ctrl Pts',(-2.141986064573,2.40794202037586,29.7709756311572));
#19549=CARTESIAN_POINT('Ctrl Pts',(-2.12460532064257,2.42327700639462,29.7695581041739));
#19550=CARTESIAN_POINT('Ctrl Pts',(-2.11701372012307,2.42991195794515,29.7689400197886));
#19551=CARTESIAN_POINT('Ctrl Pts',(-2.10118646647693,2.44361428377264,29.7676535496038));
#19552=CARTESIAN_POINT('Ctrl Pts',(-2.09294601058157,2.45067589185952,29.7669849357982));
#19553=CARTESIAN_POINT('Ctrl Pts',(-2.07156912354722,2.46880822541172,29.7652534135996));
#19554=CARTESIAN_POINT('Ctrl Pts',(-2.0583796866194,2.47981566548539,29.7641879257696));
#19555=CARTESIAN_POINT('Ctrl Pts',(-2.00172712233524,2.52633252606068,29.7596228924428));
#19556=CARTESIAN_POINT('Ctrl Pts',(-1.95743058142145,2.56080697913076,29.7560819738151));
#19557=CARTESIAN_POINT('Ctrl Pts',(-1.83821555419165,2.6486869656554,29.7466197713309));
#19558=CARTESIAN_POINT('Ctrl Pts',(-1.76187566129761,2.70006864616016,29.7406267498669));
#19559=CARTESIAN_POINT('Ctrl Pts',(-1.49558015937302,2.86319692247284,29.7199671586201));
#19560=CARTESIAN_POINT('Ctrl Pts',(-1.29641039046421,2.95870987086433,29.7048734255436));
#19561=CARTESIAN_POINT('Ctrl Pts',(-1.04907995493489,3.04751626004872,29.6872705465333));
#19562=CARTESIAN_POINT('Ctrl Pts',(-1.00879545775868,3.06108739848742,29.684439599267));
#19563=CARTESIAN_POINT('Ctrl Pts',(-0.898515013775821,3.09582530028794,
29.6768066825273));
#19564=CARTESIAN_POINT('Ctrl Pts',(-0.828043247235926,3.11541486172981,
29.6720552170986));
#19565=CARTESIAN_POINT('Ctrl Pts',(-0.745303572827527,3.13540810105431,
29.6666686595058));
#19566=CARTESIAN_POINT('Ctrl Pts',(-0.733630998414152,3.13815980225944,
29.6659131543855));
#19567=CARTESIAN_POINT('Ctrl Pts',(-0.714897712427233,3.14246576491344,
29.6647080025157));
#19568=CARTESIAN_POINT('Ctrl Pts',(-0.707846789998971,3.14406150499464,
29.6642560673893));
#19569=CARTESIAN_POINT('Ctrl Pts',(-0.695314062728149,3.14685357083816,
29.663455800664));
#19570=CARTESIAN_POINT('Ctrl Pts',(-0.689834436398883,3.14805932192016,
29.6631069332413));
#19571=CARTESIAN_POINT('Ctrl Pts',(-0.678166418906133,3.15059485388289,
29.6623662840839));
#19572=CARTESIAN_POINT('Ctrl Pts',(-0.671977264520974,3.1519207132548,29.6619747284339));
#19573=CARTESIAN_POINT('Ctrl Pts',(-0.655151028549342,3.15547346634429,
29.660913684378));
#19574=CARTESIAN_POINT('Ctrl Pts',(-0.644506410036485,3.15766482741931,
29.6602462029593));
#19575=CARTESIAN_POINT('Ctrl Pts',(-0.590978076600973,3.16840251597339,
29.6569075785604));
#19576=CARTESIAN_POINT('Ctrl Pts',(-0.547932345980393,3.17612974757747,
29.6542804549792));
#19577=CARTESIAN_POINT('Ctrl Pts',(-0.420990496588037,3.19625952686892,
29.6466667092065));
#19578=CARTESIAN_POINT('Ctrl Pts',(-0.336742964529679,3.20623052794022,
29.6417836779992));
#19579=CARTESIAN_POINT('Ctrl Pts',(-0.000406068110473529,3.23263136135832,
29.6226259748287));
#19580=CARTESIAN_POINT('Ctrl Pts',(0.252827473807959,3.22272999536765,29.6088767928467));
#19581=CARTESIAN_POINT('Ctrl Pts',(0.551060381577973,3.1756708729986,29.5914456505624));
#19582=CARTESIAN_POINT('Ctrl Pts',(0.599622859111373,3.16686045339623,29.5885701662931));
#19583=CARTESIAN_POINT('Ctrl Pts',(0.658405049910383,3.15479539712077,29.5850345670279));
#19584=CARTESIAN_POINT('Ctrl Pts',(0.66883700636404,3.15260023831344,29.5844049980047));
#19585=CARTESIAN_POINT('Ctrl Pts',(0.726216945248131,3.14022836569188,29.5809300848203));
#19586=CARTESIAN_POINT('Ctrl Pts',(0.772941837253632,3.12905509538947,29.5780558895651));
#19587=CARTESIAN_POINT('Ctrl Pts',(0.83564318239307,3.11257131438671,29.5741312797917));
#19588=CARTESIAN_POINT('Ctrl Pts',(0.851854700707565,3.10817362251126,29.5731104163109));
#19589=CARTESIAN_POINT('Ctrl Pts',(0.878401343913244,3.10074903867069,29.5714283234233));
#19590=CARTESIAN_POINT('Ctrl Pts',(0.888757120313623,3.09779668449126,29.5707695307421));
#19591=CARTESIAN_POINT('Ctrl Pts',(0.908811495637516,3.09197049588435,29.5694885964141));
#19592=CARTESIAN_POINT('Ctrl Pts',(0.918511754298188,3.08910278811082,29.5688666618729));
#19593=CARTESIAN_POINT('Ctrl Pts',(0.941158191586101,3.08229167561428,29.5674091057734));
#19594=CARTESIAN_POINT('Ctrl Pts',(0.954093276208391,3.07831231788811,29.5665723115074));
#19595=CARTESIAN_POINT('Ctrl Pts',(0.991525026363504,3.06653819863982,29.5641381735354));
#19596=CARTESIAN_POINT('Ctrl Pts',(1.01595353181547,3.05853179825947,29.5625338882188));
#19597=CARTESIAN_POINT('Ctrl Pts',(1.07397794084757,3.03874256004082,29.5586847772657));
#19598=CARTESIAN_POINT('Ctrl Pts',(1.10747893281186,3.02669377612345,29.5564313496067));
#19599=CARTESIAN_POINT('Ctrl Pts',(1.22145268042145,2.98355704726474,29.5486562195386));
#19600=CARTESIAN_POINT('Ctrl Pts',(1.3008680387229,2.94979652479162,29.5430496902575));
#19601=CARTESIAN_POINT('Ctrl Pts',(1.5692307863845,2.82276608566618,29.523462784395));
#19602=CARTESIAN_POINT('Ctrl Pts',(1.75032820285449,2.71419076092588,29.5090736483039));
#19603=CARTESIAN_POINT('Ctrl Pts',(2.02516560274469,2.51040240796522,29.4860565816094));
#19604=CARTESIAN_POINT('Ctrl Pts',(2.12593312182075,2.42566125694342,29.4773275899195));
#19605=CARTESIAN_POINT('Ctrl Pts',(2.23206697039844,2.32469730196501,29.4680400626352));
#19606=CARTESIAN_POINT('Ctrl Pts',(2.24281378251912,2.31433075926442,29.4670985445374));
#19607=CARTESIAN_POINT('Ctrl Pts',(2.25862280068223,2.29886758863895,29.4657124405473));
#19608=CARTESIAN_POINT('Ctrl Pts',(2.26374045923784,2.29382830251894,29.4652635627232));
#19609=CARTESIAN_POINT('Ctrl Pts',(2.27281277292758,2.28483499045654,29.4644675819881));
#19610=CARTESIAN_POINT('Ctrl Pts',(2.27677401771419,2.2808877456708,29.4641199564936));
#19611=CARTESIAN_POINT('Ctrl Pts',(2.28527049176272,2.2723771105962,29.4633741836911));
#19612=CARTESIAN_POINT('Ctrl Pts',(2.28980232408721,2.26781045759979,29.4629763031123));
#19613=CARTESIAN_POINT('Ctrl Pts',(2.29908552762998,2.25839972951307,29.4621609785315));
#19614=CARTESIAN_POINT('Ctrl Pts',(2.30383534056257,2.2535541544712,29.4617436555735));
#19615=CARTESIAN_POINT('Ctrl Pts',(2.32591364009411,2.23088797274666,29.4598028926061));
#19616=CARTESIAN_POINT('Ctrl Pts',(2.3430514512872,2.21288169405233,29.4582936932344));
#19617=CARTESIAN_POINT('Ctrl Pts',(2.44182459071909,2.10666903662449,29.4495664899157));
#19618=CARTESIAN_POINT('Ctrl Pts',(2.51869134286943,2.01414047870905,29.4426556672));
#19619=CARTESIAN_POINT('Ctrl Pts',(2.65366956281472,1.83181023506072,29.4298260869321));
#19620=CARTESIAN_POINT('Ctrl Pts',(2.7128309768901,1.74299740215409,29.423891139486));
#19621=CARTESIAN_POINT('Ctrl Pts',(2.88400737534978,1.45613556190016,29.4052128235388));
#19622=CARTESIAN_POINT('Ctrl Pts',(2.97952181420673,1.24910348356683,29.3923721342071));
#19623=CARTESIAN_POINT('Ctrl Pts',(3.05949903246884,1.01294912582522,29.3773765367186));
#19624=CARTESIAN_POINT('Ctrl Pts',(3.06633334115026,0.992068579045114,29.3760483795231));
#19625=CARTESIAN_POINT('Ctrl Pts',(3.07690537680614,0.958615073740874,29.3739161844441));
#19626=CARTESIAN_POINT('Ctrl Pts',(3.08078084459804,0.94608611500234,29.3731166817402));
#19627=CARTESIAN_POINT('Ctrl Pts',(3.08750109455554,0.923881089110192,29.3716978934421));
#19628=CARTESIAN_POINT('Ctrl Pts',(3.09037714762243,0.914214612373763,29.3710796433387));
#19629=CARTESIAN_POINT('Ctrl Pts',(3.09625148195943,0.894126347238917,29.369793498447));
#19630=CARTESIAN_POINT('Ctrl Pts',(3.09924262354071,0.883702619770213,29.3691253789827));
#19631=CARTESIAN_POINT('Ctrl Pts',(3.10682642850287,0.856761931016188,29.3673965754224));
#19632=CARTESIAN_POINT('Ctrl Pts',(3.11133996447568,0.84022322654944,29.3663333272389));
#19633=CARTESIAN_POINT('Ctrl Pts',(3.12082918296896,0.804327183420667,29.3640211458183));
#19634=CARTESIAN_POINT('Ctrl Pts',(3.12575715484874,0.78495807983831,29.3627707123131));
#19635=CARTESIAN_POINT('Ctrl Pts',(3.13961206620811,0.728301870177439,29.3591044824234));
#19636=CARTESIAN_POINT('Ctrl Pts',(3.14805391131739,0.690900795586383,29.3566733796703));
#19637=CARTESIAN_POINT('Ctrl Pts',(3.20053145333622,0.4374261572385,29.340120566228));
#19638=CARTESIAN_POINT('Ctrl Pts',(3.22294799654118,0.217515291900805,29.3253254145322));
#19639=CARTESIAN_POINT('Ctrl Pts',(3.22274868255297,-0.00291403553407739,
29.310403850828));
#19640=CARTESIAN_POINT('Ctrl Pts',(3.22274868160926,-0.00291507903117872,
29.3104037801903));
#19641=CARTESIAN_POINT('Ctrl Pts',(3.22256534304824,-0.205603959681518,
29.2966831237793));
#19642=CARTESIAN_POINT('Ctrl Pts',(3.20326082911173,-0.407852858796435,
29.2829337678001));
#19643=CARTESIAN_POINT('Ctrl Pts',(3.16309348166168,-0.617307007073877,
29.2694106703809));
#19644=CARTESIAN_POINT('Ctrl Pts',(3.16106077110211,-0.627632952541531,
29.2687459302496));
#19645=CARTESIAN_POINT('Ctrl Pts',(3.1576273091046,-0.644634672970911,29.2676548391535));
#19646=CARTESIAN_POINT('Ctrl Pts',(3.1562558987221,-0.651316197072443,29.2672269192357));
#19647=CARTESIAN_POINT('Ctrl Pts',(3.15354462065916,-0.664315889376073,
29.2663961111621));
#19648=CARTESIAN_POINT('Ctrl Pts',(3.15220695277181,-0.670634478685622,
29.2659931025164));
#19649=CARTESIAN_POINT('Ctrl Pts',(3.14967635126913,-0.682413129140914,
29.2652434127691));
#19650=CARTESIAN_POINT('Ctrl Pts',(3.14848822261914,-0.687874050417935,
29.2648964719155));
#19651=CARTESIAN_POINT('Ctrl Pts',(3.14574871482761,-0.700309671938866,
29.2641078428984));
#19652=CARTESIAN_POINT('Ctrl Pts',(3.14418834579419,-0.707282307104274,
29.2636666766864));
#19653=CARTESIAN_POINT('Ctrl Pts',(3.13933752253749,-0.728625289511433,
29.2623192395386));
#19654=CARTESIAN_POINT('Ctrl Pts',(3.13597158940063,-0.742978534409029,
29.2614171941518));
#19655=CARTESIAN_POINT('Ctrl Pts',(3.089482932111,-0.935272765366997,29.2493813237167));
#19656=CARTESIAN_POINT('Ctrl Pts',(3.03136414155181,-1.10927518939484,29.2390454697405));
#19657=CARTESIAN_POINT('Ctrl Pts',(2.91544766044806,-1.37776192229644,29.2226713131795));
#19658=CARTESIAN_POINT('Ctrl Pts',(2.86704942961926,-1.4758354527137,29.2165935885301));
#19659=CARTESIAN_POINT('Ctrl Pts',(2.74824608468614,-1.68858484280817,29.2028692994063));
#19660=CARTESIAN_POINT('Ctrl Pts',(2.67546130473401,-1.80168726048934,29.1951934683402));
#19661=CARTESIAN_POINT('Ctrl Pts',(2.56329817344162,-1.95413261530896,29.1840275288447));
#19662=CARTESIAN_POINT('Ctrl Pts',(2.52963819606918,-1.99751391985591,29.1807495327771));
#19663=CARTESIAN_POINT('Ctrl Pts',(2.48400786674977,-2.05331875648277,29.1763874888711));
#19664=CARTESIAN_POINT('Ctrl Pts',(2.47302154446911,-2.06653754395756,29.1753431765623));
#19665=CARTESIAN_POINT('Ctrl Pts',(2.45492580917966,-2.08795944629466,29.1736323330609));
#19666=CARTESIAN_POINT('Ctrl Pts',(2.44787967264201,-2.09621575264933,29.1729684053765));
#19667=CARTESIAN_POINT('Ctrl Pts',(2.43420871949357,-2.11207175866517,29.171684464469));
#19668=CARTESIAN_POINT('Ctrl Pts',(2.42758967739156,-2.11967628621569,29.1710646954275));
#19669=CARTESIAN_POINT('Ctrl Pts',(2.41229345480022,-2.13708428721178,29.1696366577884));
#19670=CARTESIAN_POINT('Ctrl Pts',(2.40359204442231,-2.14686614361002,29.1688273780311));
#19671=CARTESIAN_POINT('Ctrl Pts',(2.38018131644951,-2.17286303055339,29.1666580443978));
#19672=CARTESIAN_POINT('Ctrl Pts',(2.36536616874142,-2.18898142940791,29.1652935181092));
#19673=CARTESIAN_POINT('Ctrl Pts',(2.23881732764216,-2.32387758097412,29.1537054128931));
#19674=CARTESIAN_POINT('Ctrl Pts',(2.11839832906726,-2.43414955835226,29.1430984663776));
#19675=CARTESIAN_POINT('Ctrl Pts',(1.79146236147033,-2.69083719126962,29.1153810232071));
#19676=CARTESIAN_POINT('Ctrl Pts',(1.57511053416741,-2.82293531037656,29.0979463293549));
#19677=CARTESIAN_POINT('Ctrl Pts',(1.29266224771272,-2.95271579735184,29.0775892870927));
#19678=CARTESIAN_POINT('Ctrl Pts',(1.23911345335635,-2.97558483673494,29.073832022879));
#19679=CARTESIAN_POINT('Ctrl Pts',(1.17406089214567,-3.0013057517665,29.0694136140893));
#19680=CARTESIAN_POINT('Ctrl Pts',(1.16312739045241,-3.0055598276544,29.0686758897867));
#19681=CARTESIAN_POINT('Ctrl Pts',(1.14603338497877,-3.01210362198886,29.0675303734807));
#19682=CARTESIAN_POINT('Ctrl Pts',(1.13988882690843,-3.0144343106465,29.0671201912356));
#19683=CARTESIAN_POINT('Ctrl Pts',(1.12851637022563,-3.01870824532816,29.0663639965173));
#19684=CARTESIAN_POINT('Ctrl Pts',(1.12329059885219,-3.02065670006162,29.0660176815883));
#19685=CARTESIAN_POINT('Ctrl Pts',(1.11150250143589,-3.02501712908773,29.0652390816793));
#19686=CARTESIAN_POINT('Ctrl Pts',(1.10493738799372,-3.02742131404998,29.0648072652107));
#19687=CARTESIAN_POINT('Ctrl Pts',(1.08564142753255,-3.034416484567,29.0635432391056));
#19688=CARTESIAN_POINT('Ctrl Pts',(1.07288923917483,-3.03894873375401,29.0627144483772));
#19689=CARTESIAN_POINT('Ctrl Pts',(0.983152201627766,-3.07020686216032,
29.0569257809611));
#19690=CARTESIAN_POINT('Ctrl Pts',(0.905199431957328,-3.09408708161769,
29.0521213336498));
#19691=CARTESIAN_POINT('Ctrl Pts',(0.577940644502667,-3.18091009518054,
29.0325512088994));
#19692=CARTESIAN_POINT('Ctrl Pts',(0.322457362576845,-3.21686866800029,
29.0186238319458));
#19693=CARTESIAN_POINT('Ctrl Pts',(-0.0244965292561324,-3.22391103655472,
28.9988486067735));
#19694=CARTESIAN_POINT('Ctrl Pts',(-0.114425116185241,-3.22197261273145,
28.9936538743263));
#19695=CARTESIAN_POINT('Ctrl Pts',(-0.259056058253541,-3.21279228997703,
28.9851042261706));
#19696=CARTESIAN_POINT('Ctrl Pts',(-0.313860790535886,-3.20790199344572,
28.9818194808435));
#19697=CARTESIAN_POINT('Ctrl Pts',(-0.385575746276679,-3.19964747495353,
28.9774511558123));
#19698=CARTESIAN_POINT('Ctrl Pts',(-0.402624079715029,-3.19754694301061,
28.9764075028551));
#19699=CARTESIAN_POINT('Ctrl Pts',(-0.430414018425829,-3.1938971646164,
28.9746974683103));
#19700=CARTESIAN_POINT('Ctrl Pts',(-0.44116617140963,-3.19242975334629,
28.9740336854851));
#19701=CARTESIAN_POINT('Ctrl Pts',(-0.46189358693377,-3.18949424450099,
28.9727498342086));
#19702=CARTESIAN_POINT('Ctrl Pts',(-0.471869787077632,-3.18803358227474,
28.9721300089135));
#19703=CARTESIAN_POINT('Ctrl Pts',(-0.494789209224281,-3.1845679058044,
28.9707015685828));
#19704=CARTESIAN_POINT('Ctrl Pts',(-0.507727324821025,-3.18253076398856,
28.9698919405207));
#19705=CARTESIAN_POINT('Ctrl Pts',(-0.542276322214073,-3.17687489103105,
28.9677210657206));
#19706=CARTESIAN_POINT('Ctrl Pts',(-0.563863023052856,-3.17311457968817,
28.9663553365741));
#19707=CARTESIAN_POINT('Ctrl Pts',(-0.746702636286027,-3.13934005677025,
28.9547063258453));
#19708=CARTESIAN_POINT('Ctrl Pts',(-0.905460592489548,-3.09728061484943,
28.9440350000521));
#19709=CARTESIAN_POINT('Ctrl Pts',(-1.20274089852636,-2.99370695645388,
28.9230375612164));
#19710=CARTESIAN_POINT('Ctrl Pts',(-1.3413890507256,-2.9341887838544,28.9127897747778));
#19711=CARTESIAN_POINT('Ctrl Pts',(-1.4752555406476,-2.86526415052584,28.9026236394039));
#19712=CARTESIAN_POINT('Ctrl Pts',(-1.47525540425972,-2.86526422074867,
28.6587956971472));
#19713=CARTESIAN_POINT('Ctrl Pts',(-1.40396999219795,-2.90196735919833,
28.6641728647368));
#19714=CARTESIAN_POINT('Ctrl Pts',(-1.3313329276085,-2.93600090125158,28.6694959185801));
#19715=CARTESIAN_POINT('Ctrl Pts',(-1.21664140494405,-2.98460551359186,
28.6775868870742));
#19716=CARTESIAN_POINT('Ctrl Pts',(-1.17543153260819,-3.00107440122143,
28.6804330269589));
#19717=CARTESIAN_POINT('Ctrl Pts',(-1.1237423023483,-3.02050300089093,28.6839161440751));
#19718=CARTESIAN_POINT('Ctrl Pts',(-1.11357292367107,-3.02426693465933,
28.6845972822034));
#19719=CARTESIAN_POINT('Ctrl Pts',(-1.09744394476884,-3.03014427507075,
28.6856708397806));
#19720=CARTESIAN_POINT('Ctrl Pts',(-1.0914968996138,-3.03229155250976,28.6860652327261));
#19721=CARTESIAN_POINT('Ctrl Pts',(-1.08026160193583,-3.03631090353643,
28.6868075487327));
#19722=CARTESIAN_POINT('Ctrl Pts',(-1.07497484724119,-3.03818664828513,
28.6871556795278));
#19723=CARTESIAN_POINT('Ctrl Pts',(-1.06285910381106,-3.04244973997234,
28.6879508676203));
#19724=CARTESIAN_POINT('Ctrl Pts',(-1.05602696245719,-3.0448279018325,28.6883973759602));
#19725=CARTESIAN_POINT('Ctrl Pts',(-1.03782773461022,-3.05109414481469,
28.6895818573481));
#19726=CARTESIAN_POINT('Ctrl Pts',(-1.02644669036383,-3.05494174896131,
28.6903174972633));
#19727=CARTESIAN_POINT('Ctrl Pts',(-0.945255347244536,-3.08188525732524,
28.6955311188072));
#19728=CARTESIAN_POINT('Ctrl Pts',(-0.874688204289027,-3.10265157735439,
28.6998821778984));
#19729=CARTESIAN_POINT('Ctrl Pts',(-0.577957695183423,-3.17904185304228,
28.7176707123769));
#19730=CARTESIAN_POINT('Ctrl Pts',(-0.346806425840722,-3.21248883264467,
28.73036260275));
#19731=CARTESIAN_POINT('Ctrl Pts',(0.0525160222780035,-3.22662981942941,
28.7529268929991));
#19732=CARTESIAN_POINT('Ctrl Pts',(0.219270651318447,-3.21959738789219,
28.7625308840943));
#19733=CARTESIAN_POINT('Ctrl Pts',(0.407795520838591,-3.19692985981318,
28.7739614183635));
#19734=CARTESIAN_POINT('Ctrl Pts',(0.430839345416441,-3.19390593636074,
28.7753680890368));
#19735=CARTESIAN_POINT('Ctrl Pts',(0.465894098769699,-3.18891961264384,
28.7775232068439));
#19736=CARTESIAN_POINT('Ctrl Pts',(0.477930270913111,-3.18713794130816,
28.7782659223024));
#19737=CARTESIAN_POINT('Ctrl Pts',(0.499792445413534,-3.18377513656193,
28.7796200863225));
#19738=CARTESIAN_POINT('Ctrl Pts',(0.509621803679512,-3.18221655805529,
28.7802308105047));
#19739=CARTESIAN_POINT('Ctrl Pts',(0.53080882967596,-3.17875638578577,28.7815513521264));
#19740=CARTESIAN_POINT('Ctrl Pts',(0.542163810837095,-3.17683939955025,
28.7822616524814));
#19741=CARTESIAN_POINT('Ctrl Pts',(0.572886769222668,-3.17148313205629,
28.7841905795537));
#19742=CARTESIAN_POINT('Ctrl Pts',(0.592233686408896,-3.16792735716365,
28.785412906091));
#19743=CARTESIAN_POINT('Ctrl Pts',(0.685927946182076,-3.14981899119338,
28.7913704394246));
#19744=CARTESIAN_POINT('Ctrl Pts',(0.759773804354028,-3.13282604629927,
28.7961830864327));
#19745=CARTESIAN_POINT('Ctrl Pts',(0.87699065171407,-3.10146474954353,28.8040170238609));
#19746=CARTESIAN_POINT('Ctrl Pts',(0.920776848315933,-3.08874827181873,
28.8069876221633));
#19747=CARTESIAN_POINT('Ctrl Pts',(1.17616572146954,-3.00866469720912,28.8245690270011));
#19748=CARTESIAN_POINT('Ctrl Pts',(1.38060677875684,-2.9205027506252,28.8397379188287));
#19749=CARTESIAN_POINT('Ctrl Pts',(1.65535713550674,-2.76668259807285,28.8609260244795));
#19750=CARTESIAN_POINT('Ctrl Pts',(1.73438754721218,-2.71783776856526,28.8671163102619));
#19751=CARTESIAN_POINT('Ctrl Pts',(1.8496900150307,-2.63949417640251,28.8761832508512));
#19752=CARTESIAN_POINT('Ctrl Pts',(1.88760861915842,-2.61251160702068,28.8791708839483));
#19753=CARTESIAN_POINT('Ctrl Pts',(1.93376225015725,-2.57813931891385,28.882801609748));
#19754=CARTESIAN_POINT('Ctrl Pts',(1.94255909407012,-2.57151763793293,28.8834933558206));
#19755=CARTESIAN_POINT('Ctrl Pts',(1.95638340748184,-2.56100018965169,28.884579788304));
#19756=CARTESIAN_POINT('Ctrl Pts',(1.9614334787735,-2.55713447406964,28.8849765274964));
#19757=CARTESIAN_POINT('Ctrl Pts',(1.97091051274624,-2.54983542562625,28.8857207396868));
#19758=CARTESIAN_POINT('Ctrl Pts',(1.97533991252699,-2.54640554066325,28.8860684349561));
#19759=CARTESIAN_POINT('Ctrl Pts',(1.98542017193474,-2.53855780921815,28.8868594280023));
#19760=CARTESIAN_POINT('Ctrl Pts',(1.99106523364058,-2.53413264206891,28.8873021976337));
#19761=CARTESIAN_POINT('Ctrl Pts',(2.00596194063047,-2.52237459872266,28.8884702405812));
#19762=CARTESIAN_POINT('Ctrl Pts',(2.01518825011847,-2.51500959243648,28.8891932824551));
#19763=CARTESIAN_POINT('Ctrl Pts',(2.07834517174276,-2.46402317407827,28.8941416757975));
#19764=CARTESIAN_POINT('Ctrl Pts',(2.13090008533058,-2.41871768971775,28.8982541898969));
#19765=CARTESIAN_POINT('Ctrl Pts',(2.20228957414053,-2.35304092544874,28.9038996444825));
#19766=CARTESIAN_POINT('Ctrl Pts',(2.22238244325534,-2.33407311599751,28.9054954685767));
#19767=CARTESIAN_POINT('Ctrl Pts',(2.41885297919624,-2.14376608856944,28.9211975881544));
#19768=CARTESIAN_POINT('Ctrl Pts',(2.57532111485968,-1.95302748641564,28.9345590400097));
#19769=CARTESIAN_POINT('Ctrl Pts',(2.75612272864558,-1.67260349494436,28.9535927331154));
#19770=CARTESIAN_POINT('Ctrl Pts',(2.80063040280429,-1.59696041740749,28.9586666214574));
#19771=CARTESIAN_POINT('Ctrl Pts',(2.86757268797092,-1.47176323342458,28.9670465993361));
#19772=CARTESIAN_POINT('Ctrl Pts',(2.89193758341982,-1.42329077376705,28.970286610484));
#19773=CARTESIAN_POINT('Ctrl Pts',(2.92230106935959,-1.35888257761859,28.9745963909198));
#19774=CARTESIAN_POINT('Ctrl Pts',(2.92941412101072,-1.34347991805939,28.9756273554906));
#19775=CARTESIAN_POINT('Ctrl Pts',(2.94085673881402,-1.31817901150173,28.977321676591));
#19776=CARTESIAN_POINT('Ctrl Pts',(2.94525879437391,-1.30831375986799,28.9779825242725));
#19777=CARTESIAN_POINT('Ctrl Pts',(2.95367877681639,-1.28918624599409,28.9792643020775));
#19778=CARTESIAN_POINT('Ctrl Pts',(2.95770294795101,-1.27992685785367,28.9798850085528));
#19779=CARTESIAN_POINT('Ctrl Pts',(2.96688777363738,-1.25851846646698,28.9813206935619));
#19780=CARTESIAN_POINT('Ctrl Pts',(2.97201740303294,-1.24635642555943,28.982136720303));
#19781=CARTESIAN_POINT('Ctrl Pts',(2.98560068114123,-1.21359058612412,28.9843364721306));
#19782=CARTESIAN_POINT('Ctrl Pts',(2.99391559255992,-1.19293039292791,28.9857248708156));
#19783=CARTESIAN_POINT('Ctrl Pts',(3.07649546443753,-0.981440032530335,
28.9999536340679));
#19784=CARTESIAN_POINT('Ctrl Pts',(3.1326127666368,-0.784065332646564,29.013413091123));
#19785=CARTESIAN_POINT('Ctrl Pts',(3.20505859250885,-0.390016707707387,
29.0403759663423));
#19786=CARTESIAN_POINT('Ctrl Pts',(3.22284016615892,-0.194467152849475,
29.0537891193601));
#19787=CARTESIAN_POINT('Ctrl Pts',(3.22271722593296,0.0717007493025189,
29.0713365201397));
#19788=CARTESIAN_POINT('Ctrl Pts',(3.22039028229918,0.14189930542022,29.0758939041521));
#19789=CARTESIAN_POINT('Ctrl Pts',(3.21499221206757,0.223792271955602,29.0810864052186));
#19790=CARTESIAN_POINT('Ctrl Pts',(3.21414783218013,0.235609056908833,29.0818326238974));
#19791=CARTESIAN_POINT('Ctrl Pts',(3.21268668472616,0.254584861328354,29.0830257592115));
#19792=CARTESIAN_POINT('Ctrl Pts',(3.21211111186224,0.26174681135929,29.0834748948519));
#19793=CARTESIAN_POINT('Ctrl Pts',(3.21104402255572,0.274490888215193,29.0842719132135));
#19794=CARTESIAN_POINT('Ctrl Pts',(3.21056189399288,0.280073720927902,29.0846203170239));
#19795=CARTESIAN_POINT('Ctrl Pts',(3.20950215639828,0.291982569170837,29.0853618883162));
#19796=CARTESIAN_POINT('Ctrl Pts',(3.20892040648182,0.298308127845474,29.0857548199946));
#19797=CARTESIAN_POINT('Ctrl Pts',(3.20728242496246,0.315559004206297,29.0868238798402));
#19798=CARTESIAN_POINT('Ctrl Pts',(3.20618906392951,0.326480831086335,29.087497948285));
#19799=CARTESIAN_POINT('Ctrl Pts',(3.20021562258018,0.383224416561684,29.0909865984107));
#19800=CARTESIAN_POINT('Ctrl Pts',(3.19440870488997,0.428945824171261,29.0937520649199));
#19801=CARTESIAN_POINT('Ctrl Pts',(3.17415335876158,0.565009832966689,29.1018875723163));
#19802=CARTESIAN_POINT('Ctrl Pts',(3.15683655997082,0.654882479877528,29.1071368810512));
#19803=CARTESIAN_POINT('Ctrl Pts',(3.08056946531086,0.976365585140953,29.1258427994704));
#19804=CARTESIAN_POINT('Ctrl Pts',(2.99974492977684,1.20196942756836,29.1388913276044));
#19805=CARTESIAN_POINT('Ctrl Pts',(2.88188213627333,1.44281906994326,29.1543467970422));
#19806=CARTESIAN_POINT('Ctrl Pts',(2.868681135622,1.4688907353864,29.1560402125599));
#19807=CARTESIAN_POINT('Ctrl Pts',(2.81941619220345,1.56299007899431,29.1622331727083));
#19808=CARTESIAN_POINT('Ctrl Pts',(2.78127419751381,1.62989510969802,29.1667929441243));
#19809=CARTESIAN_POINT('Ctrl Pts',(2.73037025714497,1.71218779377524,29.1726333473387));
#19810=CARTESIAN_POINT('Ctrl Pts',(2.71981067782974,1.72891255766319,29.1738327135409));
#19811=CARTESIAN_POINT('Ctrl Pts',(2.70284721757682,1.7552400599415,29.1757409309371));
#19812=CARTESIAN_POINT('Ctrl Pts',(2.69654444135584,1.76490759529053,29.176446006175));
#19813=CARTESIAN_POINT('Ctrl Pts',(2.68471085993894,1.78284721020861,29.1777626527426));
#19814=CARTESIAN_POINT('Ctrl Pts',(2.67919339063614,1.79112795423892,29.1783737165681));
#19815=CARTESIAN_POINT('Ctrl Pts',(2.66686158549637,1.80945133527866,29.1797333053164));
#19816=CARTESIAN_POINT('Ctrl Pts',(2.66002871843932,1.81948126166461,29.1804825279099));
#19817=CARTESIAN_POINT('Ctrl Pts',(2.64003061574145,1.84848293416519,29.1826636448888));
#19818=CARTESIAN_POINT('Ctrl Pts',(2.62671813177074,1.86735176690557,29.1841011542546));
#19819=CARTESIAN_POINT('Ctrl Pts',(2.51911292595528,2.01644144190624,29.1956096258624));
#19820=CARTESIAN_POINT('Ctrl Pts',(2.41541305500278,2.1395634685583,29.2060523943513));
#19821=CARTESIAN_POINT('Ctrl Pts',(2.13030543509723,2.43081155771247,29.2331990204489));
#19822=CARTESIAN_POINT('Ctrl Pts',(1.93795346992231,2.5867692885241,29.250216023592));
#19823=CARTESIAN_POINT('Ctrl Pts',(1.67364821176006,2.75489222714048,29.2708290805123));
#19824=CARTESIAN_POINT('Ctrl Pts',(1.61650972287745,2.78880391382018,29.2751338136682));
#19825=CARTESIAN_POINT('Ctrl Pts',(1.54815548818489,2.82656470714442,29.2800732326752));
#19826=CARTESIAN_POINT('Ctrl Pts',(1.53792080739249,2.83214636965665,29.2808073920191));
#19827=CARTESIAN_POINT('Ctrl Pts',(1.52131124925244,2.84108809547771,29.2819898148161));
#19828=CARTESIAN_POINT('Ctrl Pts',(1.51495510381144,2.84448246948307,29.2824401803591));
#19829=CARTESIAN_POINT('Ctrl Pts',(1.50364543539903,2.85047351249694,29.2832376898377));
#19830=CARTESIAN_POINT('Ctrl Pts',(1.49869649159102,2.85307862994574,29.2835853651635));
#19831=CARTESIAN_POINT('Ctrl Pts',(1.48805705073403,2.85864389500602,29.2843300030355));
#19832=CARTESIAN_POINT('Ctrl Pts',(1.48236450612242,2.86159993314565,29.2847267055979));
#19833=CARTESIAN_POINT('Ctrl Pts',(1.46665712192126,2.86969705278641,29.2858167246806));
#19834=CARTESIAN_POINT('Ctrl Pts',(1.4566239983704,2.87480274526202,29.2865078434825));
#19835=CARTESIAN_POINT('Ctrl Pts',(1.40193496656332,2.90227328450517,29.290248312243));
#19836=CARTESIAN_POINT('Ctrl Pts',(1.35678781225537,2.92365171319271,29.2932397205461));
#19837=CARTESIAN_POINT('Ctrl Pts',(1.07460349449837,3.04932830812556,29.3114576644985));
#19838=CARTESIAN_POINT('Ctrl Pts',(0.826187780816833,3.12579918209925,29.3254990040934));
#19839=CARTESIAN_POINT('Ctrl Pts',(0.407963346515534,3.20112777082683,29.349490132611));
#19840=CARTESIAN_POINT('Ctrl Pts',(0.242646346792784,3.21788208299025,29.359046072379));
#19841=CARTESIAN_POINT('Ctrl Pts',(0.0548488916515991,3.22235794675189,
29.370344360395));
#19842=CARTESIAN_POINT('Ctrl Pts',(0.032905956164449,3.22265671449435,29.3716709932229));
#19843=CARTESIAN_POINT('Ctrl Pts',(-0.00214273177335041,3.22277593224936,
29.37380106105));
#19844=CARTESIAN_POINT('Ctrl Pts',(-0.0152475465529373,3.22274057366517,
29.3745999734712));
#19845=CARTESIAN_POINT('Ctrl Pts',(-0.0384321778173136,3.22253660266174,
29.3760179046385));
#19846=CARTESIAN_POINT('Ctrl Pts',(-0.0485121605683872,3.22240061978577,
29.3766358903689));
#19847=CARTESIAN_POINT('Ctrl Pts',(-0.069432302913408,3.22202021798673,
29.3779216740557));
#19848=CARTESIAN_POINT('Ctrl Pts',(-0.0802721848751933,3.22176838111275,
29.3785896974758));
#19849=CARTESIAN_POINT('Ctrl Pts',(-0.108251176547647,3.22097706971161,
29.3803186552264));
#19850=CARTESIAN_POINT('Ctrl Pts',(-0.125387452674089,3.22035550354695,
29.38138215616));
#19851=CARTESIAN_POINT('Ctrl Pts',(-0.198333773731072,3.2171264843759,29.3859292906803));
#19852=CARTESIAN_POINT('Ctrl Pts',(-0.254073125289005,3.21320483610382,
29.3894539024931));
#19853=CARTESIAN_POINT('Ctrl Pts',(-0.400671620884013,3.19905243871314,
29.3988621017981));
#19854=CARTESIAN_POINT('Ctrl Pts',(-0.49124109159605,3.18640141235104,29.4048164260533));
#19855=CARTESIAN_POINT('Ctrl Pts',(-0.824309834902664,3.12533962759615,
29.4272117624473));
#19856=CARTESIAN_POINT('Ctrl Pts',(-1.06151258024309,3.05293462985347,29.4442280392737));
#19857=CARTESIAN_POINT('Ctrl Pts',(-1.36931872167645,2.91872148500965,29.4665401409083));
#19858=CARTESIAN_POINT('Ctrl Pts',(-1.44905421151699,2.87996768340037,29.472332954282));
#19859=CARTESIAN_POINT('Ctrl Pts',(-1.53925768142025,2.83142967827752,29.478820287786));
#19860=CARTESIAN_POINT('Ctrl Pts',(-1.5513754705336,2.82480838258828,29.4796903505045));
#19861=CARTESIAN_POINT('Ctrl Pts',(-1.5696146349845,2.81468953000495,29.480997324202));
#19862=CARTESIAN_POINT('Ctrl Pts',(-1.57576752290986,2.81124953866858,29.481437773699));
#19863=CARTESIAN_POINT('Ctrl Pts',(-1.58676994787959,2.80505076999256,29.4822244946813));
#19864=CARTESIAN_POINT('Ctrl Pts',(-1.59162363381234,2.80229957348605,29.4825712422186));
#19865=CARTESIAN_POINT('Ctrl Pts',(-1.60213656782863,2.79630444133275,29.4833216007648));
#19866=CARTESIAN_POINT('Ctrl Pts',(-1.60779310213573,2.79305593447331,29.4837249105969));
#19867=CARTESIAN_POINT('Ctrl Pts',(-1.62361447085714,2.78390584659214,29.4848518927007));
#19868=CARTESIAN_POINT('Ctrl Pts',(-1.63375706294691,2.77796572726383,29.4855731142718));
#19869=CARTESIAN_POINT('Ctrl Pts',(-1.69350980301012,2.74253043790169,29.489815984749));
#19870=CARTESIAN_POINT('Ctrl Pts',(-1.74235631050502,2.71176033250252,29.4932597525121));
#19871=CARTESIAN_POINT('Ctrl Pts',(-2.00065102691814,2.53918874729656,29.5114830729581));
#19872=CARTESIAN_POINT('Ctrl Pts',(-2.19369724152766,2.37440579334918,29.5252106547641));
#19873=CARTESIAN_POINT('Ctrl Pts',(-2.47646698755928,2.06879805338074,29.548731441992));
#19874=CARTESIAN_POINT('Ctrl Pts',(-2.57813864954197,1.94061970938887,29.558148215819));
#19875=CARTESIAN_POINT('Ctrl Pts',(-2.68191255561879,1.78716030795524,29.5692907602122));
#19876=CARTESIAN_POINT('Ctrl Pts',(-2.69399176085513,1.76889945404617,29.5706143796169));
#19877=CARTESIAN_POINT('Ctrl Pts',(-2.71299398607165,1.73952652931348,29.5727405214983));
#19878=CARTESIAN_POINT('Ctrl Pts',(-2.72003711778324,1.72849269150688,29.5735385479879));
#19879=CARTESIAN_POINT('Ctrl Pts',(-2.73238369020971,1.70888809189005,29.5749554536819));
#19880=CARTESIAN_POINT('Ctrl Pts',(-2.73771454344464,1.70033473647812,29.5755733048334));
#19881=CARTESIAN_POINT('Ctrl Pts',(-2.74870036211992,1.68252238851788,29.5768593539146));
#19882=CARTESIAN_POINT('Ctrl Pts',(-2.75434886209182,1.67325957635592,29.577527780018));
#19883=CARTESIAN_POINT('Ctrl Pts',(-2.76881903952392,1.64925853776594,29.5792589521897));
#19884=CARTESIAN_POINT('Ctrl Pts',(-2.77756976598455,1.63447813527753,29.5803242773644));
#19885=CARTESIAN_POINT('Ctrl Pts',(-2.81441290685011,1.5710979148245,29.5848897864165));
#19886=CARTESIAN_POINT('Ctrl Pts',(-2.84134968918131,1.52184098136778,29.5884313616665));
#19887=CARTESIAN_POINT('Ctrl Pts',(-2.90901258580667,1.39004707684882,29.5978963495169));
#19888=CARTESIAN_POINT('Ctrl Pts',(-2.94751120579408,1.30643035158349,29.6038915654883));
#19889=CARTESIAN_POINT('Ctrl Pts',(-3.07400896998979,0.99752342459847,29.625974800896));
#19890=CARTESIAN_POINT('Ctrl Pts',(-3.14015841323614,0.764182201518884,
29.6426030850781));
#19891=CARTESIAN_POINT('Ctrl Pts',(-3.19473614475354,0.434049400776789,
29.6648717052604));
#19892=CARTESIAN_POINT('Ctrl Pts',(-3.20591589905586,0.341825482980683,
29.6709511967882));
#19893=CARTESIAN_POINT('Ctrl Pts',(-3.2141770306316,0.235325972411949,29.6777174937204));
#19894=CARTESIAN_POINT('Ctrl Pts',(-3.21516589940946,0.221405856701903,
29.6785968949952));
#19895=CARTESIAN_POINT('Ctrl Pts',(-3.21652017215728,0.200413763289398,
29.6799150992434));
#19896=CARTESIAN_POINT('Ctrl Pts',(-3.21695272392094,0.193346499172079,
29.6803575298326));
#19897=CARTESIAN_POINT('Ctrl Pts',(-3.21768460241923,0.180705603581696,
29.6811463839373));
#19898=CARTESIAN_POINT('Ctrl Pts',(-3.21799274311681,0.175132585882723,
29.6814932945891));
#19899=CARTESIAN_POINT('Ctrl Pts',(-3.21862838948232,0.163067781524378,
29.682242408471));
#19900=CARTESIAN_POINT('Ctrl Pts',(-3.21895073380752,0.156575815615226,
29.6826443191391));
#19901=CARTESIAN_POINT('Ctrl Pts',(-3.21979588877823,0.138447375079245,
29.6837634450653));
#19902=CARTESIAN_POINT('Ctrl Pts',(-3.22027526303739,0.126808836387373,
29.6844782644303));
#19903=CARTESIAN_POINT('Ctrl Pts',(-3.22269088586834,0.0592554099718082,
29.6886073424715));
#19904=CARTESIAN_POINT('Ctrl Pts',(-3.22323405306892,0.00329651312935113,
29.6919485097842));
#19905=CARTESIAN_POINT('Ctrl Pts',(-3.21816668937871,-0.306828167702081,
29.7101654024707));
#19906=CARTESIAN_POINT('Ctrl Pts',(-3.18395454746291,-0.559643820509983,
29.723960319426));
#19907=CARTESIAN_POINT('Ctrl Pts',(-3.079361943721,-0.96465228794684,29.7475867180965));
#19908=CARTESIAN_POINT('Ctrl Pts',(-3.026286824543,-1.12008999879813,29.7570385346208));
#19909=CARTESIAN_POINT('Ctrl Pts',(-2.95297955811983,-1.29093346616297,
29.7682202766622));
#19910=CARTESIAN_POINT('Ctrl Pts',(-2.94413621208154,-1.31097651128621,
29.7695446616785));
#19911=CARTESIAN_POINT('Ctrl Pts',(-2.9296818711405,-1.34285261538615,29.7716718010717));
#19912=CARTESIAN_POINT('Ctrl Pts',(-2.92420180454128,-1.35474455566887,
29.7724700527126));
#19913=CARTESIAN_POINT('Ctrl Pts',(-2.91437540815084,-1.37573076338613,
29.7738872189485));
#19914=CARTESIAN_POINT('Ctrl Pts',(-2.9100585735824,-1.38483870815884,29.7745051042296));
#19915=CARTESIAN_POINT('Ctrl Pts',(-2.90100723800875,-1.40370660688985,
29.7757910855052));
#19916=CARTESIAN_POINT('Ctrl Pts',(-2.89626604918457,-1.41346319405193,
29.7764594089833));
#19917=CARTESIAN_POINT('Ctrl Pts',(-2.8838936670672,-1.43859989601201,29.7781900168559));
#19918=CARTESIAN_POINT('Ctrl Pts',(-2.87618873774572,-1.4539431454608,29.7792548771685));
#19919=CARTESIAN_POINT('Ctrl Pts',(-2.84280108237013,-1.51912577303895,
29.7838156968553));
#19920=CARTESIAN_POINT('Ctrl Pts',(-2.81594398727527,-1.56834942905493,
29.7873529419509));
#19921=CARTESIAN_POINT('Ctrl Pts',(-2.74172967717129,-1.69631220044069,
29.7968034217194));
#19922=CARTESIAN_POINT('Ctrl Pts',(-2.69226844888869,-1.77376570788618,
29.8027881863976));
#19923=CARTESIAN_POINT('Ctrl Pts',(-2.49992934405106,-2.04834321412894,
29.8249649056176));
#19924=CARTESIAN_POINT('Ctrl Pts',(-2.33817105111614,-2.23120992218163,
29.8417071376863));
#19925=CARTESIAN_POINT('Ctrl Pts',(-2.08936213317222,-2.45541594605325,
29.8639860290489));
#19926=CARTESIAN_POINT('Ctrl Pts',(-2.01875212402243,-2.51379092722465,
29.8699787600656));
#19927=CARTESIAN_POINT('Ctrl Pts',(-1.93465462152868,-2.57748377393532,
29.8766608143329));
#19928=CARTESIAN_POINT('Ctrl Pts',(-1.92350976937498,-2.58581153471196,
29.8775374961406));
#19929=CARTESIAN_POINT('Ctrl Pts',(-1.90661924858856,-2.5982629979883,29.8788524311));
#19930=CARTESIAN_POINT('Ctrl Pts',(-1.90091353298779,-2.60244026025053,
29.8792942858187));
#19931=CARTESIAN_POINT('Ctrl Pts',(-1.8906802196346,-2.60988065150266,29.8800825186397));
#19932=CARTESIAN_POINT('Ctrl Pts',(-1.8861578684914,-2.61315081935606,29.880429380658));
#19933=CARTESIAN_POINT('Ctrl Pts',(-1.87634459448594,-2.62020817107423,
29.8811788507798));
#19934=CARTESIAN_POINT('Ctrl Pts',(-1.87105070652266,-2.62399107323361,
29.8815811638383));
#19935=CARTESIAN_POINT('Ctrl Pts',(-1.85622298900629,-2.63451896254672,
29.8827025474526));
#19936=CARTESIAN_POINT('Ctrl Pts',(-1.84666378497292,-2.64122827940597,
29.8834192064229));
#19937=CARTESIAN_POINT('Ctrl Pts',(-1.7906882474572,-2.6800633699564,29.8875805671746));
#19938=CARTESIAN_POINT('Ctrl Pts',(-1.74346759721204,-2.71101931098909,
29.8909508350776));
#19939=CARTESIAN_POINT('Ctrl Pts',(-1.62366007748064,-2.78513420718741,
29.8992222652674));
#19940=CARTESIAN_POINT('Ctrl Pts',(-1.5502013178676,-2.82667638698033,29.9040479009646));
#19941=CARTESIAN_POINT('Ctrl Pts',(-1.4752551445451,-2.86526435446945,29.9088139162969));
#19942=CARTESIAN_POINT('Origin',(0.,0.,4.68922655072688));
#19943=CARTESIAN_POINT('',(-1.47525569888183,-2.86526406905484,31.4041249682223));
#19944=CARTESIAN_POINT('',(-1.47525540353836,-2.86526422112008,31.1543403726568));
#19945=CARTESIAN_POINT('',(-1.47525540501186,-2.86526422036142,4.68922655072688));
#19946=CARTESIAN_POINT('Ctrl Pts',(-1.47525569888183,-2.86526406905484,
31.4041249682223));
#19947=CARTESIAN_POINT('Ctrl Pts',(-1.54049706273102,-2.83167285669126,
31.4000144140638));
#19948=CARTESIAN_POINT('Ctrl Pts',(-1.60460828957561,-2.79584454116413,
31.3958833098916));
#19949=CARTESIAN_POINT('Ctrl Pts',(-1.74615649069285,-2.71026000447311,
31.3864664849392));
#19950=CARTESIAN_POINT('Ctrl Pts',(-1.8227617937159,-2.65934377138192,31.3811594019167));
#19951=CARTESIAN_POINT('Ctrl Pts',(-1.94243829536211,-2.57219732526237,
31.3724297982344));
#19952=CARTESIAN_POINT('Ctrl Pts',(-1.98692227495442,-2.5379922986544,31.3690808157502));
#19953=CARTESIAN_POINT('Ctrl Pts',(-2.04382805416653,-2.49182252769639,
31.3646464561045));
#19954=CARTESIAN_POINT('Ctrl Pts',(-2.0570802935324,-2.48089364397653,31.363602795394));
#19955=CARTESIAN_POINT('Ctrl Pts',(-2.07856103402427,-2.46288841685041,
31.3618927513368));
#19956=CARTESIAN_POINT('Ctrl Pts',(-2.08684238861338,-2.45587543791435,
31.3612289668083));
#19957=CARTESIAN_POINT('Ctrl Pts',(-2.10274938745271,-2.44226620881424,
31.3599451144795));
#19958=CARTESIAN_POINT('Ctrl Pts',(-2.11037981649738,-2.43567572709953,
31.3593252898474));
#19959=CARTESIAN_POINT('Ctrl Pts',(-2.12785095248667,-2.42044199073886,
31.3578968542589));
#19960=CARTESIAN_POINT('Ctrl Pts',(-2.13767009626727,-2.41177437956257,
31.357087230298));
#19961=CARTESIAN_POINT('Ctrl Pts',(-2.16377429672397,-2.38844687315969,
31.3549163736471));
#19962=CARTESIAN_POINT('Ctrl Pts',(-2.17996291368153,-2.37368054500649,
31.3535506586662));
#19963=CARTESIAN_POINT('Ctrl Pts',(-2.31603995033572,-2.24699267417088,
31.341902368894));
#19964=CARTESIAN_POINT('Ctrl Pts',(-2.42735533987515,-2.12625220959061,
31.3312318054368));
#19965=CARTESIAN_POINT('Ctrl Pts',(-2.68674547701507,-1.79785815037375,
31.3033194410212));
#19966=CARTESIAN_POINT('Ctrl Pts',(-2.8202812194864,-1.58015958259838,31.2857496387808));
#19967=CARTESIAN_POINT('Ctrl Pts',(-2.95013811989943,-1.29842478745623,
31.2654618482006));
#19968=CARTESIAN_POINT('Ctrl Pts',(-2.97214620391831,-1.24722479423274,
31.2618697520665));
#19969=CARTESIAN_POINT('Ctrl Pts',(-2.99713367544048,-1.1846698729509,31.2576161779332));
#19970=CARTESIAN_POINT('Ctrl Pts',(-3.00139183226039,-1.17383987635848,
31.2568845950233));
#19971=CARTESIAN_POINT('Ctrl Pts',(-3.00793651343244,-1.15692598202071,
31.2557498126236));
#19972=CARTESIAN_POINT('Ctrl Pts',(-3.01026340255732,-1.15085796070127,
31.2553442516362));
#19973=CARTESIAN_POINT('Ctrl Pts',(-3.01455545987411,-1.13956312768473,
31.2545922926781));
#19974=CARTESIAN_POINT('Ctrl Pts',(-3.01652537991746,-1.13433829859165,
31.2542456196517));
#19975=CARTESIAN_POINT('Ctrl Pts',(-3.02096498219883,-1.12246976560065,
31.2534607642309));
#19976=CARTESIAN_POINT('Ctrl Pts',(-3.0234263275321,-1.11582303373404,31.253023083904));
#19977=CARTESIAN_POINT('Ctrl Pts',(-3.03067807514303,-1.09603990659993,
31.2517257621092));
#19978=CARTESIAN_POINT('Ctrl Pts',(-3.03540500891705,-1.08288019664208,
31.2508698150855));
#19979=CARTESIAN_POINT('Ctrl Pts',(-3.07111359810302,-0.981396798428517,
31.2443199610372));
#19980=CARTESIAN_POINT('Ctrl Pts',(-3.09832295956663,-0.891782936280663,
31.2388316999514));
#19981=CARTESIAN_POINT('Ctrl Pts',(-3.18146583494294,-0.567806714320533,
31.2196163521395));
#19982=CARTESIAN_POINT('Ctrl Pts',(-3.21499791107935,-0.328527242136726,
31.2065163718238));
#19983=CARTESIAN_POINT('Ctrl Pts',(-3.22406238880603,0.0043147249046562,
31.1875618446388));
#19984=CARTESIAN_POINT('Ctrl Pts',(-3.2226227795599,0.096422956578223,31.182247215611));
#19985=CARTESIAN_POINT('Ctrl Pts',(-3.21395960204302,0.244409437609208,
31.1735063337456));
#19986=CARTESIAN_POINT('Ctrl Pts',(-3.20921208528118,0.300382273167392,
31.1701538681618));
#19987=CARTESIAN_POINT('Ctrl Pts',(-3.20110541513175,0.373278676709265,
31.1657155381103));
#19988=CARTESIAN_POINT('Ctrl Pts',(-3.19906959685009,0.390341576046077,
31.1646714850309));
#19989=CARTESIAN_POINT('Ctrl Pts',(-3.19552548077266,0.418153391734688,
31.1629609595805));
#19990=CARTESIAN_POINT('Ctrl Pts',(-3.19409914914591,0.428912553039472,
31.1622970888515));
#19991=CARTESIAN_POINT('Ctrl Pts',(-3.19124306187078,0.449652010736602,
31.1610131832165));
#19992=CARTESIAN_POINT('Ctrl Pts',(-3.18982076472645,0.45963321891602,31.1603933920889));
#19993=CARTESIAN_POINT('Ctrl Pts',(-3.18644363235984,0.482561910714854,
31.1589651962708));
#19994=CARTESIAN_POINT('Ctrl Pts',(-3.18445668596398,0.495504416694939,
31.1581557796873));
#19995=CARTESIAN_POINT('Ctrl Pts',(-3.17893589646574,0.530060130984325,
31.1559858406746));
#19996=CARTESIAN_POINT('Ctrl Pts',(-3.17526057334678,0.551649734347801,
31.1546208419077));
#19997=CARTESIAN_POINT('Ctrl Pts',(-3.1422953499445,0.734037756801617,31.1430088904198));
#19998=CARTESIAN_POINT('Ctrl Pts',(-3.10103669955303,0.892405907189711,
31.132376742876));
#19999=CARTESIAN_POINT('Ctrl Pts',(-2.96565101060818,1.28655298327257,31.1045839755335));
#20000=CARTESIAN_POINT('Ctrl Pts',(-2.85538558413461,1.51560965706892,31.0870977927304));
#20001=CARTESIAN_POINT('Ctrl Pts',(-2.68869285935838,1.77773195480971,31.0667650693938));
#20002=CARTESIAN_POINT('Ctrl Pts',(-2.65666160965921,1.82525347509511,31.0630687227994));
#20003=CARTESIAN_POINT('Ctrl Pts',(-2.61656374430491,1.8814487418211,31.0587089212942));
#20004=CARTESIAN_POINT('Ctrl Pts',(-2.60969727513731,1.89096148512838,31.0579712959332));
#20005=CARTESIAN_POINT('Ctrl Pts',(-2.59893438391404,1.90570200565681,31.0568292062978));
#20006=CARTESIAN_POINT('Ctrl Pts',(-2.59507386988263,1.91095569752275,31.0564223320511));
#20007=CARTESIAN_POINT('Ctrl Pts',(-2.58787856888038,1.92068561490598,31.055669185379));
#20008=CARTESIAN_POINT('Ctrl Pts',(-2.58454812680498,1.92516484996496,31.0553226300729));
#20009=CARTESIAN_POINT('Ctrl Pts',(-2.57697912184891,1.93528964331584,31.0545396248657));
#20010=CARTESIAN_POINT('Ctrl Pts',(-2.57273364691588,1.94092992718386,31.0541036671901));
#20011=CARTESIAN_POINT('Ctrl Pts',(-2.56010427991879,1.95759430307416,31.0528161688916));
#20012=CARTESIAN_POINT('Ctrl Pts',(-2.55166769308742,1.96857851748845,31.0519682403198));
#20013=CARTESIAN_POINT('Ctrl Pts',(-2.4880820055722,2.05026981782221,31.0456645919791));
#20014=CARTESIAN_POINT('Ctrl Pts',(-2.43006868209291,2.11870898558736,31.0403974542612));
#20015=CARTESIAN_POINT('Ctrl Pts',(-2.20264746053282,2.36534967227088,31.0210872459879));
#20016=CARTESIAN_POINT('Ctrl Pts',(-2.01589314191846,2.52640532284587,31.0077341262375));
#20017=CARTESIAN_POINT('Ctrl Pts',(-1.7369210814528,2.71617524019865,30.9885225928932));
#20018=CARTESIAN_POINT('Ctrl Pts',(-1.65905174396757,2.76442546979597,30.9832362985634));
#20019=CARTESIAN_POINT('Ctrl Pts',(-1.53047184248708,2.83670639101246,30.9745377745647));
#20020=CARTESIAN_POINT('Ctrl Pts',(-1.48100262988593,2.86284436320936,30.9711983993155));
#20021=CARTESIAN_POINT('Ctrl Pts',(-1.41550513974602,2.89529915609879,30.9667749924335));
#20022=CARTESIAN_POINT('Ctrl Pts',(-1.40006953146704,2.90279473840227,30.9657324159737));
#20023=CARTESIAN_POINT('Ctrl Pts',(-1.37477928726068,2.91482712197039,30.964023702122));
#20024=CARTESIAN_POINT('Ctrl Pts',(-1.36496017315769,2.91943812415988,30.9633601557511));
#20025=CARTESIAN_POINT('Ctrl Pts',(-1.34596882389628,2.92823960346182,30.9620764502105));
#20026=CARTESIAN_POINT('Ctrl Pts',(-1.33679982089459,2.93243678283953,30.9614565325207));
#20027=CARTESIAN_POINT('Ctrl Pts',(-1.31566848609356,2.94199010561221,30.9600274321575));
#20028=CARTESIAN_POINT('Ctrl Pts',(-1.30369293757034,2.94731641721606,30.9592172333981));
#20029=CARTESIAN_POINT('Ctrl Pts',(-1.2715820962703,2.96136421675292,30.9570438325861));
#20030=CARTESIAN_POINT('Ctrl Pts',(-1.25138993735685,2.9699532383585,30.9556761317178));
#20031=CARTESIAN_POINT('Ctrl Pts',(-1.07807091397471,3.0415956560808,30.9439259803328));
#20032=CARTESIAN_POINT('Ctrl Pts',(-0.920406057871046,3.09295628540771,
30.9331476492001));
#20033=CARTESIAN_POINT('Ctrl Pts',(-0.508391983690069,3.19287117832151,
30.904858124988));
#20034=CARTESIAN_POINT('Ctrl Pts',(-0.250868985372037,3.22334449882516,
30.8870089342507));
#20035=CARTESIAN_POINT('Ctrl Pts',(0.0582938486393527,3.22262268236336,
30.8668480082903));
#20036=CARTESIAN_POINT('Ctrl Pts',(0.10905700270632,3.22130445347779,30.8635819177435));
#20037=CARTESIAN_POINT('Ctrl Pts',(0.171073999725646,3.21822611402835,30.8596626680382));
#20038=CARTESIAN_POINT('Ctrl Pts',(0.182374135131546,3.21760552557616,30.8589514272067));
#20039=CARTESIAN_POINT('Ctrl Pts',(0.200088061438667,3.21653908083966,30.8578412718011));
#20040=CARTESIAN_POINT('Ctrl Pts',(0.206504055790797,3.21613354317833,30.8574401558536));
#20041=CARTESIAN_POINT('Ctrl Pts',(0.218499544670998,3.21533929656842,30.8566921133601));
#20042=CARTESIAN_POINT('Ctrl Pts',(0.224079178379036,3.21495526648418,30.8563449384982));
#20043=CARTESIAN_POINT('Ctrl Pts',(0.236829158162078,3.21404436832022,30.8555533498293));
#20044=CARTESIAN_POINT('Ctrl Pts',(0.243998746662671,3.21350803105829,30.8551094734122));
#20045=CARTESIAN_POINT('Ctrl Pts',(0.266089974185052,3.21178108801797,30.8537454748703));
#20046=CARTESIAN_POINT('Ctrl Pts',(0.281005411508791,3.21051049063543,30.8528297308612));
#20047=CARTESIAN_POINT('Ctrl Pts',(0.430928253530235,3.1966862288378,30.8436725143295));
#20048=CARTESIAN_POINT('Ctrl Pts',(0.565042596116501,3.17572641435453,30.8358654207246));
#20049=CARTESIAN_POINT('Ctrl Pts',(0.881951424925628,3.10547770356722,30.8175139443786));
#20050=CARTESIAN_POINT('Ctrl Pts',(1.06249494998204,3.04843178168042,30.8071207834093));
#20051=CARTESIAN_POINT('Ctrl Pts',(1.32719462947861,2.93840302586508,30.7908435446531));
#20052=CARTESIAN_POINT('Ctrl Pts',(1.41563049331865,2.89683378837911,30.7852204827145));
#20053=CARTESIAN_POINT('Ctrl Pts',(1.55385759683216,2.82401745936542,30.7760201045856));
#20054=CARTESIAN_POINT('Ctrl Pts',(1.60492094477216,2.79531324724433,30.7725271622462));
#20055=CARTESIAN_POINT('Ctrl Pts',(1.67013783343983,2.75627673126546,30.7679289231176));
#20056=CARTESIAN_POINT('Ctrl Pts',(1.68503088304417,2.74719724566579,30.7668693605738));
#20057=CARTESIAN_POINT('Ctrl Pts',(1.70911854077668,2.73224274398326,30.7651397996345));
#20058=CARTESIAN_POINT('Ctrl Pts',(1.71835843647854,2.72644106439706,30.7644725154302));
#20059=CARTESIAN_POINT('Ctrl Pts',(1.73606338099305,2.71519847485267,30.7631864263824));
#20060=CARTESIAN_POINT('Ctrl Pts',(1.74453276832865,2.70976460919209,30.7625678891817));
#20061=CARTESIAN_POINT('Ctrl Pts',(1.76385788737466,2.69723767452166,30.7611488423101));
#20062=CARTESIAN_POINT('Ctrl Pts',(1.77469648085034,2.69011860568836,30.7603473631959));
#20063=CARTESIAN_POINT('Ctrl Pts',(1.80336345908475,2.67104074401438,30.7582124483637));
#20064=CARTESIAN_POINT('Ctrl Pts',(1.82111558333641,2.65896905169235,30.7568747606541));
#20065=CARTESIAN_POINT('Ctrl Pts',(1.95773006115948,2.56405945033691,30.7464567432735));
#20066=CARTESIAN_POINT('Ctrl Pts',(2.07098836663216,2.47348028582223,30.7370766980317));
#20067=CARTESIAN_POINT('Ctrl Pts',(2.33146681896542,2.23469487041166,30.7136373847543));
#20068=CARTESIAN_POINT('Ctrl Pts',(2.47113258664423,2.07920484032101,30.6993659779647));
#20069=CARTESIAN_POINT('Ctrl Pts',(2.64268674453016,1.84630635200738,30.679974775298));
#20070=CARTESIAN_POINT('Ctrl Pts',(2.68812795877596,1.77949719303746,30.6746168887248));
#20071=CARTESIAN_POINT('Ctrl Pts',(2.75354887707876,1.67507842042336,30.6666233229205));
#20072=CARTESIAN_POINT('Ctrl Pts',(2.7753725972629,1.63866607136462,30.6639032197766));
#20073=CARTESIAN_POINT('Ctrl Pts',(2.80178477506933,1.59255577540493,30.6605520964186));
#20074=CARTESIAN_POINT('Ctrl Pts',(2.80705167734764,1.58325383684642,30.6598807474611));
#20075=CARTESIAN_POINT('Ctrl Pts',(2.81534415602522,1.56843693169881,30.6588189927131));
#20076=CARTESIAN_POINT('Ctrl Pts',(2.81839998076755,1.5629391144897,30.6584266858936));
#20077=CARTESIAN_POINT('Ctrl Pts',(2.82415556812372,1.55251230976243,30.6576858473924));
#20078=CARTESIAN_POINT('Ctrl Pts',(2.82685849974318,1.54758526995826,30.6573371217821));
#20079=CARTESIAN_POINT('Ctrl Pts',(2.8330421339967,1.53624317590814,30.6565374057121));
#20080=CARTESIAN_POINT('Ctrl Pts',(2.83651394110666,1.52982335349463,30.6560869855057));
#20081=CARTESIAN_POINT('Ctrl Pts',(2.84574430403583,1.51261576489752,30.6548855001183));
#20082=CARTESIAN_POINT('Ctrl Pts',(2.85146338551973,1.501806801233,30.6541368745573));
#20083=CARTESIAN_POINT('Ctrl Pts',(2.89345264334473,1.42134323672057,30.6486070921127));
#20084=CARTESIAN_POINT('Ctrl Pts',(2.92723075776941,1.35040997656245,30.6439708702697));
#20085=CARTESIAN_POINT('Ctrl Pts',(3.04832021717778,1.07017268621329,30.6262973206752));
#20086=CARTESIAN_POINT('Ctrl Pts',(3.11604440259237,0.853116488909561,30.6139241494622));
#20087=CARTESIAN_POINT('Ctrl Pts',(3.19318041282869,0.466611307229636,30.5916712309533));
#20088=CARTESIAN_POINT('Ctrl Pts',(3.2130969796351,0.300206582904236,30.5820298296068));
#20089=CARTESIAN_POINT('Ctrl Pts',(3.22096377766471,0.109777502715783,30.5705568331624));
#20090=CARTESIAN_POINT('Ctrl Pts',(3.22167227122581,0.0865245070454551,
30.5691488248579));
#20091=CARTESIAN_POINT('Ctrl Pts',(3.2223679454749,0.0510940992607525,30.566991920158));
#20092=CARTESIAN_POINT('Ctrl Pts',(3.22253796761573,0.0389207383701022,
30.566248768067));
#20093=CARTESIAN_POINT('Ctrl Pts',(3.2227136708738,0.0177508262931659,30.5649526866344));
#20094=CARTESIAN_POINT('Ctrl Pts',(3.22275066524682,0.00875461658659629,
30.5644007476076));
#20095=CARTESIAN_POINT('Ctrl Pts',(3.2227491527339,-0.0114245863545412,
30.5631600379063));
#20096=CARTESIAN_POINT('Ctrl Pts',(3.22269010644003,-0.0226074196351687,
30.5624706285465));
#20097=CARTESIAN_POINT('Ctrl Pts',(3.22237706742979,-0.0524624874323674,
30.5606250826662));
#20098=CARTESIAN_POINT('Ctrl Pts',(3.22201898686414,-0.0711329874130248,
30.5594656924567));
#20099=CARTESIAN_POINT('Ctrl Pts',(3.21950594560912,-0.161287200730689,
30.5538412841109));
#20100=CARTESIAN_POINT('Ctrl Pts',(3.21513434264981,-0.232684209076111,
30.5493072526171));
#20101=CARTESIAN_POINT('Ctrl Pts',(3.18314952522559,-0.570391177725851,
30.5274655471515));
#20102=CARTESIAN_POINT('Ctrl Pts',(3.12479772400483,-0.832695382683397,
30.5092072556514));
#20103=CARTESIAN_POINT('Ctrl Pts',(2.98780638003923,-1.21595981197791,30.4817858873665));
#20104=CARTESIAN_POINT('Ctrl Pts',(2.93242147285564,-1.34404571259879,30.4725114262139));
#20105=CARTESIAN_POINT('Ctrl Pts',(2.86207593314905,-1.48150730125619,30.4627203838548));
#20106=CARTESIAN_POINT('Ctrl Pts',(2.85514973213737,-1.49481188059214,30.4617745474452));
#20107=CARTESIAN_POINT('Ctrl Pts',(2.84476370194231,-1.51442689362191,30.4603833321143));
#20108=CARTESIAN_POINT('Ctrl Pts',(2.84137533746258,-1.52077464801888,30.4599336162215));
#20109=CARTESIAN_POINT('Ctrl Pts',(2.8353152461268,-1.53203665224649,30.4591367151749));
#20110=CARTESIAN_POINT('Ctrl Pts',(2.83265196154433,-1.53695533936767,30.4587890027692));
#20111=CARTESIAN_POINT('Ctrl Pts',(2.82690195247177,-1.54750902830305,30.4580436745375));
#20112=CARTESIAN_POINT('Ctrl Pts',(2.82381118769628,-1.55314172550802,30.4576463221048));
#20113=CARTESIAN_POINT('Ctrl Pts',(2.81523830804946,-1.56865499986002,30.4565530736595));
#20114=CARTESIAN_POINT('Ctrl Pts',(2.80972097959947,-1.57851615935056,30.4558593959542));
#20115=CARTESIAN_POINT('Ctrl Pts',(2.779255255878,-1.63230191652864,30.4520816209732));
#20116=CARTESIAN_POINT('Ctrl Pts',(2.75332709287934,-1.67566700257382,30.4490568307441));
#20117=CARTESIAN_POINT('Ctrl Pts',(2.58851219322617,-1.9371588184228,30.4308348997187));
#20118=CARTESIAN_POINT('Ctrl Pts',(2.42479647900398,-2.13854444366878,30.416813403412));
#20119=CARTESIAN_POINT('Ctrl Pts',(2.11958316106935,-2.43329622748664,30.3928574525194));
#20120=CARTESIAN_POINT('Ctrl Pts',(1.99173330265579,-2.5390059179462,30.383316334553));
#20121=CARTESIAN_POINT('Ctrl Pts',(1.838397560125,-2.64705374646689,30.3720343478765));
#20122=CARTESIAN_POINT('Ctrl Pts',(1.8203308608015,-2.65951022680665,30.3707077322552));
#20123=CARTESIAN_POINT('Ctrl Pts',(1.79127237559914,-2.67911041881263,30.3685775453819));
#20124=CARTESIAN_POINT('Ctrl Pts',(1.78036157415552,-2.68637339494712,30.3677784956791));
#20125=CARTESIAN_POINT('Ctrl Pts',(1.76097861270702,-2.69910607004278,30.3663602319654));
#20126=CARTESIAN_POINT('Ctrl Pts',(1.75252446740648,-2.70460297256803,30.3657420509058));
#20127=CARTESIAN_POINT('Ctrl Pts',(1.73492274372522,-2.71593046823951,30.3644557714514));
#20128=CARTESIAN_POINT('Ctrl Pts',(1.72577125871732,-2.72175472682334,30.3637874469982));
#20129=CARTESIAN_POINT('Ctrl Pts',(1.70206890478329,-2.73667195952448,30.3620575159931));
#20130=CARTESIAN_POINT('Ctrl Pts',(1.68747465287437,-2.7456950391897,30.3609933389918));
#20131=CARTESIAN_POINT('Ctrl Pts',(1.62499990890735,-2.78363459208889,30.356441510777));
#20132=CARTESIAN_POINT('Ctrl Pts',(1.57644539967755,-2.81141699422034,30.3529127834915));
#20133=CARTESIAN_POINT('Ctrl Pts',(1.44657510623723,-2.88130522581978,30.343491399806));
#20134=CARTESIAN_POINT('Ctrl Pts',(1.36414987205505,-2.92123124314398,30.3375277729438));
#20135=CARTESIAN_POINT('Ctrl Pts',(1.05434274108739,-3.05532593201959,30.3151995017479));
#20136=CARTESIAN_POINT('Ctrl Pts',(0.818117910257989,-3.12687108220597,
30.298267348129));
#20137=CARTESIAN_POINT('Ctrl Pts',(0.488009825825243,-3.18684390698463,
30.2759664506942));
#20138=CARTESIAN_POINT('Ctrl Pts',(0.399314636015608,-3.1991684353077,30.2701133695743));
#20139=CARTESIAN_POINT('Ctrl Pts',(0.296433884548542,-3.20911766110724,
30.2635670281546));
#20140=CARTESIAN_POINT('Ctrl Pts',(0.282645724258407,-3.21036144717234,
30.2626947095551));
#20141=CARTESIAN_POINT('Ctrl Pts',(0.261816170163801,-3.21210517770268,
30.2613849321946));
#20142=CARTESIAN_POINT('Ctrl Pts',(0.254780655932871,-3.21267088249002,
30.260943914004));
#20143=CARTESIAN_POINT('Ctrl Pts',(0.242178158558334,-3.21364255269438,
30.2601564715131));
#20144=CARTESIAN_POINT('Ctrl Pts',(0.236611948808043,-3.21405717189382,
30.2598095685211));
#20145=CARTESIAN_POINT('Ctrl Pts',(0.224540875129676,-3.21492480071507,
30.2590592023079));
#20146=CARTESIAN_POINT('Ctrl Pts',(0.218035724807319,-3.21537252948138,
30.2586560387003));
#20147=CARTESIAN_POINT('Ctrl Pts',(0.199818324534206,-3.21657083514405,
30.257530276326));
#20148=CARTESIAN_POINT('Ctrl Pts',(0.188103126212695,-3.21727719105762,
30.2568101186542));
#20149=CARTESIAN_POINT('Ctrl Pts',(0.119100684118839,-3.22105942829446,
30.2525893598998));
#20150=CARTESIAN_POINT('Ctrl Pts',(0.0617394618062305,-3.22266938956621,
30.2491656866355));
#20151=CARTESIAN_POINT('Ctrl Pts',(-0.248902013345923,-3.22308983224044,
30.2309381426778));
#20152=CARTESIAN_POINT('Ctrl Pts',(-0.501346255244765,-3.19357775135259,
30.2171926214421));
#20153=CARTESIAN_POINT('Ctrl Pts',(-0.906700856111815,-3.09688779334011,
30.193651224675));
#20154=CARTESIAN_POINT('Ctrl Pts',(-1.0625173357958,-3.04694387582986,30.1842334347241));
#20155=CARTESIAN_POINT('Ctrl Pts',(-1.2341504148667,-2.97715802610212,30.173089459085));
#20156=CARTESIAN_POINT('Ctrl Pts',(-1.25435227359172,-2.96870299901701,
30.1717655182531));
#20157=CARTESIAN_POINT('Ctrl Pts',(-1.28649269723778,-2.95486472733944,
30.1696388162053));
#20158=CARTESIAN_POINT('Ctrl Pts',(-1.29848756447217,-2.9496133736288,30.1688405529336));
#20159=CARTESIAN_POINT('Ctrl Pts',(-1.31966087720477,-2.94018951421828,
30.1674231994489));
#20160=CARTESIAN_POINT('Ctrl Pts',(-1.3288524224391,-2.93604673771598,30.1668051377803));
#20161=CARTESIAN_POINT('Ctrl Pts',(-1.34789803597533,-2.92735482013418,
30.1655186223799));
#20162=CARTESIAN_POINT('Ctrl Pts',(-1.35774885287747,-2.92279889938476,
30.1648499401821));
#20163=CARTESIAN_POINT('Ctrl Pts',(-1.38313657176366,-2.91090124890507,
30.1631180419268));
#20164=CARTESIAN_POINT('Ctrl Pts',(-1.39863794910964,-2.90348492778955,
30.1620522443065));
#20165=CARTESIAN_POINT('Ctrl Pts',(-1.43458046966549,-2.88593433101557,
30.1595612713528));
#20166=CARTESIAN_POINT('Ctrl Pts',(-1.4549737214081,-2.87570676985225,30.1581329162072));
#20167=CARTESIAN_POINT('Ctrl Pts',(-1.47525540759407,-2.86526421903189,
30.1566970682534));
#20168=CARTESIAN_POINT('',(3.22274869089678,-0.00290479312253886,30.3149198866253));
#20169=CARTESIAN_POINT('Ctrl Pts',(-1.4752551445451,-2.86526435446945,29.9088139162969));
#20170=CARTESIAN_POINT('Ctrl Pts',(-1.32485372920929,-2.94270239657363,
29.9183783199176));
#20171=CARTESIAN_POINT('Ctrl Pts',(-1.16846286164701,-3.00824305892808,
29.9277144246265));
#20172=CARTESIAN_POINT('Ctrl Pts',(-0.851862684615299,-3.112442056773,29.9465412399396));
#20173=CARTESIAN_POINT('Ctrl Pts',(-0.692562113047588,-3.15171586102294,
29.9559833170831));
#20174=CARTESIAN_POINT('Ctrl Pts',(-0.509374902386215,-3.18231590788476,
29.9671541637009));
#20175=CARTESIAN_POINT('Ctrl Pts',(-0.4877348670029,-3.18570431647154,29.968478336435));
#20176=CARTESIAN_POINT('Ctrl Pts',(-0.453107146559448,-3.19076525292545,
29.9706051992506));
#20177=CARTESIAN_POINT('Ctrl Pts',(-0.440140653869682,-3.19257970650865,
29.971403388468));
#20178=CARTESIAN_POINT('Ctrl Pts',(-0.417173495792871,-3.1956510172556,
29.9728204824632));
#20179=CARTESIAN_POINT('Ctrl Pts',(-0.407177257856685,-3.19694007242823,
29.9734383582769));
#20180=CARTESIAN_POINT('Ctrl Pts',(-0.386409859560162,-3.19951913003204,
29.9747243583272));
#20181=CARTESIAN_POINT('Ctrl Pts',(-0.375637917694197,-3.20080167976545,
29.9753927102387));
#20182=CARTESIAN_POINT('Ctrl Pts',(-0.347798963901124,-3.20397382868587,
29.9771234744598));
#20183=CARTESIAN_POINT('Ctrl Pts',(-0.330723126053853,-3.20578143510953,
29.9781884635707));
#20184=CARTESIAN_POINT('Ctrl Pts',(-0.261600732279352,-3.21254042142824,
29.9825136451671));
#20185=CARTESIAN_POINT('Ctrl Pts',(-0.209454085725985,-3.21636120036841,
29.9858091754865));
#20186=CARTESIAN_POINT('Ctrl Pts',(-0.0723877919872352,-3.22305672261099,
29.9945618329305));
#20187=CARTESIAN_POINT('Ctrl Pts',(0.012588494431664,-3.22384462017334,
30.0000798910321));
#20188=CARTESIAN_POINT('Ctrl Pts',(0.370305917249913,-3.21301839814294,
30.0236731377819));
#20189=CARTESIAN_POINT('Ctrl Pts',(0.640931400912043,-3.17014162748544,
30.0425334838655));
#20190=CARTESIAN_POINT('Ctrl Pts',(0.973906804136973,-3.07296183525789,
30.0654414448459));
#20191=CARTESIAN_POINT('Ctrl Pts',(1.04418499877582,-3.04979810988885,30.0702500252699));
#20192=CARTESIAN_POINT('Ctrl Pts',(1.12491472290792,-3.02007112008365,30.0756944460744));
#20193=CARTESIAN_POINT('Ctrl Pts',(1.13619687186787,-3.01584472133704,30.0764534755096));
#20194=CARTESIAN_POINT('Ctrl Pts',(1.15422461886513,-3.00897583380398,30.0776630728587));
#20195=CARTESIAN_POINT('Ctrl Pts',(1.16098533999302,-3.00637374289373,30.0781159563752));
#20196=CARTESIAN_POINT('Ctrl Pts',(1.17296694083972,-3.00171577612577,30.0789171905565));
#20197=CARTESIAN_POINT('Ctrl Pts',(1.17819129129456,-2.99966903639722,30.0792660827025));
#20198=CARTESIAN_POINT('Ctrl Pts',(1.18928602265496,-2.99528900483679,30.0800059871108));
#20199=CARTESIAN_POINT('Ctrl Pts',(1.19515488423319,-2.99295209959919,30.0803967775628));
#20200=CARTESIAN_POINT('Ctrl Pts',(1.21085322373667,-2.98664768441831,30.0814405670009));
#20201=CARTESIAN_POINT('Ctrl Pts',(1.22067016258588,-2.98264887001018,30.0820917022877));
#20202=CARTESIAN_POINT('Ctrl Pts',(1.26915576276783,-2.96261935430214,30.0853005707879));
#20203=CARTESIAN_POINT('Ctrl Pts',(1.30753127377072,-2.94588393266936,30.0878180149808));
#20204=CARTESIAN_POINT('Ctrl Pts',(1.4177226146433,-2.89525214197987,30.0950119147973));
#20205=CARTESIAN_POINT('Ctrl Pts',(1.48862865463231,-2.85944205439147,30.0995978907407));
#20206=CARTESIAN_POINT('Ctrl Pts',(1.6995345611077,-2.7429527563825,30.1133165368947));
#20207=CARTESIAN_POINT('Ctrl Pts',(1.83485805341036,-2.65433739575478,30.1222370050728));
#20208=CARTESIAN_POINT('Ctrl Pts',(2.1155308730456,-2.43878029477274,30.1421070957447));
#20209=CARTESIAN_POINT('Ctrl Pts',(2.2572735480932,-2.30820744233556,30.1530923352389));
#20210=CARTESIAN_POINT('Ctrl Pts',(2.40147453404029,-2.14930984201592,30.1659945889721));
#20211=CARTESIAN_POINT('Ctrl Pts',(2.41625751356064,-2.13267726690592,30.1673395620991));
#20212=CARTESIAN_POINT('Ctrl Pts',(2.4395295315613,-2.1059409579539,30.1694935107113));
#20213=CARTESIAN_POINT('Ctrl Pts',(2.44813097432026,-2.09593568083501,30.1702978002006));
#20214=CARTESIAN_POINT('Ctrl Pts',(2.46320463085365,-2.07818248064839,30.1717219714086));
#20215=CARTESIAN_POINT('Ctrl Pts',(2.4697023715187,-2.07045639141828,30.1723407899316));
#20216=CARTESIAN_POINT('Ctrl Pts',(2.48307933527197,-2.05439804467347,30.1736250420898));
#20217=CARTESIAN_POINT('Ctrl Pts',(2.4899531614543,-2.046061475231,30.1742906850085));
#20218=CARTESIAN_POINT('Ctrl Pts',(2.50751825059293,-2.02453894905689,30.1760065393413));
#20219=CARTESIAN_POINT('Ctrl Pts',(2.51814738323025,-2.01130292891549,30.1770592438148));
#20220=CARTESIAN_POINT('Ctrl Pts',(2.56153955655275,-1.95638529373948,30.1814172070548));
#20221=CARTESIAN_POINT('Ctrl Pts',(2.59337464158526,-1.91398425971639,30.184759029172));
#20222=CARTESIAN_POINT('Ctrl Pts',(2.70876901566231,-1.7521236673462,30.1974394895382));
#20223=CARTESIAN_POINT('Ctrl Pts',(2.7852287580075,-1.62783849958295,30.2070350036993));
#20224=CARTESIAN_POINT('Ctrl Pts',(2.90641699151178,-1.39715633109783,30.2245044350131));
#20225=CARTESIAN_POINT('Ctrl Pts',(2.9543523452791,-1.29271282751195,30.2322968160354));
#20226=CARTESIAN_POINT('Ctrl Pts',(3.0269647015746,-1.1092369646233,30.2456396261825));
#20227=CARTESIAN_POINT('Ctrl Pts',(3.05436485626434,-1.03139629245465,30.2511975464793));
#20228=CARTESIAN_POINT('Ctrl Pts',(3.10453143215176,-0.869258632403087,
30.2624688219088));
#20229=CARTESIAN_POINT('Ctrl Pts',(3.12692291176562,-0.78490894975683,30.2681683621354));
#20230=CARTESIAN_POINT('Ctrl Pts',(3.14885289283336,-0.686317917875907,
30.2745645576127));
#20231=CARTESIAN_POINT('Ctrl Pts',(3.15175401612548,-0.672869573423179,
30.2754313632553));
#20232=CARTESIAN_POINT('Ctrl Pts',(3.15600906688295,-0.652513500472056,
30.2767344173874));
#20233=CARTESIAN_POINT('Ctrl Pts',(3.15742658503816,-0.645619439665913,
30.2771741735542));
#20234=CARTESIAN_POINT('Ctrl Pts',(3.15992711405623,-0.633252962864281,
30.2779601508414));
#20235=CARTESIAN_POINT('Ctrl Pts',(3.16101850703718,-0.627782351471588,
30.2783068441306));
#20236=CARTESIAN_POINT('Ctrl Pts',(3.16335686477289,-0.615900612076316,
30.279057651223));
#20237=CARTESIAN_POINT('Ctrl Pts',(3.16459854341345,-0.609488538591633,
30.2794614607852));
#20238=CARTESIAN_POINT('Ctrl Pts',(3.16711650688184,-0.596270527922909,
30.2802911471517));
#20239=CARTESIAN_POINT('Ctrl Pts',(3.16839036745164,-0.589464156778562,
30.280716886519));
#20240=CARTESIAN_POINT('Ctrl Pts',(3.1715905858526,-0.572054933614299,30.2818021453007));
#20241=CARTESIAN_POINT('Ctrl Pts',(3.17348573548982,-0.561446333459101,
30.2824599716221));
#20242=CARTESIAN_POINT('Ctrl Pts',(3.20671468066524,-0.369893363558426,
30.2942782071231));
#20243=CARTESIAN_POINT('Ctrl Pts',(3.22258313323825,-0.186584217027832,
30.3046373579577));
#20244=CARTESIAN_POINT('Ctrl Pts',(3.22274869089678,-0.00290479312253886,
30.3149198866253));
#20245=CARTESIAN_POINT('Ctrl Pts',(3.22274868914525,-0.00290673572484593,
30.3149197778768));
#20246=CARTESIAN_POINT('Ctrl Pts',(3.22299387022043,0.268929806518607,30.3301374173408));
#20247=CARTESIAN_POINT('Ctrl Pts',(3.18884801419423,0.539685140348905,30.3451725098073));
#20248=CARTESIAN_POINT('Ctrl Pts',(3.11297967882882,0.834591324622212,30.3633797714072));
#20249=CARTESIAN_POINT('Ctrl Pts',(3.10435840602317,0.86610849669144,30.365348112516));
#20250=CARTESIAN_POINT('Ctrl Pts',(3.09137296792005,0.910892705231855,30.3681794413213));
#20251=CARTESIAN_POINT('Ctrl Pts',(3.08739929600207,0.924271564355853,30.3690296899358));
#20252=CARTESIAN_POINT('Ctrl Pts',(3.08037585612877,0.947367863832681,30.3705053229563));
#20253=CARTESIAN_POINT('Ctrl Pts',(3.07736667263886,0.957097509555341,30.3711293679604));
#20254=CARTESIAN_POINT('Ctrl Pts',(3.07150315950228,0.975742554942193,30.3723299386522));
#20255=CARTESIAN_POINT('Ctrl Pts',(3.06865600022167,0.98466011481312,30.3729062225381));
#20256=CARTESIAN_POINT('Ctrl Pts',(3.06111994013475,1.00791357656737,30.3744144305873));
#20257=CARTESIAN_POINT('Ctrl Pts',(3.05636921845122,1.0222290613023,30.3753483909337));
#20258=CARTESIAN_POINT('Ctrl Pts',(3.03964970001899,1.0714518300963,30.3785789312619));
#20259=CARTESIAN_POINT('Ctrl Pts',(3.02718230933927,1.10618552075993,30.3808919785199));
#20260=CARTESIAN_POINT('Ctrl Pts',(2.93606491307461,1.34694978546955,30.3971661942472));
#20261=CARTESIAN_POINT('Ctrl Pts',(2.83705805865563,1.54461003308747,30.4118281129002));
#20262=CARTESIAN_POINT('Ctrl Pts',(2.66107604981017,1.82107033357091,30.4339821368988));
#20263=CARTESIAN_POINT('Ctrl Pts',(2.59899486772562,1.90862492348789,30.441265520862));
#20264=CARTESIAN_POINT('Ctrl Pts',(2.48040093553641,2.0593375522211,30.4541381952754));
#20265=CARTESIAN_POINT('Ctrl Pts',(2.42554285634798,2.12367695504919,30.4597535932905));
#20266=CARTESIAN_POINT('Ctrl Pts',(2.33864856792758,2.21782344081351,30.4680719323454));
#20267=CARTESIAN_POINT('Ctrl Pts',(2.30843324873756,2.24925639293838,30.4708674635473));
#20268=CARTESIAN_POINT('Ctrl Pts',(2.2701371149384,2.28751086217601,30.4742819446518));
#20269=CARTESIAN_POINT('Ctrl Pts',(2.26264993918842,2.29491693207852,30.4749435745963));
#20270=CARTESIAN_POINT('Ctrl Pts',(2.25053885884961,2.30677993019094,30.4760041130781));
#20271=CARTESIAN_POINT('Ctrl Pts',(2.24593777582064,2.31125989676106,30.4764047895648));
#20272=CARTESIAN_POINT('Ctrl Pts',(2.23730539585466,2.31961492372251,30.4771523109207));
#20273=CARTESIAN_POINT('Ctrl Pts',(2.2332774503664,2.32349320183066,30.4774994021357));
#20274=CARTESIAN_POINT('Ctrl Pts',(2.22404408222566,2.33233729041339,30.4782911798068));
#20275=CARTESIAN_POINT('Ctrl Pts',(2.21883212167112,2.33729615884314,30.4787353268226));
#20276=CARTESIAN_POINT('Ctrl Pts',(2.20270222450377,2.352540213345,30.4801014585476));
#20277=CARTESIAN_POINT('Ctrl Pts',(2.19172887048058,2.36276683651309,30.4810190438877));
#20278=CARTESIAN_POINT('Ctrl Pts',(2.07764972801598,2.46760430996102,30.4904421005458));
#20279=CARTESIAN_POINT('Ctrl Pts',(1.96854325791587,2.55549350279578,30.4984846196199));
#20280=CARTESIAN_POINT('Ctrl Pts',(1.63425776547915,2.7906145360599,30.5215615069101));
#20281=CARTESIAN_POINT('Ctrl Pts',(1.39600310008242,2.91710501024149,30.5362192696091));
#20282=CARTESIAN_POINT('Ctrl Pts',(1.07937316053417,3.03742848432863,30.5560479170053));
#20283=CARTESIAN_POINT('Ctrl Pts',(1.01314538403693,3.06015580632849,30.5602061506008));
#20284=CARTESIAN_POINT('Ctrl Pts',(0.928422490394513,3.08617828473099,30.5655620767027));
#20285=CARTESIAN_POINT('Ctrl Pts',(0.910564579107442,3.09149427469589,30.566692977984));
#20286=CARTESIAN_POINT('Ctrl Pts',(0.881927602823141,3.09974935519481,30.5685100534215));
#20287=CARTESIAN_POINT('Ctrl Pts',(0.871177436669819,3.10278781590461,30.569192971159));
#20288=CARTESIAN_POINT('Ctrl Pts',(0.850780681171142,3.10843846208108,30.5704903000512));
#20289=CARTESIAN_POINT('Ctrl Pts',(0.841137295452415,3.11106179408419,30.5711043390545));
#20290=CARTESIAN_POINT('Ctrl Pts',(0.819240825401045,3.11690913623143,30.5725001869886));
#20291=CARTESIAN_POINT('Ctrl Pts',(0.806980673304221,3.12010581216021,30.5732828742488));
#20292=CARTESIAN_POINT('Ctrl Pts',(0.775300955426744,3.12816667820165,30.5753083647325));
#20293=CARTESIAN_POINT('Ctrl Pts',(0.755854568688049,3.13292230670779,30.5765546574748));
#20294=CARTESIAN_POINT('Ctrl Pts',(0.631613941120976,3.16208138750361,30.5845370279462));
#20295=CARTESIAN_POINT('Ctrl Pts',(0.525708111837543,3.18140244171346,30.5914350954561));
#20296=CARTESIAN_POINT('Ctrl Pts',(0.172200902407954,3.22776140336313,30.614775027036));
#20297=CARTESIAN_POINT('Ctrl Pts',(-0.0775480296026197,3.2314172595377,
30.6318448310135));
#20298=CARTESIAN_POINT('Ctrl Pts',(-0.405272945825708,3.19817945815858,
30.6539250427879));
#20299=CARTESIAN_POINT('Ctrl Pts',(-0.485036647610255,3.1870580873313,30.6592648836753));
#20300=CARTESIAN_POINT('Ctrl Pts',(-0.606000017891726,3.16554497551066,
30.6672346703614));
#20301=CARTESIAN_POINT('Ctrl Pts',(-0.647547137155879,3.15730805121099,
30.6699485062906));
#20302=CARTESIAN_POINT('Ctrl Pts',(-0.699354139006458,3.14597129502787,
30.6732928843781));
#20303=CARTESIAN_POINT('Ctrl Pts',(-0.709774929078797,3.14363661362401,
30.6739635714577));
#20304=CARTESIAN_POINT('Ctrl Pts',(-0.726311354266359,3.13984536177924,
30.6750244366579));
#20305=CARTESIAN_POINT('Ctrl Pts',(-0.732434554206835,3.13842264595356,
30.6754165114065));
#20306=CARTESIAN_POINT('Ctrl Pts',(-0.744022277752315,3.13569449670675,
30.6761570154587));
#20307=CARTESIAN_POINT('Ctrl Pts',(-0.749487480946366,3.1343927071772,30.6765056379766));
#20308=CARTESIAN_POINT('Ctrl Pts',(-0.762044560734919,3.13136694026463,
30.6773052443543));
#20309=CARTESIAN_POINT('Ctrl Pts',(-0.769134001743944,3.12963316012505,
30.67775565752));
#20310=CARTESIAN_POINT('Ctrl Pts',(-0.788089971592249,3.12492902215584,
30.6789573873019));
#20311=CARTESIAN_POINT('Ctrl Pts',(-0.799945716954668,3.12191512661602,
30.6797062617465));
#20312=CARTESIAN_POINT('Ctrl Pts',(-0.887947450061585,3.09900963527778,
30.6852465706928));
#20313=CARTESIAN_POINT('Ctrl Pts',(-0.963365966683503,3.07640043542946,
30.6898924345344));
#20314=CARTESIAN_POINT('Ctrl Pts',(-1.05770200740286,3.04430978747947,30.6956606566191));
#20315=CARTESIAN_POINT('Ctrl Pts',(-1.0774509066064,3.03737636637863,30.6968657690571));
#20316=CARTESIAN_POINT('Ctrl Pts',(-1.31911400067984,2.94987994456055,30.7115978890921));
#20317=CARTESIAN_POINT('Ctrl Pts',(-1.53159893128865,2.84535915862341,30.7244532486862));
#20318=CARTESIAN_POINT('Ctrl Pts',(-1.80826268273697,2.6692214784955,30.7431256140288));
#20319=CARTESIAN_POINT('Ctrl Pts',(-1.88360770977575,2.6165965107142,30.7484283434048));
#20320=CARTESIAN_POINT('Ctrl Pts',(-2.00115126855666,2.52678746529781,30.7571512147674));
#20321=CARTESIAN_POINT('Ctrl Pts',(-2.04480607404662,2.49159162754908,30.7604979552525));
#20322=CARTESIAN_POINT('Ctrl Pts',(-2.10059938843576,2.44415518329824,30.7649295346038));
#20323=CARTESIAN_POINT('Ctrl Pts',(-2.11359073944614,2.43292961655727,30.7659727162362));
#20324=CARTESIAN_POINT('Ctrl Pts',(-2.13464259878507,2.41444325045045,30.7676820211003));
#20325=CARTESIAN_POINT('Ctrl Pts',(-2.14275734803602,2.40724451958692,30.7683455481789));
#20326=CARTESIAN_POINT('Ctrl Pts',(-2.15834156805202,2.3932782596782,30.7696289339581));
#20327=CARTESIAN_POINT('Ctrl Pts',(-2.16581594782148,2.38651637939239,30.7702485498394));
#20328=CARTESIAN_POINT('Ctrl Pts',(-2.18292704329954,2.37088981895917,30.7716765481376));
#20329=CARTESIAN_POINT('Ctrl Pts',(-2.19254165056297,2.36200129390854,30.7724859431582));
#20330=CARTESIAN_POINT('Ctrl Pts',(-2.21809670025177,2.33808564810473,30.774656278314));
#20331=CARTESIAN_POINT('Ctrl Pts',(-2.23393831657579,2.32295437514376,30.7760216992005));
#20332=CARTESIAN_POINT('Ctrl Pts',(-2.36707820650148,2.19316302346191,30.7876708219113));
#20333=CARTESIAN_POINT('Ctrl Pts',(-2.47560092440002,2.06988130496887,30.7983426108006));
#20334=CARTESIAN_POINT('Ctrl Pts',(-2.72720752968395,1.73582465102214,30.8262370123137));
#20335=CARTESIAN_POINT('Ctrl Pts',(-2.85558399503191,1.5153822753524,30.8437860602046));
#20336=CARTESIAN_POINT('Ctrl Pts',(-2.97899039845763,1.23079918560959,30.864074536397));
#20337=CARTESIAN_POINT('Ctrl Pts',(-2.99991858613339,1.17887226070512,30.8676835152072));
#20338=CARTESIAN_POINT('Ctrl Pts',(-3.0235566542196,1.11550815050646,30.8719541333152));
#20339=CARTESIAN_POINT('Ctrl Pts',(-3.02756930238077,1.10457114039206,30.8726865325431));
#20340=CARTESIAN_POINT('Ctrl Pts',(-3.03372841488643,1.08749791715335,30.8738222157482));
#20341=CARTESIAN_POINT('Ctrl Pts',(-3.03591572071721,1.08137669365312,30.8742278682005));
#20342=CARTESIAN_POINT('Ctrl Pts',(-3.03994675504478,1.06998712258704,30.8749797723577));
#20343=CARTESIAN_POINT('Ctrl Pts',(-3.04179529959364,1.06472065448502,30.8753263003351));
#20344=CARTESIAN_POINT('Ctrl Pts',(-3.04595766561037,1.0527628353469,30.8761105338018));
#20345=CARTESIAN_POINT('Ctrl Pts',(-3.04826311948865,1.04606866161011,30.8765477394076));
#20346=CARTESIAN_POINT('Ctrl Pts',(-3.05504639134056,1.02615972766939,30.8778427686254));
#20347=CARTESIAN_POINT('Ctrl Pts',(-3.05946054002329,1.01292322527341,30.8786969158437));
#20348=CARTESIAN_POINT('Ctrl Pts',(-3.09256877316825,0.911451912199076,
30.8851954861471));
#20349=CARTESIAN_POINT('Ctrl Pts',(-3.11752924805369,0.822034712855346,
30.8906378634238));
#20350=CARTESIAN_POINT('Ctrl Pts',(-3.19350514445047,0.496119742796025,
30.9098710069783));
#20351=CARTESIAN_POINT('Ctrl Pts',(-3.22172690357942,0.255143882280493,
30.9230220295249));
#20352=CARTESIAN_POINT('Ctrl Pts',(-3.22310147156134,-0.0787385245298545,
30.9420296622394));
#20353=CARTESIAN_POINT('Ctrl Pts',(-3.21954004625433,-0.170712646760827,
30.9473400942806));
#20354=CARTESIAN_POINT('Ctrl Pts',(-3.20747926518954,-0.318347104908386,
30.9560744787626));
#20355=CARTESIAN_POINT('Ctrl Pts',(-3.20144853731525,-0.374158791742361,
30.9594247757065));
#20356=CARTESIAN_POINT('Ctrl Pts',(-3.19167323932266,-0.446804782395326,
30.9638604091472));
#20357=CARTESIAN_POINT('Ctrl Pts',(-3.18924664304082,-0.463808594428457,
30.9649039915441));
#20358=CARTESIAN_POINT('Ctrl Pts',(-3.18506572742602,-0.491519661958937,
30.9666137880989));
#20359=CARTESIAN_POINT('Ctrl Pts',(-3.18339303508522,-0.502239032468734,
30.9672774032209));
#20360=CARTESIAN_POINT('Ctrl Pts',(-3.18006209212615,-0.522899829960585,
30.9685608434203));
#20361=CARTESIAN_POINT('Ctrl Pts',(-3.17841126675701,-0.532842338426372,
30.9691804250553));
#20362=CARTESIAN_POINT('Ctrl Pts',(-3.17450915189105,-0.555680273227197,
30.9706081783366));
#20363=CARTESIAN_POINT('Ctrl Pts',(-3.17222588769866,-0.5685699875837,30.9714173614512));
#20364=CARTESIAN_POINT('Ctrl Pts',(-3.16591387550435,-0.602981172921261,
30.9735867589013));
#20365=CARTESIAN_POINT('Ctrl Pts',(-3.16174428036182,-0.624475803688521,
30.9749514479059));
#20366=CARTESIAN_POINT('Ctrl Pts',(-3.12459629645006,-0.806059201737283,
30.9865634144551));
#20367=CARTESIAN_POINT('Ctrl Pts',(-3.07970718062468,-0.963443071882241,
30.9971959220118));
#20368=CARTESIAN_POINT('Ctrl Pts',(-2.93539951244614,-1.35409832722291,
31.0249690537506));
#20369=CARTESIAN_POINT('Ctrl Pts',(-2.82006744379474,-1.5803060287256,31.0424337011622));
#20370=CARTESIAN_POINT('Ctrl Pts',(-2.64747750384873,-1.83855787917176,
31.0627680974446));
#20371=CARTESIAN_POINT('Ctrl Pts',(-2.61420825132768,-1.88556315239567,
31.0664828565777));
#20372=CARTESIAN_POINT('Ctrl Pts',(-2.57265509806996,-1.94105673855285,
31.0708612041755));
#20373=CARTESIAN_POINT('Ctrl Pts',(-2.56556368168135,-1.95042008838233,
31.0715996962196));
#20374=CARTESIAN_POINT('Ctrl Pts',(-2.55445566390821,-1.96492146101508,
31.0727427468899));
#20375=CARTESIAN_POINT('Ctrl Pts',(-2.55047447660281,-1.97008630085497,
31.0731497229313));
#20376=CARTESIAN_POINT('Ctrl Pts',(-2.54305795604091,-1.97964767684539,
31.0739028266103));
#20377=CARTESIAN_POINT('Ctrl Pts',(-2.53962691434688,-1.98404733534443,
31.0742492383984));
#20378=CARTESIAN_POINT('Ctrl Pts',(-2.5318335601699,-1.9939874901052,31.0750316182666));
#20379=CARTESIAN_POINT('Ctrl Pts',(-2.52746448968699,-1.99952257869295,
31.0754670963315));
#20380=CARTESIAN_POINT('Ctrl Pts',(-2.51447923929541,-2.01586276893567,
31.0767522809537));
#20381=CARTESIAN_POINT('Ctrl Pts',(-2.50581155714943,-2.02662700168541,
31.0775983934848));
#20382=CARTESIAN_POINT('Ctrl Pts',(-2.44086039385233,-2.10623486132251,
31.0838548882697));
#20383=CARTESIAN_POINT('Ctrl Pts',(-2.38181284063194,-2.17278518222201,
31.0890798469625));
#20384=CARTESIAN_POINT('Ctrl Pts',(-2.14880108849659,-2.41447114586384,
31.1084105179707));
#20385=CARTESIAN_POINT('Ctrl Pts',(-1.95767567534258,-2.57187430493659,
31.1218136658013));
#20386=CARTESIAN_POINT('Ctrl Pts',(-1.67365375859619,-2.75560626005268,
31.1410757937894));
#20387=CARTESIAN_POINT('Ctrl Pts',(-1.5947847966252,-2.80198899188276,31.1463560636249));
#20388=CARTESIAN_POINT('Ctrl Pts',(-1.50116695529643,-2.85181143492072,
31.1526101846239));
#20389=CARTESIAN_POINT('Ctrl Pts',(-1.48823366213642,-2.85858202895638,
31.1534738563823));
#20390=CARTESIAN_POINT('Ctrl Pts',(-1.47525540353836,-2.86526422112008,
31.1543403726568));
#20391=CARTESIAN_POINT('Origin',(0.,0.,4.68922655072688));
#20392=CARTESIAN_POINT('',(-1.47525540501496,-2.86526422035982,32.6506479065737));
#20393=CARTESIAN_POINT('',(-1.47525529429555,-2.86526427736657,32.4060211118892));
#20394=CARTESIAN_POINT('',(-1.47525540501186,-2.86526422036142,4.68922655072688));
#20395=CARTESIAN_POINT('',(3.22274870594889,0.00297136373924148,31.8105144221227));
#20396=CARTESIAN_POINT('Ctrl Pts',(-1.47525540501479,-2.8652642203599,32.6506479065737));
#20397=CARTESIAN_POINT('Ctrl Pts',(-1.48291685166428,-2.86131952635942,
32.6501042669168));
#20398=CARTESIAN_POINT('Ctrl Pts',(-1.49056256546604,-2.85734405767437,
32.6495624097806));
#20399=CARTESIAN_POINT('Ctrl Pts',(-1.50444135845292,-2.85005676738993,
32.6485801507047));
#20400=CARTESIAN_POINT('Ctrl Pts',(-1.51067963242588,-2.84675507003948,
32.6481391379674));
#20401=CARTESIAN_POINT('Ctrl Pts',(-1.52183173724427,-2.84080567452559,
32.6473517013386));
#20402=CARTESIAN_POINT('Ctrl Pts',(-1.52674956358572,-2.83816569081889,
32.647004798786));
#20403=CARTESIAN_POINT('Ctrl Pts',(-1.53739765880858,-2.83241390308338,
32.6462544291026));
#20404=CARTESIAN_POINT('Ctrl Pts',(-1.54312533261345,-2.82929749042332,
32.6458512616093));
#20405=CARTESIAN_POINT('Ctrl Pts',(-1.55913576696437,-2.82052317263687,
32.6447254774036));
#20406=CARTESIAN_POINT('Ctrl Pts',(-1.56939726116582,-2.81482638074299,
32.6440053019387));
#20407=CARTESIAN_POINT('Ctrl Pts',(-1.62963732957346,-2.78095155615464,
32.6397842235566));
#20408=CARTESIAN_POINT('Ctrl Pts',(-1.67889080003837,-2.75149704841219,
32.6363602620487));
#20409=CARTESIAN_POINT('Ctrl Pts',(-1.94114493311019,-2.58499802795509,
32.6181326975254));
#20410=CARTESIAN_POINT('Ctrl Pts',(-2.13822831928392,-2.42451330176459,
32.6043873635631));
#20411=CARTESIAN_POINT('Ctrl Pts',(-2.4282090504413,-2.12523425899002,32.580846263));
#20412=CARTESIAN_POINT('Ctrl Pts',(-2.53281406830006,-1.99941550664937,
32.5714285732258));
#20413=CARTESIAN_POINT('Ctrl Pts',(-2.64010319616985,-1.84836475590185,
32.5602847096252));
#20414=CARTESIAN_POINT('Ctrl Pts',(-2.65260220675551,-1.83038210593846,
32.55896077099));
#20415=CARTESIAN_POINT('Ctrl Pts',(-2.67228001905848,-1.80144622911154,
32.5568340718041));
#20416=CARTESIAN_POINT('Ctrl Pts',(-2.67957715277906,-1.79057401159564,
32.5560358091785));
#20417=CARTESIAN_POINT('Ctrl Pts',(-2.69237522670015,-1.77125233915481,
32.5546184564413));
#20418=CARTESIAN_POINT('Ctrl Pts',(-2.6979031846448,-1.76282092480332,32.5540003948706));
#20419=CARTESIAN_POINT('Ctrl Pts',(-2.70929967996856,-1.74525946568782,
32.5527138792752));
#20420=CARTESIAN_POINT('Ctrl Pts',(-2.71516183322567,-1.73612544858693,
32.5520451967824));
#20421=CARTESIAN_POINT('Ctrl Pts',(-2.73018608392119,-1.71245344605958,
32.5503132969058));
#20422=CARTESIAN_POINT('Ctrl Pts',(-2.739278151372,-1.69787162316168,32.5492474979498));
#20423=CARTESIAN_POINT('Ctrl Pts',(-2.77758991251153,-1.63531857714893,
32.5446793247281));
#20424=CARTESIAN_POINT('Ctrl Pts',(-2.80566792003677,-1.58666299280107,
32.5411355065275));
#20425=CARTESIAN_POINT('Ctrl Pts',(-2.8763871670721,-1.45636361290657,32.5316635861376));
#20426=CARTESIAN_POINT('Ctrl Pts',(-2.91682248917228,-1.37358732552068,
32.5256635630037));
#20427=CARTESIAN_POINT('Ctrl Pts',(-3.05000621350855,-1.06845308928956,
32.5036370978224));
#20428=CARTESIAN_POINT('Ctrl Pts',(-3.12129772791029,-0.837625034367631,
32.4870761631634));
#20429=CARTESIAN_POINT('Ctrl Pts',(-3.18366981582592,-0.509046704729985,
32.4648125038878));
#20430=CARTESIAN_POINT('Ctrl Pts',(-3.19711491829628,-0.416343384846984,
32.458680632028));
#20431=CARTESIAN_POINT('Ctrl Pts',(-3.20790715398496,-0.30926490388749,
32.45186333026));
#20432=CARTESIAN_POINT('Ctrl Pts',(-3.20921884682066,-0.295343019639964,
32.450982120647));
#20433=CARTESIAN_POINT('Ctrl Pts',(-3.21105882877317,-0.274351960802021,
32.4496616529361));
#20434=CARTESIAN_POINT('Ctrl Pts',(-3.2116544574235,-0.267289073160047,
32.4492187503789));
#20435=CARTESIAN_POINT('Ctrl Pts',(-3.21267766233792,-0.254658555870999,
32.4484292768727));
#20436=CARTESIAN_POINT('Ctrl Pts',(-3.21311407302239,-0.24909174513666,
32.4480822166881));
#20437=CARTESIAN_POINT('Ctrl Pts',(-3.21402709001161,-0.237043582791671,
32.4473330250569));
#20438=CARTESIAN_POINT('Ctrl Pts',(-3.21449855988002,-0.23056193476432,
32.4469311850621));
#20439=CARTESIAN_POINT('Ctrl Pts',(-3.21575950149652,-0.212470691377941,
32.4458128519063));
#20440=CARTESIAN_POINT('Ctrl Pts',(-3.21650571625871,-0.200858042067644,
32.4450987480883));
#20441=CARTESIAN_POINT('Ctrl Pts',(-3.22046029516785,-0.133628419595537,
32.4409849189462));
#20442=CARTESIAN_POINT('Ctrl Pts',(-3.22228923452116,-0.0779360269604391,
32.4376576457728));
#20443=CARTESIAN_POINT('Ctrl Pts',(-3.22442804807954,0.232260052644628,
32.4194356922017));
#20444=CARTESIAN_POINT('Ctrl Pts',(-3.19603478523003,0.486076309874904,
32.4056265872412));
#20445=CARTESIAN_POINT('Ctrl Pts',(-3.10071736806259,0.893626156200001,
32.3819858711514));
#20446=CARTESIAN_POINT('Ctrl Pts',(-3.05123667663764,1.05021911223644,32.3725354479807));
#20447=CARTESIAN_POINT('Ctrl Pts',(-2.98188533857926,1.22268455073457,32.3613549695967));
#20448=CARTESIAN_POINT('Ctrl Pts',(-2.97350350116868,1.24292983521008,32.3600303154276));
#20449=CARTESIAN_POINT('Ctrl Pts',(-2.95978271976823,1.27513738871831,32.3579026839672));
#20450=CARTESIAN_POINT('Ctrl Pts',(-2.95457606746857,1.2871555313712,32.3571042109099));
#20451=CARTESIAN_POINT('Ctrl Pts',(-2.94523190351983,1.30836854741294,32.3556866146746));
#20452=CARTESIAN_POINT('Ctrl Pts',(-2.94112420537878,1.31757642140256,32.3550685212166));
#20453=CARTESIAN_POINT('Ctrl Pts',(-2.93250583111739,1.33665435914517,32.3537820690478));
#20454=CARTESIAN_POINT('Ctrl Pts',(-2.92798838154686,1.34652120602452,32.3531134825141));
#20455=CARTESIAN_POINT('Ctrl Pts',(-2.91619181230212,1.3719467678322,32.3513821102763));
#20456=CARTESIAN_POINT('Ctrl Pts',(-2.90883805138723,1.38747028519196,32.3503167459823));
#20457=CARTESIAN_POINT('Ctrl Pts',(-2.87693628750076,1.45344524931114,32.3457529587842));
#20458=CARTESIAN_POINT('Ctrl Pts',(-2.85119836716688,1.50330726322978,32.3422131908309));
#20459=CARTESIAN_POINT('Ctrl Pts',(-2.77988127803945,1.63304366064887,32.3327548438015));
#20460=CARTESIAN_POINT('Ctrl Pts',(-2.732164972664,1.71167857876124,32.3267645997801));
#20461=CARTESIAN_POINT('Ctrl Pts',(-2.54664308495737,1.98984883403533,32.3046452495708));
#20462=CARTESIAN_POINT('Ctrl Pts',(-2.38981749171377,2.17569455868383,32.2879718752486));
#20463=CARTESIAN_POINT('Ctrl Pts',(-2.14653953429876,2.40562101123155,32.2656989340353));
#20464=CARTESIAN_POINT('Ctrl Pts',(-2.07672679368562,2.46614145844884,32.2596536124603));
#20465=CARTESIAN_POINT('Ctrl Pts',(-1.99348738271045,2.53225590744613,32.2529202547534));
#20466=CARTESIAN_POINT('Ctrl Pts',(-1.98251412065642,2.54085609662356,32.2520417031501));
#20467=CARTESIAN_POINT('Ctrl Pts',(-1.96588527119318,2.55371548435117,32.2507244303169));
#20468=CARTESIAN_POINT('Ctrl Pts',(-1.96027106154988,2.55802756866145,32.2502820901424));
#20469=CARTESIAN_POINT('Ctrl Pts',(-1.95020358792304,2.56570744631809,32.2494932238978));
#20470=CARTESIAN_POINT('Ctrl Pts',(-1.94575575393921,2.56908218670173,32.2491462117374));
#20471=CARTESIAN_POINT('Ctrl Pts',(-1.93610658207787,2.57636394594035,32.2483966746265));
#20472=CARTESIAN_POINT('Ctrl Pts',(-1.93090219386008,2.58026676888646,32.2479944435444));
#20473=CARTESIAN_POINT('Ctrl Pts',(-1.91633178574284,2.59112449336481,32.2468739168112));
#20474=CARTESIAN_POINT('Ctrl Pts',(-1.90693965508675,2.59804442123703,32.246158025731));
#20475=CARTESIAN_POINT('Ctrl Pts',(-1.85208969634267,2.63799904999241,32.242013000598));
#20476=CARTESIAN_POINT('Ctrl Pts',(-1.80580858729125,2.66989353088683,32.2386576097807));
#20477=CARTESIAN_POINT('Ctrl Pts',(-1.54576415520346,2.83924476229148,32.2204342929575));
#20478=CARTESIAN_POINT('Ctrl Pts',(-1.31713942681308,2.95226500538679,32.2066439313556));
#20479=CARTESIAN_POINT('Ctrl Pts',(-0.923183504161726,3.0920368868483,32.1830322379499));
#20480=CARTESIAN_POINT('Ctrl Pts',(-0.764844786626363,3.13495803900215,
32.1735911528506));
#20481=CARTESIAN_POINT('Ctrl Pts',(-0.582422252100943,3.16976053568869,
32.1624211209254));
#20482=CARTESIAN_POINT('Ctrl Pts',(-0.560861262169621,3.17364650546416,
32.1610966704355));
#20483=CARTESIAN_POINT('Ctrl Pts',(-0.526350821919155,3.17950371827202,
32.1589693043467));
#20484=CARTESIAN_POINT('Ctrl Pts',(-0.513425830534473,3.18161641164266,
32.1581708911856));
#20485=CARTESIAN_POINT('Ctrl Pts',(-0.490528346930976,3.18521603020549,
32.1567533642627));
#20486=CARTESIAN_POINT('Ctrl Pts',(-0.480561023402479,3.18673505603114,
32.1561352798853));
#20487=CARTESIAN_POINT('Ctrl Pts',(-0.459850850816696,3.18979192578056,
32.1548488096849));
#20488=CARTESIAN_POINT('Ctrl Pts',(-0.449107047726601,3.19132232622173,
32.1541801958554));
#20489=CARTESIAN_POINT('Ctrl Pts',(-0.421336279817834,3.19513511871768,
32.1524486735259));
#20490=CARTESIAN_POINT('Ctrl Pts',(-0.404298596104516,3.19733565868851,
32.1513831855879));
#20491=CARTESIAN_POINT('Ctrl Pts',(-0.33259650445973,3.20601423419007,32.1468852620894));
#20492=CARTESIAN_POINT('Ctrl Pts',(-0.277791051929911,3.21122706031571,
32.1434131902558));
#20493=CARTESIAN_POINT('Ctrl Pts',(-0.133116213764621,3.22125661575129,
32.1341522968375));
#20494=CARTESIAN_POINT('Ctrl Pts',(-0.0431368919750242,3.22371694527691,
32.1282949313381));
#20495=CARTESIAN_POINT('Ctrl Pts',(0.300614868560171,3.2187222732619,32.105573491936));
#20496=CARTESIAN_POINT('Ctrl Pts',(0.553055718134541,3.18506744055155,32.0880851896187));
#20497=CARTESIAN_POINT('Ctrl Pts',(0.812424153067238,3.11869826125232,32.0703246460258));
#20498=CARTESIAN_POINT('Ctrl Pts',(0.825905350060756,3.11515524676999,32.069402395148));
#20499=CARTESIAN_POINT('Ctrl Pts',(0.908409492889777,3.09289897274025,32.0637653167548));
#20500=CARTESIAN_POINT('Ctrl Pts',(0.976822732889488,3.07197834679629,32.0591209523462));
#20501=CARTESIAN_POINT('Ctrl Pts',(1.05575794869457,3.04493589773411,32.0538414071602));
#20502=CARTESIAN_POINT('Ctrl Pts',(1.06700606105942,3.04101258523069,32.0530909933535));
#20503=CARTESIAN_POINT('Ctrl Pts',(1.08502274271987,3.03461614234726,32.0518923838326));
#20504=CARTESIAN_POINT('Ctrl Pts',(1.09180509595619,3.03218256680718,32.051441938148));
#20505=CARTESIAN_POINT('Ctrl Pts',(1.1038511843549,3.02781465286966,32.0506433469181));
#20506=CARTESIAN_POINT('Ctrl Pts',(1.10911809454526,3.02588930126551,32.0502946736556));
#20507=CARTESIAN_POINT('Ctrl Pts',(1.12033226315809,3.02175667825614,32.0495533624632));
#20508=CARTESIAN_POINT('Ctrl Pts',(1.12627802443907,3.01954559756382,32.0491609561795));
#20509=CARTESIAN_POINT('Ctrl Pts',(1.14224573251456,3.01355387867224,32.0481087419447));
#20510=CARTESIAN_POINT('Ctrl Pts',(1.15225552809678,3.00974076934065,32.0474508492471));
#20511=CARTESIAN_POINT('Ctrl Pts',(1.20251027283317,2.99030937682275,32.0441556224705));
#20512=CARTESIAN_POINT('Ctrl Pts',(1.24245968629992,2.97393266175769,32.0415612190032));
#20513=CARTESIAN_POINT('Ctrl Pts',(1.358337920506,2.92368706619062,32.034076058665));
#20514=CARTESIAN_POINT('Ctrl Pts',(1.43330317111045,2.88767587363463,32.0292847309871));
#20515=CARTESIAN_POINT('Ctrl Pts',(1.66073380245944,2.76738265637367,32.0146630105339));
#20516=CARTESIAN_POINT('Ctrl Pts',(1.80782125190431,2.67361727356417,32.0050688274867));
#20517=CARTESIAN_POINT('Ctrl Pts',(2.08587570415357,2.4628790620077,31.9854123896935));
#20518=CARTESIAN_POINT('Ctrl Pts',(2.21630260841923,2.34619722437109,31.9753777585279));
#20519=CARTESIAN_POINT('Ctrl Pts',(2.35184971830429,2.20349934428614,31.9635420559775));
#20520=CARTESIAN_POINT('Ctrl Pts',(2.36691201604515,2.18731203278201,31.9622055180295));
#20521=CARTESIAN_POINT('Ctrl Pts',(2.39066840783102,2.16124852720196,31.9600624081833));
#20522=CARTESIAN_POINT('Ctrl Pts',(2.39947082140512,2.15147168275718,31.9592604459019));
#20523=CARTESIAN_POINT('Ctrl Pts',(2.41491941238188,2.13410019412087,31.9578388059321));
#20524=CARTESIAN_POINT('Ctrl Pts',(2.42159027873963,2.12652766854324,31.9572201775346));
#20525=CARTESIAN_POINT('Ctrl Pts',(2.43534402894336,2.11076626999908,31.9559347463029));
#20526=CARTESIAN_POINT('Ctrl Pts',(2.44242142475973,2.10257279663996,31.9552677262408));
#20527=CARTESIAN_POINT('Ctrl Pts',(2.46054668406639,2.08137424878591,31.9535449721046));
#20528=CARTESIAN_POINT('Ctrl Pts',(2.47153267709984,2.06831693798482,31.9524867079808));
#20529=CARTESIAN_POINT('Ctrl Pts',(2.51670714489029,2.01375134489924,31.9480756228174));
#20530=CARTESIAN_POINT('Ctrl Pts',(2.54995608343093,1.97147983560572,31.9446851104949));
#20531=CARTESIAN_POINT('Ctrl Pts',(2.66122441568723,1.82249124422599,31.9328182695657));
#20532=CARTESIAN_POINT('Ctrl Pts',(2.73371871044321,1.71183075866648,31.9241401991683));
#20533=CARTESIAN_POINT('Ctrl Pts',(2.85280109727604,1.50310984478794,31.9080764178577));
#20534=CARTESIAN_POINT('Ctrl Pts',(2.90162968875457,1.40654076892554,31.9007542135455));
#20535=CARTESIAN_POINT('Ctrl Pts',(3.0217968900951,1.13587268191479,31.880708316817));
#20536=CARTESIAN_POINT('Ctrl Pts',(3.08291080104405,0.957674669974966,31.8680121563428));
#20537=CARTESIAN_POINT('Ctrl Pts',(3.13166055473726,0.760942752618961,31.8551660512304));
#20538=CARTESIAN_POINT('Ctrl Pts',(3.13508355637754,0.74671468209955,31.854243537446));
#20539=CARTESIAN_POINT('Ctrl Pts',(3.14002863266406,0.725526356139643,31.8528799559708));
#20540=CARTESIAN_POINT('Ctrl Pts',(3.14162467860461,0.718583807569237,31.8524347920099));
#20541=CARTESIAN_POINT('Ctrl Pts',(3.1444313686651,0.706187045110335,31.8516428673776));
#20542=CARTESIAN_POINT('Ctrl Pts',(3.14565085889075,0.700734935988452,31.8512956048356));
#20543=CARTESIAN_POINT('Ctrl Pts',(3.14825276542802,0.688958628620088,31.8505477601554));
#20544=CARTESIAN_POINT('Ctrl Pts',(3.14963030308985,0.682633446716022,31.8501474599121));
#20545=CARTESIAN_POINT('Ctrl Pts',(3.15242455401594,0.669614667962316,31.8493262901574));
#20546=CARTESIAN_POINT('Ctrl Pts',(3.15383903013294,0.662920618405464,31.8489055482326));
#20547=CARTESIAN_POINT('Ctrl Pts',(3.15738542756784,0.645868909381281,31.847837469423));
#20548=CARTESIAN_POINT('Ctrl Pts',(3.15948772584706,0.635505077497406,31.8471917491857));
#20549=CARTESIAN_POINT('Ctrl Pts',(3.16541355592326,0.605535766752645,31.8453339588908));
#20550=CARTESIAN_POINT('Ctrl Pts',(3.16910595080587,0.585904480663125,31.8441286821797));
#20551=CARTESIAN_POINT('Ctrl Pts',(3.20579579446999,0.380332896570112,31.8316171952126));
#20552=CARTESIAN_POINT('Ctrl Pts',(3.22257452653606,0.191850745334481,31.8210686942788));
#20553=CARTESIAN_POINT('Ctrl Pts',(3.22274863087502,0.00297063851481531,
31.8105142503188));
#20554=CARTESIAN_POINT('Ctrl Pts',(3.22274863019977,0.00297137098221913,
31.8105142912484));
#20555=CARTESIAN_POINT('Ctrl Pts',(3.22294655442589,-0.211697222216134,
31.7985188106586));
#20556=CARTESIAN_POINT('Ctrl Pts',(3.2016966095535,-0.425834942704719,31.7865487754178));
#20557=CARTESIAN_POINT('Ctrl Pts',(3.15179628169263,-0.67360854883105,31.7716561250349));
#20558=CARTESIAN_POINT('Ctrl Pts',(3.14361538969645,-0.71080966747438,31.7693932376667));
#20559=CARTESIAN_POINT('Ctrl Pts',(3.13016127318282,-0.767205098686855,
31.7659172523452));
#20560=CARTESIAN_POINT('Ctrl Pts',(3.12536623256774,-0.786510740601612,
31.7647191473432));
#20561=CARTESIAN_POINT('Ctrl Pts',(3.11612273591884,-0.822306718833107,
31.7624817651706));
#20562=CARTESIAN_POINT('Ctrl Pts',(3.1117213005569,-0.838808545103621,31.7614440228271));
#20563=CARTESIAN_POINT('Ctrl Pts',(3.10431479167114,-0.86571619452275,31.7597412387505));
#20564=CARTESIAN_POINT('Ctrl Pts',(3.10138801985981,-0.876143367827872,
31.759078753382));
#20565=CARTESIAN_POINT('Ctrl Pts',(3.09563292462377,-0.896256759208142,
31.7577956929485));
#20566=CARTESIAN_POINT('Ctrl Pts',(3.09281155450412,-0.905944847697968,
31.7571753518048));
#20567=CARTESIAN_POINT('Ctrl Pts',(3.08620925219622,-0.928225664958481,
31.7557432476211));
#20568=CARTESIAN_POINT('Ctrl Pts',(3.08239668162054,-0.940808759699964,
31.7549304545748));
#20569=CARTESIAN_POINT('Ctrl Pts',(3.07197399351923,-0.974464515102667,
31.7527455582349));
#20570=CARTESIAN_POINT('Ctrl Pts',(3.06522417562286,-0.995492853822492,
31.7513688810894));
#20571=CARTESIAN_POINT('Ctrl Pts',(2.98786019161372,-1.22826293802806,31.7359988258656));
#20572=CARTESIAN_POINT('Ctrl Pts',(2.8956613494858,-1.43214815950187,31.721261031844));
#20573=CARTESIAN_POINT('Ctrl Pts',(2.72883652109949,-1.71790006338102,31.6989330237154));
#20574=CARTESIAN_POINT('Ctrl Pts',(2.66987420867143,-1.80817617550761,31.6916127097813));
#20575=CARTESIAN_POINT('Ctrl Pts',(2.53399560215951,-1.99503961220759,31.6760524739148));
#20576=CARTESIAN_POINT('Ctrl Pts',(2.45582078760895,-2.09051841347114,31.6678439800124));
#20577=CARTESIAN_POINT('Ctrl Pts',(2.35564755857946,-2.19946624834774,31.6583674354191));
#20578=CARTESIAN_POINT('Ctrl Pts',(2.33872687586444,-2.217449860821,31.6567994498702));
#20579=CARTESIAN_POINT('Ctrl Pts',(2.31690385102352,-2.24011606033941,31.6548204451901));
#20580=CARTESIAN_POINT('Ctrl Pts',(2.31219170242051,-2.24497949921201,31.654395650719));
#20581=CARTESIAN_POINT('Ctrl Pts',(2.30297950624752,-2.25442769347834,31.6535701493753));
#20582=CARTESIAN_POINT('Ctrl Pts',(2.29848101320443,-2.25901391429292,31.653169327547));
#20583=CARTESIAN_POINT('Ctrl Pts',(2.29003997410059,-2.26756824987753,31.6524215381755));
#20584=CARTESIAN_POINT('Ctrl Pts',(2.28610085519934,-2.27153950687205,31.6520743241006));
#20585=CARTESIAN_POINT('Ctrl Pts',(2.27706998687222,-2.28059677025413,31.6512822625145));
#20586=CARTESIAN_POINT('Ctrl Pts',(2.27197153662212,-2.28567598157656,31.6508379548484));
#20587=CARTESIAN_POINT('Ctrl Pts',(2.25619032144485,-2.30129266981563,31.6494713104575));
#20588=CARTESIAN_POINT('Ctrl Pts',(2.2454507632227,-2.31177282812969,31.6485533764769));
#20589=CARTESIAN_POINT('Ctrl Pts',(2.1335791968284,-2.41942714647603,31.6391108323562));
#20590=CARTESIAN_POINT('Ctrl Pts',(2.02626580448385,-2.5099890502429,31.6310512680974));
#20591=CARTESIAN_POINT('Ctrl Pts',(1.73639877619137,-2.7238594319444,31.6107127573063));
#20592=CARTESIAN_POINT('Ctrl Pts',(1.5465211439489,-2.83597668525063,31.5986561905489));
#20593=CARTESIAN_POINT('Ctrl Pts',(1.24375160228321,-2.97523799235726,31.5795137198177));
#20594=CARTESIAN_POINT('Ctrl Pts',(1.13838318882406,-3.01712424606775,31.5728742948988));
#20595=CARTESIAN_POINT('Ctrl Pts',(1.01145877586732,-3.05998295056648,31.56479783105));
#20596=CARTESIAN_POINT('Ctrl Pts',(0.991819204731621,-3.066404922301,31.563546083599));
#20597=CARTESIAN_POINT('Ctrl Pts',(0.960688594364407,-3.07625400998359,
31.5615581660108));
#20598=CARTESIAN_POINT('Ctrl Pts',(0.949237637500321,-3.07980668398456,
31.5608261371693));
#20599=CARTESIAN_POINT('Ctrl Pts',(0.928339535615406,-3.0861627262168,31.5594886097369));
#20600=CARTESIAN_POINT('Ctrl Pts',(0.918898810472238,-3.08898683046013,
31.5588838009211));
#20601=CARTESIAN_POINT('Ctrl Pts',(0.898281742825715,-3.09505135380699,
31.5575616628602));
#20602=CARTESIAN_POINT('Ctrl Pts',(0.887100537242835,-3.09827461715767,
31.5568437813052));
#20603=CARTESIAN_POINT('Ctrl Pts',(0.856476170187395,-3.10692349498022,
31.5548751231888));
#20604=CARTESIAN_POINT('Ctrl Pts',(0.836999354375975,-3.11222702973482,
31.5536203888655));
#20605=CARTESIAN_POINT('Ctrl Pts',(0.738362382420617,-3.13809299553197,
31.5472515022911));
#20606=CARTESIAN_POINT('Ctrl Pts',(0.658495765406616,-3.15581812446404,
31.5420464654003));
#20607=CARTESIAN_POINT('Ctrl Pts',(0.554484208805832,-3.17478164349647,
31.5352012997161));
#20608=CARTESIAN_POINT('Ctrl Pts',(0.530874763144241,-3.17881474184123,
31.5336432337452));
#20609=CARTESIAN_POINT('Ctrl Pts',(0.252787149857518,-3.22313483687704,
31.5152425679041));
#20610=CARTESIAN_POINT('Ctrl Pts',(-0.00557936023520656,-3.23302320659039,
31.4975601948538));
#20611=CARTESIAN_POINT('Ctrl Pts',(-0.339963207176285,-3.20571553381336,
31.4750931836018));
#20612=CARTESIAN_POINT('Ctrl Pts',(-0.41736182553296,-3.19656031329922,
31.4699312181219));
#20613=CARTESIAN_POINT('Ctrl Pts',(-0.53516792649685,-3.17827287853875,
31.4622025396388));
#20614=CARTESIAN_POINT('Ctrl Pts',(-0.57585529802097,-3.17115345868604,
31.4595570325029));
#20615=CARTESIAN_POINT('Ctrl Pts',(-0.626774243737929,-3.16123130933243,
31.4562855962421));
#20616=CARTESIAN_POINT('Ctrl Pts',(-0.637141878815733,-3.15915804880541,
31.4556215584571));
#20617=CARTESIAN_POINT('Ctrl Pts',(-0.653682858163162,-3.1557655376065,
31.4545656239615));
#20618=CARTESIAN_POINT('Ctrl Pts',(-0.659862747861199,-3.15447912705302,
31.4541718974085));
#20619=CARTESIAN_POINT('Ctrl Pts',(-0.671532218276745,-3.15201420768962,
31.4534299552215));
#20620=CARTESIAN_POINT('Ctrl Pts',(-0.677022429572355,-3.15083952558238,
31.4530815367481));
#20621=CARTESIAN_POINT('Ctrl Pts',(-0.689603751460724,-3.14811323138528,
31.45228455325));
#20622=CARTESIAN_POINT('Ctrl Pts',(-0.696692703623661,-3.14655200668855,
31.4518365450466));
#20623=CARTESIAN_POINT('Ctrl Pts',(-0.715577525245787,-3.14232598697329,
31.4506457217876));
#20624=CARTESIAN_POINT('Ctrl Pts',(-0.727363905694022,-3.13961869697579,
31.4499052787004));
#20625=CARTESIAN_POINT('Ctrl Pts',(-0.812425515832031,-3.11957562500354,
31.4445797656049));
#20626=CARTESIAN_POINT('Ctrl Pts',(-0.885094839887949,-3.09974134431951,
31.4401278429332));
#20627=CARTESIAN_POINT('Ctrl Pts',(-1.00402594848297,-3.06275593034443,
31.4329043418943));
#20628=CARTESIAN_POINT('Ctrl Pts',(-1.05070383265645,-3.04705821908434,
31.4300856262903));
#20629=CARTESIAN_POINT('Ctrl Pts',(-1.22655498250397,-2.98339790531444,
31.4194672774839));
#20630=CARTESIAN_POINT('Ctrl Pts',(-1.35289316253756,-2.9282656021495,31.4118344611414));
#20631=CARTESIAN_POINT('Ctrl Pts',(-1.47525569888183,-2.86526406905484,
31.4041249682223));
#20632=CARTESIAN_POINT('Ctrl Pts',(-1.47525540353836,-2.86526422112008,
31.1543403726568));
#20633=CARTESIAN_POINT('Ctrl Pts',(-1.4385464654136,-2.88416476750862,31.1567913095114));
#20634=CARTESIAN_POINT('Ctrl Pts',(-1.40147779098518,-2.90235806517172,
31.1592650689877));
#20635=CARTESIAN_POINT('Ctrl Pts',(-1.34853185279998,-2.92709301561504,
31.1628014532052));
#20636=CARTESIAN_POINT('Ctrl Pts',(-1.33293650732094,-2.93422765474034,
31.1638434624792));
#20637=CARTESIAN_POINT('Ctrl Pts',(-1.30738902028689,-2.94566954875886,
31.1655513290561));
#20638=CARTESIAN_POINT('Ctrl Pts',(-1.29747064165849,-2.9500517063844,31.1662145986323));
#20639=CARTESIAN_POINT('Ctrl Pts',(-1.27828912902419,-2.95841107465922,
31.1674978258099));
#20640=CARTESIAN_POINT('Ctrl Pts',(-1.26902906603944,-2.96239504622687,
31.1681175424174));
#20641=CARTESIAN_POINT('Ctrl Pts',(-1.24768941140512,-2.97145762254765,
31.1695462600095));
#20642=CARTESIAN_POINT('Ctrl Pts',(-1.23559729415399,-2.97650610421951,
31.1703562769307));
#20643=CARTESIAN_POINT('Ctrl Pts',(-1.20317665311436,-2.98981017834674,
31.172529364861));
#20644=CARTESIAN_POINT('Ctrl Pts',(-1.18279432534424,-2.99793203835976,
31.1738969344998));
#20645=CARTESIAN_POINT('Ctrl Pts',(-1.00773512017665,-3.06562573231448,
31.1856564167914));
#20646=CARTESIAN_POINT('Ctrl Pts',(-0.848782439136819,-3.11338150543386,
31.1964449722444));
#20647=CARTESIAN_POINT('Ctrl Pts',(-0.434395662077885,-3.20377934986971,
31.2247473238573));
#20648=CARTESIAN_POINT('Ctrl Pts',(-0.176211266408086,-3.22828864967506,
31.2425983151369));
#20649=CARTESIAN_POINT('Ctrl Pts',(0.132728582943767,-3.22041351035558,
31.2627493596028));
#20650=CARTESIAN_POINT('Ctrl Pts',(0.183299244577456,-3.21793134201322,
31.2660056624235));
#20651=CARTESIAN_POINT('Ctrl Pts',(0.245067901590247,-3.21343851158656,
31.2699146502115));
#20652=CARTESIAN_POINT('Ctrl Pts',(0.256337977231287,-3.21255913479016,
31.2706250753855));
#20653=CARTESIAN_POINT('Ctrl Pts',(0.274005718662339,-3.21108699711769,
31.2717341563601));
#20654=CARTESIAN_POINT('Ctrl Pts',(0.280406506083703,-3.21053438386452,
31.2721350076566));
#20655=CARTESIAN_POINT('Ctrl Pts',(0.29237468242913,-3.20946504407314,31.2728826793606));
#20656=CARTESIAN_POINT('Ctrl Pts',(0.297942316656516,-3.20895297575298,
31.2732297471742));
#20657=CARTESIAN_POINT('Ctrl Pts',(0.31066653726288,-3.20774929785889,31.2740212433305));
#20658=CARTESIAN_POINT('Ctrl Pts',(0.317822147739402,-3.20704822852074,
31.2744651336936));
#20659=CARTESIAN_POINT('Ctrl Pts',(0.339876926421341,-3.20481287643749,
31.2758296904556));
#20660=CARTESIAN_POINT('Ctrl Pts',(0.354768043041343,-3.20319864414155,
31.2767459721483));
#20661=CARTESIAN_POINT('Ctrl Pts',(0.505824072391171,-3.18575749115097,
31.2859943710882));
#20662=CARTESIAN_POINT('Ctrl Pts',(0.640876943737671,-3.16135970489541,
31.2938823933859));
#20663=CARTESIAN_POINT('Ctrl Pts',(1.028700637433,-3.06541128591255,31.3164594356302));
#20664=CARTESIAN_POINT('Ctrl Pts',(1.27475853586173,-2.97152514696446,31.3307709033711));
#20665=CARTESIAN_POINT('Ctrl Pts',(1.57575540490046,-2.81233220896481,31.3506271984647));
#20666=CARTESIAN_POINT('Ctrl Pts',(1.64344145130215,-2.77332224217286,31.3552544523252));
#20667=CARTESIAN_POINT('Ctrl Pts',(1.72592224567952,-2.72170514570515,31.3611313730312));
#20668=CARTESIAN_POINT('Ctrl Pts',(1.74211273117079,-2.71137044784312,31.362296751054));
#20669=CARTESIAN_POINT('Ctrl Pts',(1.76767863291337,-2.69472771757317,31.3641562109556));
#20670=CARTESIAN_POINT('Ctrl Pts',(1.7771150878358,-2.68851393534968,31.3648467605085));
#20671=CARTESIAN_POINT('Ctrl Pts',(1.79481964606716,-2.67672177813273,31.3661504214758));
#20672=CARTESIAN_POINT('Ctrl Pts',(1.80309492706077,-2.67115437964214,31.3667631130432));
#20673=CARTESIAN_POINT('Ctrl Pts',(1.82165525362025,-2.65854191490187,31.3681449219851));
#20674=CARTESIAN_POINT('Ctrl Pts',(1.83192548822038,-2.65147543358933,31.368914848862));
#20675=CARTESIAN_POINT('Ctrl Pts',(1.85803464987177,-2.63328680023688,31.3708859184999));
#20676=CARTESIAN_POINT('Ctrl Pts',(1.87381468587425,-2.62208135439037,31.3720902444273));
#20677=CARTESIAN_POINT('Ctrl Pts',(1.96757747455022,-2.55422149283098,31.3793256191301));
#20678=CARTESIAN_POINT('Ctrl Pts',(2.0430802414395,-2.49423906658596,31.3854857708941));
#20679=CARTESIAN_POINT('Ctrl Pts',(2.30396033408986,-2.26718395342923,31.4080219771351));
#20680=CARTESIAN_POINT('Ctrl Pts',(2.47247462645146,-2.08211338324742,31.4250874709857));
#20681=CARTESIAN_POINT('Ctrl Pts',(2.66988731846174,-1.80713996142825,31.4478408691678));
#20682=CARTESIAN_POINT('Ctrl Pts',(2.71882086717044,-1.73264782152367,31.4537708082675));
#20683=CARTESIAN_POINT('Ctrl Pts',(2.78788242528316,-1.61736830213692,31.4625046006794));
#20684=CARTESIAN_POINT('Ctrl Pts',(2.81033694880198,-1.57802895209662,31.4654108346381));
#20685=CARTESIAN_POINT('Ctrl Pts',(2.83716596401702,-1.5286353388717,31.4689567372364));
#20686=CARTESIAN_POINT('Ctrl Pts',(2.84232719818813,-1.51901705492339,31.4696424499297));
#20687=CARTESIAN_POINT('Ctrl Pts',(2.85040827864743,-1.50377205276406,31.470721560723));
#20688=CARTESIAN_POINT('Ctrl Pts',(2.85336050637855,-1.49816272945965,31.4711169663542));
#20689=CARTESIAN_POINT('Ctrl Pts',(2.85889265290075,-1.48757581080624,31.4718600934118));
#20690=CARTESIAN_POINT('Ctrl Pts',(2.86147610101475,-1.48260025546768,31.4722080288655));
#20691=CARTESIAN_POINT('Ctrl Pts',(2.86735107478382,-1.47121287374998,31.4730013735598));
#20692=CARTESIAN_POINT('Ctrl Pts',(2.87063408080551,-1.46479673758719,31.4734462429657));
#20693=CARTESIAN_POINT('Ctrl Pts',(2.8792905639763,-1.44773807893706,31.4746235092059));
#20694=CARTESIAN_POINT('Ctrl Pts',(2.88462661645523,-1.43707654314635,31.4753536178085));
#20695=CARTESIAN_POINT('Ctrl Pts',(2.92166846062267,-1.36202855789241,31.4804549427931));
#20696=CARTESIAN_POINT('Ctrl Pts',(2.95127750749413,-1.2966229967614,31.4847052830448));
#20697=CARTESIAN_POINT('Ctrl Pts',(2.98840002265576,-1.206744045536,31.4903566161616));
#20698=CARTESIAN_POINT('Ctrl Pts',(2.99784112788908,-1.18309531003444,31.4918262255357));
#20699=CARTESIAN_POINT('Ctrl Pts',(3.0953211307437,-0.930258938984102,31.5073788004879));
#20700=CARTESIAN_POINT('Ctrl Pts',(3.15717797308431,-0.691833870314143,
31.5207207850651));
#20701=CARTESIAN_POINT('Ctrl Pts',(3.20810843219345,-0.329581809502716,
31.5415894227408));
#20702=CARTESIAN_POINT('Ctrl Pts',(3.21817157940083,-0.209644786509443,
31.5485814650545));
#20703=CARTESIAN_POINT('Ctrl Pts',(3.22233468156651,-0.0596859423883815,
31.5575690418416));
#20704=CARTESIAN_POINT('Ctrl Pts',(3.22274842593739,-0.0299283243626218,
31.5593642408183));
#20705=CARTESIAN_POINT('Ctrl Pts',(3.22275069678397,0.013125637980479,31.5619801628055));
#20706=CARTESIAN_POINT('Ctrl Pts',(3.22266912042875,0.0264209749777316,
31.5627905376577));
#20707=CARTESIAN_POINT('Ctrl Pts',(3.22238066351417,0.0498264277796811,
31.564221802491));
#20708=CARTESIAN_POINT('Ctrl Pts',(3.2222084637789,0.0599368479843692,31.5648415949953));
#20709=CARTESIAN_POINT('Ctrl Pts',(3.22175472590328,0.0808079060521612,
31.5661242706762));
#20710=CARTESIAN_POINT('Ctrl Pts',(3.22146685216968,0.0915682665137558,
31.5667873453523));
#20711=CARTESIAN_POINT('Ctrl Pts',(3.22059198451827,0.119108030738224,31.5684890342999));
#20712=CARTESIAN_POINT('Ctrl Pts',(3.21992776934796,0.135884497714904,31.5695300629698));
#20713=CARTESIAN_POINT('Ctrl Pts',(3.21663558675833,0.20530894412162,31.573856787698));
#20714=CARTESIAN_POINT('Ctrl Pts',(3.21284731003834,0.25789124199196,31.5771786793638));
#20715=CARTESIAN_POINT('Ctrl Pts',(3.19965030994605,0.394293153660462,31.5859178210813));
#20716=CARTESIAN_POINT('Ctrl Pts',(3.18823830804634,0.477874151793341,31.5913939256647));
#20717=CARTESIAN_POINT('Ctrl Pts',(3.14445865283243,0.725576076223137,31.60797138609));
#20718=CARTESIAN_POINT('Ctrl Pts',(3.10258378118853,0.887719845045409,31.6192996306446));
#20719=CARTESIAN_POINT('Ctrl Pts',(3.01491037780936,1.14325576822739,31.6375796691943));
#20720=CARTESIAN_POINT('Ctrl Pts',(2.97684767686744,1.23899080969529,31.6445258937912));
#20721=CARTESIAN_POINT('Ctrl Pts',(2.90234166504304,1.40302872606525,31.6564414513898));
#20722=CARTESIAN_POINT('Ctrl Pts',(2.86789988402392,1.47215119937337,31.6614661483235));
#20723=CARTESIAN_POINT('Ctrl Pts',(2.82519005897335,1.55066656982373,31.6671235811861));
#20724=CARTESIAN_POINT('Ctrl Pts',(2.81931389094956,1.56132471810529,31.667890449156));
#20725=CARTESIAN_POINT('Ctrl Pts',(2.80982639210189,1.57830485284822,31.6691101071988));
#20726=CARTESIAN_POINT('Ctrl Pts',(2.80625383981955,1.5846482105625,31.6695652728674));
#20727=CARTESIAN_POINT('Ctrl Pts',(2.79988749849229,1.59586311874077,31.6703690891598));
#20728=CARTESIAN_POINT('Ctrl Pts',(2.79710243476334,1.60073953824306,31.670718293671));
#20729=CARTESIAN_POINT('Ctrl Pts',(2.79116765895107,1.61106806384799,31.6714572524936));
#20730=CARTESIAN_POINT('Ctrl Pts',(2.7880147175561,1.61651821611255,31.6718467932604));
#20731=CARTESIAN_POINT('Ctrl Pts',(2.77944833126341,1.63122639470243,31.6728970701508));
#20732=CARTESIAN_POINT('Ctrl Pts',(2.7740045568614,1.64046679424992,31.6735558669272));
#20733=CARTESIAN_POINT('Ctrl Pts',(2.74655482399039,1.68653329691992,31.6768358705896));
#20734=CARTESIAN_POINT('Ctrl Pts',(2.72386005418996,1.72294654131337,31.6794146908492));
#20735=CARTESIAN_POINT('Ctrl Pts',(2.65565096034204,1.82766827149937,31.6868233460114));
#20736=CARTESIAN_POINT('Ctrl Pts',(2.60824427205007,1.89470764372552,31.6915564897157));
#20737=CARTESIAN_POINT('Ctrl Pts',(2.43181052036207,2.12501657687448,31.7080531236677));
#20738=CARTESIAN_POINT('Ctrl Pts',(2.2895999767914,2.27752815325309,31.7194497364084));
#20739=CARTESIAN_POINT('Ctrl Pts',(2.02606675822561,2.51033633097974,31.7394241746705));
#20740=CARTESIAN_POINT('Ctrl Pts',(1.91223555627755,2.59809210189347,31.7477507939705));
#20741=CARTESIAN_POINT('Ctrl Pts',(1.77513748361164,2.68988170841189,31.7576784157971));
#20742=CARTESIAN_POINT('Ctrl Pts',(1.75721426616615,2.70162445202023,31.7589741839566));
#20743=CARTESIAN_POINT('Ctrl Pts',(1.72827034813277,2.72017774348512,31.761064011697));
#20744=CARTESIAN_POINT('Ctrl Pts',(1.71732316860249,2.72710221283988,31.7618538175989));
#20745=CARTESIAN_POINT('Ctrl Pts',(1.69780236276659,2.73928564734107,31.7632612457228));
#20746=CARTESIAN_POINT('Ctrl Pts',(1.68924525600514,2.74457085573782,31.7638778858263));
#20747=CARTESIAN_POINT('Ctrl Pts',(1.67135380611016,2.7555059548212,31.7651665837162));
#20748=CARTESIAN_POINT('Ctrl Pts',(1.66201524342205,2.76114866282097,31.7658388954553));
#20749=CARTESIAN_POINT('Ctrl Pts',(1.6376618091582,2.77569560493259,31.7675914098761));
#20750=CARTESIAN_POINT('Ctrl Pts',(1.62260307893132,2.7845253673347,31.7686743132924));
#20751=CARTESIAN_POINT('Ctrl Pts',(1.55656196973952,2.82253127977033,31.7734207842086));
#20752=CARTESIAN_POINT('Ctrl Pts',(1.50486175287006,2.85043125926927,31.7771299314323));
#20753=CARTESIAN_POINT('Ctrl Pts',(1.36486941962881,2.92110769792734,31.7871628044619));
#20754=CARTESIAN_POINT('Ctrl Pts',(1.27534328842244,2.96128944846798,31.7935695094477));
#20755=CARTESIAN_POINT('Ctrl Pts',(1.00592154060091,3.06772795527495,31.8127877456447));
#20756=CARTESIAN_POINT('Ctrl Pts',(0.821794032291912,3.12209533876354,31.825866376912));
#20757=CARTESIAN_POINT('Ctrl Pts',(0.504123477055967,3.18582947391031,31.8476665198329));
#20758=CARTESIAN_POINT('Ctrl Pts',(0.372802525880266,3.20385338677006,31.8564568862512));
#20759=CARTESIAN_POINT('Ctrl Pts',(0.225836699110293,3.21486211855393,31.8658009966638));
#20760=CARTESIAN_POINT('Ctrl Pts',(0.210934196695225,3.21587428872627,31.8667428345717));
#20761=CARTESIAN_POINT('Ctrl Pts',(0.188856508110901,3.21721966268327,31.8681292238262));
#20762=CARTESIAN_POINT('Ctrl Pts',(0.181686631686446,3.21763253166805,31.8685780709914));
#20763=CARTESIAN_POINT('Ctrl Pts',(0.168933205012346,3.21832415812376,31.8693739112689));
#20764=CARTESIAN_POINT('Ctrl Pts',(0.163350260748968,3.21861235760456,31.869721427318));
#20765=CARTESIAN_POINT('Ctrl Pts',(0.151344318712029,3.21920080185935,31.8704668622995));
#20766=CARTESIAN_POINT('Ctrl Pts',(0.144921181813532,3.219496351647,31.8708645152377));
#20767=CARTESIAN_POINT('Ctrl Pts',(0.127179279637503,3.22025951193936,31.8719598308866));
#20768=CARTESIAN_POINT('Ctrl Pts',(0.115858737551582,3.2206866744906,31.8726552603862));
#20769=CARTESIAN_POINT('Ctrl Pts',(0.0535859592466406,3.22270767314267,
31.8764628696621));
#20770=CARTESIAN_POINT('Ctrl Pts',(0.0026005191167779,3.22315220177833,
31.879514623337));
#20771=CARTESIAN_POINT('Ctrl Pts',(-0.30644653896629,3.21851252337684,31.8977297161829));
#20772=CARTESIAN_POINT('Ctrl Pts',(-0.563142152439043,3.18365098370623,
31.9117265874135));
#20773=CARTESIAN_POINT('Ctrl Pts',(-0.97323564475835,3.07674618037183,31.9356542255654));
#20774=CARTESIAN_POINT('Ctrl Pts',(-1.13003988695846,3.02267329175473,31.945193963887));
#20775=CARTESIAN_POINT('Ctrl Pts',(-1.30211085083626,2.94806821739571,31.9564741096689));
#20776=CARTESIAN_POINT('Ctrl Pts',(-1.32214932118541,2.93913593056156,31.9578003951808));
#20777=CARTESIAN_POINT('Ctrl Pts',(-1.35400758018509,2.92454316587647,31.9599300105496));
#20778=CARTESIAN_POINT('Ctrl Pts',(-1.36588697026365,2.91901388019633,31.9607288208967));
#20779=CARTESIAN_POINT('Ctrl Pts',(-1.38684524465525,2.90910285995094,31.9621466338735));
#20780=CARTESIAN_POINT('Ctrl Pts',(-1.39593796128396,2.90475065831416,31.9627646040593));
#20781=CARTESIAN_POINT('Ctrl Pts',(-1.41476884922265,2.89562847219811,31.9640504181318));
#20782=CARTESIAN_POINT('Ctrl Pts',(-1.42450365209201,2.89085186170273,31.9647184877937));
#20783=CARTESIAN_POINT('Ctrl Pts',(-1.44957296956339,2.87839363555183,31.9664476998643));
#20784=CARTESIAN_POINT('Ctrl Pts',(-1.4648704512151,2.87063864986549,31.9675114103111));
#20785=CARTESIAN_POINT('Ctrl Pts',(-1.52976180869564,2.83708852395585,31.9720606513543));
#20786=CARTESIAN_POINT('Ctrl Pts',(-1.57873944633834,2.81012875383744,31.9755872074281));
#20787=CARTESIAN_POINT('Ctrl Pts',(-1.70595887772636,2.73572498833287,31.9850019091354));
#20788=CARTESIAN_POINT('Ctrl Pts',(-1.78291999315527,2.68620191243504,31.9909609131953));
#20789=CARTESIAN_POINT('Ctrl Pts',(-2.05925853040386,2.49127153967934,32.0133274329423));
#20790=CARTESIAN_POINT('Ctrl Pts',(-2.24383584015036,2.32640596420908,32.030306753817));
#20791=CARTESIAN_POINT('Ctrl Pts',(-2.46694642894772,2.07562343896931,32.0526134550647));
#20792=CARTESIAN_POINT('Ctrl Pts',(-2.52332550241131,2.00670597860277,32.0584323169291));
#20793=CARTESIAN_POINT('Ctrl Pts',(-2.5850855280914,1.92448471831555,32.0649450697155));
#20794=CARTESIAN_POINT('Ctrl Pts',(-2.59331599054158,1.91337942078905,32.0658160228391));
#20795=CARTESIAN_POINT('Ctrl Pts',(-2.60563741479335,1.89652865979826,32.0671240678157));
#20796=CARTESIAN_POINT('Ctrl Pts',(-2.60978126059345,1.89082232610839,32.067564706639));
#20797=CARTESIAN_POINT('Ctrl Pts',(-2.61716997635998,1.88057704095503,32.0683516309602));
#20798=CARTESIAN_POINT('Ctrl Pts',(-2.62042180798153,1.8760432409532,32.0686983935701));
#20799=CARTESIAN_POINT('Ctrl Pts',(-2.62744857736224,1.86619239491428,32.069448630815));
#20800=CARTESIAN_POINT('Ctrl Pts',(-2.63121914591467,1.86087234636604,32.0698518051053));
#20801=CARTESIAN_POINT('Ctrl Pts',(-2.64173504824622,1.84593916661408,32.0709780254229));
#20802=CARTESIAN_POINT('Ctrl Pts',(-2.64844410444986,1.83630044041457,32.0716986260889));
#20803=CARTESIAN_POINT('Ctrl Pts',(-2.68771429101991,1.77921905537042,32.0759302812312));
#20804=CARTESIAN_POINT('Ctrl Pts',(-2.71905502894969,1.73094461396924,32.0793639337899));
#20805=CARTESIAN_POINT('Ctrl Pts',(-2.8811429292694,1.46600240786322,32.0975864920437));
#20806=CARTESIAN_POINT('Ctrl Pts',(-2.9873285869846,1.23533075697919,32.1113206172386));
#20807=CARTESIAN_POINT('Ctrl Pts',(-3.11588232448205,0.839114198316271,
32.1348517909764));
#20808=CARTESIAN_POINT('Ctrl Pts',(-3.15441968612414,0.680045115225367,
32.1442721065176));
#20809=CARTESIAN_POINT('Ctrl Pts',(-3.1842497645424,0.497142249588672,32.1554186119938));
#20810=CARTESIAN_POINT('Ctrl Pts',(-3.18755381343815,0.475497244479642,
32.1567423090101));
#20811=CARTESIAN_POINT('Ctrl Pts',(-3.19248036675914,0.440860558960777,
32.1588685520131));
#20812=CARTESIAN_POINT('Ctrl Pts',(-3.19424474433226,0.427889506718449,
32.1596666013287));
#20813=CARTESIAN_POINT('Ctrl Pts',(-3.19722759199732,0.404913407159634,
32.1610835334345));
#20814=CARTESIAN_POINT('Ctrl Pts',(-3.19847825210967,0.394912660524777,
32.1617013880439));
#20815=CARTESIAN_POINT('Ctrl Pts',(-3.20097771890057,0.374134879547901,
32.1629874302397));
#20816=CARTESIAN_POINT('Ctrl Pts',(-3.20221905637688,0.363357090697862,
32.1636558459299));
#20817=CARTESIAN_POINT('Ctrl Pts',(-3.20528499900597,0.335500592200841,
32.1653869608449));
#20818=CARTESIAN_POINT('Ctrl Pts',(-3.20702751516114,0.31841336468411,32.1664522388526));
#20819=CARTESIAN_POINT('Ctrl Pts',(-3.2138810478703,0.245431274437439,32.1710172718786));
#20820=CARTESIAN_POINT('Ctrl Pts',(-3.21766771403154,0.189424769271709,
32.1745584075382));
#20821=CARTESIAN_POINT('Ctrl Pts',(-3.22379684662015,0.0414259104642137,
32.1840219221749));
#20822=CARTESIAN_POINT('Ctrl Pts',(-3.22366532132784,-0.0506120853055336,
32.1900160767371));
#20823=CARTESIAN_POINT('Ctrl Pts',(-3.20889753582343,-0.384242628219668,
32.2121092770526));
#20824=CARTESIAN_POINT('Ctrl Pts',(-3.17101047327491,-0.623973968916234,
32.228749640117));
#20825=CARTESIAN_POINT('Ctrl Pts',(-3.08200055192469,-0.94656489273503,
32.2510192745402));
#20826=CARTESIAN_POINT('Ctrl Pts',(-3.05349410165831,-1.03483803166881,
32.2570894886258));
#20827=CARTESIAN_POINT('Ctrl Pts',(-3.01636191059413,-1.13484492181403,
32.2638467849155));
#20828=CARTESIAN_POINT('Ctrl Pts',(-3.01142116997953,-1.14789142596748,
32.2647258998003));
#20829=CARTESIAN_POINT('Ctrl Pts',(-3.00384559654875,-1.16750987703003,
32.2660437598006));
#20830=CARTESIAN_POINT('Ctrl Pts',(-3.00127364536192,-1.1741056974553,32.2664861297846));
#20831=CARTESIAN_POINT('Ctrl Pts',(-2.99663512387307,-1.18588644032712,
32.2672749184583));
#20832=CARTESIAN_POINT('Ctrl Pts',(-2.99457680639064,-1.19107450110663,
32.2676218239455));
#20833=CARTESIAN_POINT('Ctrl Pts',(-2.99009201281197,-1.20229346454582,
32.2683709751067));
#20834=CARTESIAN_POINT('Ctrl Pts',(-2.98766077210108,-1.20832236285817,
32.2687729279583));
#20835=CARTESIAN_POINT('Ctrl Pts',(-2.98082103074559,-1.22513644049199,
32.2698922904996));
#20836=CARTESIAN_POINT('Ctrl Pts',(-2.97637220712789,-1.23590525909468,
32.2706073026539));
#20837=CARTESIAN_POINT('Ctrl Pts',(-2.95020250469586,-1.2982907150566,32.2747397485273));
#20838=CARTESIAN_POINT('Ctrl Pts',(-2.92719613655321,-1.34936179668311,
32.2780839514318));
#20839=CARTESIAN_POINT('Ctrl Pts',(-2.79246879816565,-1.628753695155,32.2963009923558));
#20840=CARTESIAN_POINT('Ctrl Pts',(-2.65536268545062,-1.84385383607882,
32.3100938861088));
#20841=CARTESIAN_POINT('Ctrl Pts',(-2.39053701552614,-2.16756793231108,
32.3337171517172));
#20842=CARTESIAN_POINT('Ctrl Pts',(-2.27715943863118,-2.28638413007821,
32.3431679597455));
#20843=CARTESIAN_POINT('Ctrl Pts',(-2.13895533847233,-2.41069855614808,
32.3543485735389));
#20844=CARTESIAN_POINT('Ctrl Pts',(-2.1225194768875,-2.42518215862843,32.3556729365911));
#20845=CARTESIAN_POINT('Ctrl Pts',(-2.09602604277873,-2.44805307089488,
32.3578000473681));
#20846=CARTESIAN_POINT('Ctrl Pts',(-2.08606261272699,-2.45654875338665,
32.3585982925504));
#20847=CARTESIAN_POINT('Ctrl Pts',(-2.06833853309669,-2.47147625218798,
32.3600154513119));
#20848=CARTESIAN_POINT('Ctrl Pts',(-2.06059891875293,-2.4779328572401,32.3606333356133));
#20849=CARTESIAN_POINT('Ctrl Pts',(-2.04446697060567,-2.49126274012229,
32.3619193188305));
#20850=CARTESIAN_POINT('Ctrl Pts',(-2.0360699780651,-2.49813015554321,32.3625876452498));
#20851=CARTESIAN_POINT('Ctrl Pts',(-2.01429324732095,-2.51575735412601,
32.364318269295));
#20852=CARTESIAN_POINT('Ctrl Pts',(-2.00086204017969,-2.52645273631248,
32.3653831429305));
#20853=CARTESIAN_POINT('Ctrl Pts',(-1.94320690599002,-2.57161588211964,
32.3699440969464));
#20854=CARTESIAN_POINT('Ctrl Pts',(-1.89817521076367,-2.60503196845777,
32.3734814660727));
#20855=CARTESIAN_POINT('Ctrl Pts',(-1.77711819326298,-2.69005733091694,
32.3829323612883));
#20856=CARTESIAN_POINT('Ctrl Pts',(-1.69972217332263,-2.739616676277,32.3889174252026));
#20857=CARTESIAN_POINT('Ctrl Pts',(-1.57263946449086,-2.81353253129002,
32.3986427283713));
#20858=CARTESIAN_POINT('Ctrl Pts',(-1.52426796674987,-2.84002883744678,
32.4023216146312));
#20859=CARTESIAN_POINT('Ctrl Pts',(-1.47525529429555,-2.86526427736657,
32.4060211118892));
#20860=CARTESIAN_POINT('Origin',(0.,0.,4.68922655072688));
#20861=CARTESIAN_POINT('',(-1.47525541125577,-2.86526421714657,33.905101584668));
#20862=CARTESIAN_POINT('',(-1.47525540501188,-2.8652642203614,33.660216611122));
#20863=CARTESIAN_POINT('',(-1.47525540501186,-2.86526422036142,4.68922655072688));
#20864=CARTESIAN_POINT('Ctrl Pts',(-1.47525541125578,-2.86526421714657,
33.905101584668));
#20865=CARTESIAN_POINT('Ctrl Pts',(-1.69531057939917,-2.75196312064189,
33.8885652916234));
#20866=CARTESIAN_POINT('Ctrl Pts',(-1.90159038241384,-2.61368528888915,
33.8714955802727));
#20867=CARTESIAN_POINT('Ctrl Pts',(-2.13267762831647,-2.41680448803221,
33.8516382700764));
#20868=CARTESIAN_POINT('Ctrl Pts',(-2.17438145576787,-2.37935369134562,
33.8480249354861));
#20869=CARTESIAN_POINT('Ctrl Pts',(-2.22355671916634,-2.3328199566314,33.843749694358));
#20870=CARTESIAN_POINT('Ctrl Pts',(-2.23197990031346,-2.32476217446094,
33.8430168632812));
#20871=CARTESIAN_POINT('Ctrl Pts',(-2.2450340267972,-2.31213798699392,33.8418805711419));
#20872=CARTESIAN_POINT('Ctrl Pts',(-2.2496950809723,-2.30760306309399,33.841474738603));
#20873=CARTESIAN_POINT('Ctrl Pts',(-2.25833249464318,-2.29914833821134,
33.8407225351419));
#20874=CARTESIAN_POINT('Ctrl Pts',(-2.26231235584596,-2.29523235049462,
33.8403758875435));
#20875=CARTESIAN_POINT('Ctrl Pts',(-2.27131713211602,-2.28632591725271,
33.8395914196449));
#20876=CARTESIAN_POINT('Ctrl Pts',(-2.27633577540863,-2.28132925164277,
33.8391540993561));
#20877=CARTESIAN_POINT('Ctrl Pts',(-2.29119454430668,-2.26643770179881,
33.8378588336379));
#20878=CARTESIAN_POINT('Ctrl Pts',(-2.30098706692023,-2.25649525374923,
33.8370045653312));
#20879=CARTESIAN_POINT('Ctrl Pts',(-2.37536362752936,-2.17999231793096,
33.8305082990117));
#20880=CARTESIAN_POINT('Ctrl Pts',(-2.43711849971667,-2.11072872725382,
33.8250681649327));
#20881=CARTESIAN_POINT('Ctrl Pts',(-2.64884877933328,-1.85154983181771,
33.805833806235));
#20882=CARTESIAN_POINT('Ctrl Pts',(-2.78031828541351,-1.64756778863008,
33.7926799463854));
#20883=CARTESIAN_POINT('Ctrl Pts',(-2.92856712725885,-1.34835968307134,
33.7736701677506));
#20884=CARTESIAN_POINT('Ctrl Pts',(-2.9658558378288,-1.26422959548301,33.7683608390868));
#20885=CARTESIAN_POINT('Ctrl Pts',(-3.02001976497589,-1.12638724235393,
33.759627878908));
#20886=CARTESIAN_POINT('Ctrl Pts',(-3.03917676958496,-1.07362544056749,
33.7562778596431));
#20887=CARTESIAN_POINT('Ctrl Pts',(-3.06238494401519,-1.00409717961567,
33.7518423181365));
#20888=CARTESIAN_POINT('Ctrl Pts',(-3.06769382018977,-0.987758725213661,
33.750798540593));
#20889=CARTESIAN_POINT('Ctrl Pts',(-3.07614276474595,-0.96103123062179,
33.7490883531957));
#20890=CARTESIAN_POINT('Ctrl Pts',(-3.07936147513867,-0.950667258406022,
33.7484245430008));
#20891=CARTESIAN_POINT('Ctrl Pts',(-3.08546945383179,-0.930643577050133,
33.7471406748097));
#20892=CARTESIAN_POINT('Ctrl Pts',(-3.08836586201137,-0.920986165319195,
33.7465208601634));
#20893=CARTESIAN_POINT('Ctrl Pts',(-3.09492024947608,-0.898753431200608,
33.745092496014));
#20894=CARTESIAN_POINT('Ctrl Pts',(-3.0985469678971,-0.886169148813521,
33.7442829338374));
#20895=CARTESIAN_POINT('Ctrl Pts',(-3.1080352656065,-0.852475403032485,
33.7421123505938));
#20896=CARTESIAN_POINT('Ctrl Pts',(-3.11375838516319,-0.83132797713795,
33.7407468490101));
#20897=CARTESIAN_POINT('Ctrl Pts',(-3.16045129693933,-0.651543728185929,
33.7291094096636));
#20898=CARTESIAN_POINT('Ctrl Pts',(-3.18947801955127,-0.490078475075718,
33.7184503186501));
#20899=CARTESIAN_POINT('Ctrl Pts',(-3.23190277618421,-0.0742830768988021,
33.6905743230458));
#20900=CARTESIAN_POINT('Ctrl Pts',(-3.22770070291164,0.180712163993436,
33.6730301942253));
#20901=CARTESIAN_POINT('Ctrl Pts',(-3.18604612106548,0.488247502101714,
33.6527289717567));
#20902=CARTESIAN_POINT('Ctrl Pts',(-3.17704768323688,0.543731954564406,
33.649105216305));
#20903=CARTESIAN_POINT('Ctrl Pts',(-3.16443393072998,0.610419163202396,
33.6448193489147));
#20904=CARTESIAN_POINT('Ctrl Pts',(-3.16220352100297,0.6218702102047,33.6440859086618));
#20905=CARTESIAN_POINT('Ctrl Pts',(-3.15863259880329,0.639687412197749,
33.6429488797428));
#20906=CARTESIAN_POINT('Ctrl Pts',(-3.15733493503664,0.64606190827203,33.6425429147233));
#20907=CARTESIAN_POINT('Ctrl Pts',(-3.15488766311264,0.6579001201662,33.6417905917697));
#20908=CARTESIAN_POINT('Ctrl Pts',(-3.15374316922362,0.663364724915909,
33.6414439563693));
#20909=CARTESIAN_POINT('Ctrl Pts',(-3.15111534014424,0.67575127595778,33.6406596765853));
#20910=CARTESIAN_POINT('Ctrl Pts',(-3.14962339958502,0.682671309559527,
33.6402225312141));
#20911=CARTESIAN_POINT('Ctrl Pts',(-3.14512558941835,0.70320476860301,33.638928263838));
#20912=CARTESIAN_POINT('Ctrl Pts',(-3.14205412789166,0.716803873792837,
33.6380748105598));
#20913=CARTESIAN_POINT('Ctrl Pts',(-3.11796838207419,0.820314804306374,
33.6316041442122));
#20914=CARTESIAN_POINT('Ctrl Pts',(-3.09318485771091,0.90931516952203,33.6261870017195));
#20915=CARTESIAN_POINT('Ctrl Pts',(-2.98960636892076,1.22765446023291,33.6069432922198));
#20916=CARTESIAN_POINT('Ctrl Pts',(-2.88883154327705,1.44898135043722,33.5937634997309));
#20917=CARTESIAN_POINT('Ctrl Pts',(-2.71691602821771,1.73578157202477,33.5747272151386));
#20918=CARTESIAN_POINT('Ctrl Pts',(-2.66629737136026,1.81257462390482,33.5694205565016));
#20919=CARTESIAN_POINT('Ctrl Pts',(-2.57961614449665,1.93257490994135,33.5606915871537));
#20920=CARTESIAN_POINT('Ctrl Pts',(-2.54558375648294,1.97718688992095,33.5573428006244));
#20921=CARTESIAN_POINT('Ctrl Pts',(-2.4996346696397,2.03426623877532,33.552908664357));
#20922=CARTESIAN_POINT('Ctrl Pts',(-2.48875687277528,2.04755996794475,33.5518650257321));
#20923=CARTESIAN_POINT('Ctrl Pts',(-2.47083436820923,2.06910919217336,33.5501550087713));
#20924=CARTESIAN_POINT('Ctrl Pts',(-2.46385322311762,2.07741729429547,33.5494912290946));
#20925=CARTESIAN_POINT('Ctrl Pts',(-2.45030507612276,2.09337628143266,33.5482073797634));
#20926=CARTESIAN_POINT('Ctrl Pts',(-2.44374386012715,2.10103192839646,33.5475875532427));
#20927=CARTESIAN_POINT('Ctrl Pts',(-2.42857703578079,2.11856146776315,33.5461591041454));
#20928=CARTESIAN_POINT('Ctrl Pts',(-2.41994698695365,2.12841388916854,33.5453494685017));
#20929=CARTESIAN_POINT('Ctrl Pts',(-2.39671911886759,2.15460789154794,33.5431785601508));
#20930=CARTESIAN_POINT('Ctrl Pts',(-2.3820144899698,2.17085343409826,33.5418128048172));
#20931=CARTESIAN_POINT('Ctrl Pts',(-2.25582664871502,2.30743879070337,33.5301624610827));
#20932=CARTESIAN_POINT('Ctrl Pts',(-2.13548825528763,2.41923599937711,33.5194897257598));
#20933=CARTESIAN_POINT('Ctrl Pts',(-1.8080037731613,2.6799351616483,33.4915704096102));
#20934=CARTESIAN_POINT('Ctrl Pts',(-1.59075110143172,2.81432697847393,33.4739956753835));
#20935=CARTESIAN_POINT('Ctrl Pts',(-1.30952439907176,2.94522622309955,33.4537104289571));
#20936=CARTESIAN_POINT('Ctrl Pts',(-1.25849202675051,2.96739117090903,33.4501243800596));
#20937=CARTESIAN_POINT('Ctrl Pts',(-1.196123234236,2.99258116920105,33.4458769776246));
#20938=CARTESIAN_POINT('Ctrl Pts',(-1.18531482125331,2.99687864785867,33.445145751741));
#20939=CARTESIAN_POINT('Ctrl Pts',(-1.1684324706784,3.00348553222065,33.4440114012174));
#20940=CARTESIAN_POINT('Ctrl Pts',(-1.16237454416993,3.00583519202732,33.4436059179311));
#20941=CARTESIAN_POINT('Ctrl Pts',(-1.15109724614366,3.01017007394198,33.4428540288283));
#20942=CARTESIAN_POINT('Ctrl Pts',(-1.14587987259306,3.01216003267126,33.4425073484203));
#20943=CARTESIAN_POINT('Ctrl Pts',(-1.13402671092958,3.01664569370343,33.4417223816341));
#20944=CARTESIAN_POINT('Ctrl Pts',(-1.1273878591714,3.01913306094684,33.4412845979136));
#20945=CARTESIAN_POINT('Ctrl Pts',(-1.10762355498596,3.02646383684378,33.4399866853785));
#20946=CARTESIAN_POINT('Ctrl Pts',(-1.09447451287261,3.03124377977235,33.4391302559923));
#20947=CARTESIAN_POINT('Ctrl Pts',(-0.992885538735602,3.0674262037669,33.4325647818383));
#20948=CARTESIAN_POINT('Ctrl Pts',(-0.903134053152203,3.09504081957385,
33.4270624925609));
#20949=CARTESIAN_POINT('Ctrl Pts',(-0.579511025181729,3.17933165576605,
33.4078525535622));
#20950=CARTESIAN_POINT('Ctrl Pts',(-0.340662388143395,3.2137119089271,33.3947681847463));
#20951=CARTESIAN_POINT('Ctrl Pts',(-0.0081356523373253,3.22405577500048,
33.3758297082113));
#20952=CARTESIAN_POINT('Ctrl Pts',(0.0840042197246141,3.22297117284149,
33.3705136011199));
#20953=CARTESIAN_POINT('Ctrl Pts',(0.232061255261061,3.21487498674679,33.3617705103617));
#20954=CARTESIAN_POINT('Ctrl Pts',(0.288063533020512,3.21034148164816,33.3584173627918));
#20955=CARTESIAN_POINT('Ctrl Pts',(0.361003346803763,3.20251299401827,33.3539782553722));
#20956=CARTESIAN_POINT('Ctrl Pts',(0.378075196832905,3.20054245730381,33.3529341255126));
#20957=CARTESIAN_POINT('Ctrl Pts',(0.405901942940358,3.19710478028528,33.3512235058603));
#20958=CARTESIAN_POINT('Ctrl Pts',(0.416666771839865,3.19571966231283,33.3505596182623));
#20959=CARTESIAN_POINT('Ctrl Pts',(0.437417203064515,3.19294306230467,33.3492757021845));
#20960=CARTESIAN_POINT('Ctrl Pts',(0.447403689089852,3.19155904597713,33.3486559176027));
#20961=CARTESIAN_POINT('Ctrl Pts',(0.470344416225842,3.18826992788678,33.3472277686543));
#20962=CARTESIAN_POINT('Ctrl Pts',(0.483293803830338,3.18633270296559,33.3464183926119));
#20963=CARTESIAN_POINT('Ctrl Pts',(0.51786759911378,3.18094486418892,33.3442486329774));
#20964=CARTESIAN_POINT('Ctrl Pts',(0.539468950392259,3.17735271768103,33.3428837742108));
#20965=CARTESIAN_POINT('Ctrl Pts',(0.721871183864628,3.14510690047236,33.3312788992833));
#20966=CARTESIAN_POINT('Ctrl Pts',(0.880291141178254,3.1044916454797,33.3206542310558));
#20967=CARTESIAN_POINT('Ctrl Pts',(1.27465914894822,2.97076405636814,33.2928840606322));
#20968=CARTESIAN_POINT('Ctrl Pts',(1.50396205133326,2.86151849308659,33.2754134187567));
#20969=CARTESIAN_POINT('Ctrl Pts',(1.76684169685521,2.69586812064414,33.255071961419));
#20970=CARTESIAN_POINT('Ctrl Pts',(1.81473942900712,2.6638611611531,33.2513558726949));
#20971=CARTESIAN_POINT('Ctrl Pts',(1.87134729900661,2.62379780019707,33.2469759900922));
#20972=CARTESIAN_POINT('Ctrl Pts',(1.88090075121767,2.6169577726662,33.2462372439097));
#20973=CARTESIAN_POINT('Ctrl Pts',(1.89569991469763,2.60623904308241,33.2450937992664));
#20974=CARTESIAN_POINT('Ctrl Pts',(1.90097150091154,2.60239648608435,33.2446866817957));
#20975=CARTESIAN_POINT('Ctrl Pts',(1.91073177118265,2.59523656204553,33.2439333137136));
#20976=CARTESIAN_POINT('Ctrl Pts',(1.9152234632616,2.59192357157722,33.2435867787757));
#20977=CARTESIAN_POINT('Ctrl Pts',(1.92537281045458,2.58439680891437,33.2428041097164));
#20978=CARTESIAN_POINT('Ctrl Pts',(1.93102523661592,2.58017613021912,33.2423684660254));
#20979=CARTESIAN_POINT('Ctrl Pts',(1.94771465926231,2.56762853974097,33.2410827544212));
#20980=CARTESIAN_POINT('Ctrl Pts',(1.95871214737732,2.55924900148646,33.2402362836725));
#20981=CARTESIAN_POINT('Ctrl Pts',(2.04009586749581,2.49640676504022,33.2339749825782));
#20982=CARTESIAN_POINT('Ctrl Pts',(2.10825996911913,2.43911477734735,33.2287458794735));
#20983=CARTESIAN_POINT('Ctrl Pts',(2.35608028398883,2.21265889393444,33.2094167756447));
#20984=CARTESIAN_POINT('Ctrl Pts',(2.51848755508962,2.02588463223565,33.1960181108751));
#20985=CARTESIAN_POINT('Ctrl Pts',(2.7097195090643,1.74696940995367,33.1767612676353));
#20986=CARTESIAN_POINT('Ctrl Pts',(2.75819883300765,1.66937689846189,33.1714812702249));
#20987=CARTESIAN_POINT('Ctrl Pts',(2.83088391091098,1.54121313355475,33.1627921629424));
#20988=CARTESIAN_POINT('Ctrl Pts',(2.85718615166249,1.49188751739117,33.1594557010843));
#20989=CARTESIAN_POINT('Ctrl Pts',(2.88986626982433,1.42656396915544,33.1550356160375));
#20990=CARTESIAN_POINT('Ctrl Pts',(2.89741840600205,1.41116206667512,33.1539933689585));
#20991=CARTESIAN_POINT('Ctrl Pts',(2.90954457508609,1.38592408847538,33.1522850591905));
#20992=CARTESIAN_POINT('Ctrl Pts',(2.91419260448723,1.37612378543218,33.1516215851556));
#20993=CARTESIAN_POINT('Ctrl Pts',(2.92306638619555,1.35716696133607,33.1503379240567));
#20994=CARTESIAN_POINT('Ctrl Pts',(2.92729881354909,1.34801369115939,33.1497179779593));
#20995=CARTESIAN_POINT('Ctrl Pts',(2.93693428517259,1.32691613323543,33.1482886750025));
#20996=CARTESIAN_POINT('Ctrl Pts',(2.94230752113732,1.31495850237124,33.1474783011181));
#20997=CARTESIAN_POINT('Ctrl Pts',(2.95648303512143,1.28289030530972,33.1453041249689));
#20998=CARTESIAN_POINT('Ctrl Pts',(2.96515291693345,1.26272230244952,33.1439358188462));
#20999=CARTESIAN_POINT('Ctrl Pts',(3.03764845674439,1.08921767808597,33.1321543217278));
#21000=CARTESIAN_POINT('Ctrl Pts',(3.08972834569552,0.931271594622281,33.1213428036412));
#21001=CARTESIAN_POINT('Ctrl Pts',(3.19149484625394,0.517696489777949,33.0929191056644));
#21002=CARTESIAN_POINT('Ctrl Pts',(3.22283672148331,0.258783790515589,33.0749644616394));
#21003=CARTESIAN_POINT('Ctrl Pts',(3.22273372058091,-0.0492191042587242,
33.0549003123629));
#21004=CARTESIAN_POINT('Ctrl Pts',(3.22163891785126,-0.0973572008384966,
33.0518049848874));
#21005=CARTESIAN_POINT('Ctrl Pts',(3.21894454657732,-0.156993514469821,
33.0480350902363));
#21006=CARTESIAN_POINT('Ctrl Pts',(3.21836123360326,-0.168528742632896,
33.0473089059134));
#21007=CARTESIAN_POINT('Ctrl Pts',(3.21734997899298,-0.186600028739783,
33.0461762373029));
#21008=CARTESIAN_POINT('Ctrl Pts',(3.21696411126131,-0.19313820626645,33.0457674616939));
#21009=CARTESIAN_POINT('Ctrl Pts',(3.21621264563369,-0.205243528497641,
33.0450125726018));
#21010=CARTESIAN_POINT('Ctrl Pts',(3.21585252668228,-0.210810852038877,
33.044666164964));
#21011=CARTESIAN_POINT('Ctrl Pts',(3.21500663215855,-0.223381276763552,
33.0438857350055));
#21012=CARTESIAN_POINT('Ctrl Pts',(3.21451243296257,-0.230383723740913,
33.0434521910989));
#21013=CARTESIAN_POINT('Ctrl Pts',(3.21295572147802,-0.25146033922258,33.0421507348878));
#21014=CARTESIAN_POINT('Ctrl Pts',(3.21182361217343,-0.265529417527553,
33.0412866388439));
#21015=CARTESIAN_POINT('Ctrl Pts',(3.19904455428085,-0.412273933941461,
33.0323182273948));
#21016=CARTESIAN_POINT('Ctrl Pts',(3.17927452020103,-0.544130897736348,
33.0246362002165));
#21017=CARTESIAN_POINT('Ctrl Pts',(3.10313446795583,-0.899924678833476,
33.0040428507792));
#21018=CARTESIAN_POINT('Ctrl Pts',(3.03080510532378,-1.11961172746976,32.9914320538523));
#21019=CARTESIAN_POINT('Ctrl Pts',(2.89049461495532,-1.42938224049477,32.9718833329992));
#21020=CARTESIAN_POINT('Ctrl Pts',(2.84030004951245,-1.52669072770253,32.9654699017901));
#21021=CARTESIAN_POINT('Ctrl Pts',(2.77513067424075,-1.63864961379603,32.9576661513925));
#21022=CARTESIAN_POINT('Ctrl Pts',(2.76484091562407,-1.65595214271126,32.9564477532775));
#21023=CARTESIAN_POINT('Ctrl Pts',(2.74779316749824,-1.6840165442531,32.9544506857886));
#21024=CARTESIAN_POINT('Ctrl Pts',(2.74113233740833,-1.69483701700616,32.9536755793747));
#21025=CARTESIAN_POINT('Ctrl Pts',(2.72911488678863,-1.71410312240555,32.9522861707441));
#21026=CARTESIAN_POINT('Ctrl Pts',(2.72378258546942,-1.72256378780028,32.9516727747768));
#21027=CARTESIAN_POINT('Ctrl Pts',(2.71241854528443,-1.74041020177461,32.9503719712198));
#21028=CARTESIAN_POINT('Ctrl Pts',(2.70637728709467,-1.74978970454354,32.9496842137768));
#21029=CARTESIAN_POINT('Ctrl Pts',(2.69015916161012,-1.77468463189595,32.9478477257405));
#21030=CARTESIAN_POINT('Ctrl Pts',(2.67989691012695,-1.79014367729256,32.9466957972543));
#21031=CARTESIAN_POINT('Ctrl Pts',(2.63020288933737,-1.8636176895258,32.9411647669136));
#21032=CARTESIAN_POINT('Ctrl Pts',(2.58902001193395,-1.92041981612103,32.9367193943096));
#21033=CARTESIAN_POINT('Ctrl Pts',(2.38118906282716,-2.18822709486243,32.9149068709048));
#21034=CARTESIAN_POINT('Ctrl Pts',(2.19044650969267,-2.37913801747994,32.8965735669121));
#21035=CARTESIAN_POINT('Ctrl Pts',(1.86788299037469,-2.62995918748407,32.8690426065043));
#21036=CARTESIAN_POINT('Ctrl Pts',(1.75200738177078,-2.70853313399905,32.8597365172584));
#21037=CARTESIAN_POINT('Ctrl Pts',(1.61844249412796,-2.78693138080748,32.8499163928834));
#21038=CARTESIAN_POINT('Ctrl Pts',(1.60545126594163,-2.7944353421264,32.8489703493416));
#21039=CARTESIAN_POINT('Ctrl Pts',(1.58615162590132,-2.80540413573197,32.8475788888995));
#21040=CARTESIAN_POINT('Ctrl Pts',(1.57988346991535,-2.80893886886205,32.847129132862));
#21041=CARTESIAN_POINT('Ctrl Pts',(1.568722103029,-2.81518379735845,32.8463321876864));
#21042=CARTESIAN_POINT('Ctrl Pts',(1.56383363175756,-2.81790227355953,32.8459844710727));
#21043=CARTESIAN_POINT('Ctrl Pts',(1.55331518497217,-2.82371577400936,32.8452391639311));
#21044=CARTESIAN_POINT('Ctrl Pts',(1.54768304064095,-2.82680668664678,32.8448418366374));
#21045=CARTESIAN_POINT('Ctrl Pts',(1.532121307783,-2.83528649265728,32.8437487282991));
#21046=CARTESIAN_POINT('Ctrl Pts',(1.52217245422814,-2.84064010843147,32.8430551646226));
#21047=CARTESIAN_POINT('Ctrl Pts',(1.4676109664777,-2.86963144170824,32.839279166703));
#21048=CARTESIAN_POINT('Ctrl Pts',(1.4224730007517,-2.89227207938064,32.8362559736934));
#21049=CARTESIAN_POINT('Ctrl Pts',(1.14300628456107,-3.02432273839991,32.8180339684018));
#21050=CARTESIAN_POINT('Ctrl Pts',(0.896722641424523,-3.10626955590679,
32.8040112962091));
#21051=CARTESIAN_POINT('Ctrl Pts',(0.480927071639537,-3.19096773218185,
32.7800536650873));
#21052=CARTESIAN_POINT('Ctrl Pts',(0.316298426956155,-3.21146547745588,
32.7705121173458));
#21053=CARTESIAN_POINT('Ctrl Pts',(0.128916173166071,-3.22024529389398,
32.7592296494377));
#21054=CARTESIAN_POINT('Ctrl Pts',(0.106986027989452,-3.22104844513118,
32.7579030245892));
#21055=CARTESIAN_POINT('Ctrl Pts',(0.0719471716861846,-3.22197345821536,
32.7557728256951));
#21056=CARTESIAN_POINT('Ctrl Pts',(0.0588427122529572,-3.22223942130419,
32.7549737732803));
#21057=CARTESIAN_POINT('Ctrl Pts',(0.0356540445916773,-3.22256854713764,
32.7535555064266));
#21058=CARTESIAN_POINT('Ctrl Pts',(0.0255704203228948,-3.22266433278892,
32.7529373249543));
#21059=CARTESIAN_POINT('Ctrl Pts',(0.00463905159577563,-3.22276491754879,
32.7516510463084));
#21060=CARTESIAN_POINT('Ctrl Pts',(-0.00620858570992438,-3.22276227535319,
32.7509827230848));
#21061=CARTESIAN_POINT('Ctrl Pts',(-0.0342138956032114,-3.22261405957662,
32.7492527988418));
#21062=CARTESIAN_POINT('Ctrl Pts',(-0.0513706203514442,-3.22238622896835,
32.7481886274113));
#21063=CARTESIAN_POINT('Ctrl Pts',(-0.124445632281463,-3.22083210378685,
32.743636855234));
#21064=CARTESIAN_POINT('Ctrl Pts',(-0.180323326982917,-3.21818722595246,
32.7401081796733));
#21065=CARTESIAN_POINT('Ctrl Pts',(-0.32740542293295,-3.20738284186303,
32.7306869690326));
#21066=CARTESIAN_POINT('Ctrl Pts',(-0.418374846235888,-3.19678885765793,
32.7247234667327));
#21067=CARTESIAN_POINT('Ctrl Pts',(-0.751736903474163,-3.14349393027239,
32.7023943564808));
#21068=CARTESIAN_POINT('Ctrl Pts',(-0.98943642851421,-3.07695669882826,
32.6854611413806));
#21069=CARTESIAN_POINT('Ctrl Pts',(-1.30009905826486,-2.95023187124312,
32.6631601046024));
#21070=CARTESIAN_POINT('Ctrl Pts',(-1.38152323385195,-2.91299199914829,
32.6573077871076));
#21071=CARTESIAN_POINT('Ctrl Pts',(-1.46595678380419,-2.87003755765287,
32.6513079616142));
#21072=CARTESIAN_POINT('Ctrl Pts',(-1.47060898770064,-2.86765654851168,
32.6509776062806));
#21073=CARTESIAN_POINT('Ctrl Pts',(-1.47525540501479,-2.8652642203599,32.6506479065737));
#21074=CARTESIAN_POINT('',(3.22274859474753,0.00298732763886637,32.814161792891));
#21075=CARTESIAN_POINT('Ctrl Pts',(-1.47525529429555,-2.86526427736657,
32.4060211118892));
#21076=CARTESIAN_POINT('Ctrl Pts',(-1.39484804649379,-2.90666402501159,
32.41209028498));
#21077=CARTESIAN_POINT('Ctrl Pts',(-1.31271522488961,-2.9446702933697,32.418215933755));
#21078=CARTESIAN_POINT('Ctrl Pts',(-1.05498043027862,-3.05099990093074,
32.4370884081259));
#21079=CARTESIAN_POINT('Ctrl Pts',(-0.874906521245708,-3.10743291387524,
32.449807403356));
#21080=CARTESIAN_POINT('Ctrl Pts',(-0.676634677132355,-3.15095174123194,
32.4626729572916));
#21081=CARTESIAN_POINT('Ctrl Pts',(-0.662331285902206,-3.1539893228438,
32.4635947268513));
#21082=CARTESIAN_POINT('Ctrl Pts',(-0.641033050275847,-3.15836110696402,
32.4649573327813));
#21083=CARTESIAN_POINT('Ctrl Pts',(-0.634053894286388,-3.15976959840119,
32.4654022583912));
#21084=CARTESIAN_POINT('Ctrl Pts',(-0.621592058936658,-3.16224162011029,
32.4661938154477));
#21085=CARTESIAN_POINT('Ctrl Pts',(-0.616111243562462,-3.16331403576564,
32.4665409479681));
#21086=CARTESIAN_POINT('Ctrl Pts',(-0.604272908015296,-3.16559847424139,
32.4672885693926));
#21087=CARTESIAN_POINT('Ctrl Pts',(-0.597914535005387,-3.16680559208341,
32.4676887762993));
#21088=CARTESIAN_POINT('Ctrl Pts',(-0.581024869463102,-3.16995936235909,
32.4687483870502));
#21089=CARTESIAN_POINT('Ctrl Pts',(-0.57048732975085,-3.17187270741842,
32.4694059227346));
#21090=CARTESIAN_POINT('Ctrl Pts',(-0.515161565583093,-3.18163380533274,
32.4728404833274));
#21091=CARTESIAN_POINT('Ctrl Pts',(-0.470217993924355,-3.18858599350661,
32.4755696656836));
#21092=CARTESIAN_POINT('Ctrl Pts',(-0.335618083148154,-3.20649873356882,
32.4836023584478));
#21093=CARTESIAN_POINT('Ctrl Pts',(-0.245628345288927,-3.21464504109731,
32.4887878617375));
#21094=CARTESIAN_POINT('Ctrl Pts',(0.104682712549077,-3.23155760944982,
32.5086537179753));
#21095=CARTESIAN_POINT('Ctrl Pts',(0.365327829932817,-3.21254741585919,
32.5228349408671));
#21096=CARTESIAN_POINT('Ctrl Pts',(0.704460088561196,-3.14596785493337,
32.5429085629154));
#21097=CARTESIAN_POINT('Ctrl Pts',(0.787380738413174,-3.12624494289355,
32.5479411687893));
#21098=CARTESIAN_POINT('Ctrl Pts',(0.889103026786777,-3.09774616452662,
32.5543135848249));
#21099=CARTESIAN_POINT('Ctrl Pts',(0.90873509933982,-3.09204398118237,32.5555526942832));
#21100=CARTESIAN_POINT('Ctrl Pts',(0.939508698094618,-3.08278732580966,
32.5575101415069));
#21101=CARTESIAN_POINT('Ctrl Pts',(0.950687614269772,-3.07935826826967,
32.5582243655098));
#21102=CARTESIAN_POINT('Ctrl Pts',(0.970389176276476,-3.07319743974693,
32.5594887819215));
#21103=CARTESIAN_POINT('Ctrl Pts',(0.978919613098458,-3.0704908476692,32.5600381397819));
#21104=CARTESIAN_POINT('Ctrl Pts',(0.998438938031406,-3.06420802067885,
32.5612995611318));
#21105=CARTESIAN_POINT('Ctrl Pts',(1.00942003744565,-3.0606081567876,32.5620123995555));
#21106=CARTESIAN_POINT('Ctrl Pts',(1.03820735768362,-3.05099921548932,32.5638896454268));
#21107=CARTESIAN_POINT('Ctrl Pts',(1.05598059159825,-3.04489338015105,32.5650572465812));
#21108=CARTESIAN_POINT('Ctrl Pts',(1.14987903089594,-3.01171441926257,32.5712723458542));
#21109=CARTESIAN_POINT('Ctrl Pts',(1.22501364585072,-2.98194319429782,32.576409257774));
#21110=CARTESIAN_POINT('Ctrl Pts',(1.55350542802854,-2.83727126819555,32.5996236041743));
#21111=CARTESIAN_POINT('Ctrl Pts',(1.79245679538935,-2.69268278754898,32.6186954563068));
#21112=CARTESIAN_POINT('Ctrl Pts',(2.10243759296631,-2.44538510752028,32.6452926506345));
#21113=CARTESIAN_POINT('Ctrl Pts',(2.19091231493155,-2.36644497206343,32.6531208637461));
#21114=CARTESIAN_POINT('Ctrl Pts',(2.28531546148905,-2.27237083728936,32.6615692412041));
#21115=CARTESIAN_POINT('Ctrl Pts',(2.29571235696151,-2.26186665707975,32.6625010365024));
#21116=CARTESIAN_POINT('Ctrl Pts',(2.31103211423161,-2.24617436167468,32.6638755305101));
#21117=CARTESIAN_POINT('Ctrl Pts',(2.3160103871061,-2.24104096018165,32.6643224210818));
#21118=CARTESIAN_POINT('Ctrl Pts',(2.32484807794097,-2.23186697558647,32.6651161191681));
#21119=CARTESIAN_POINT('Ctrl Pts',(2.32871410500528,-2.22783289342548,32.6654634387173));
#21120=CARTESIAN_POINT('Ctrl Pts',(2.33702074847036,-2.21911991402158,32.6662099410067));
#21121=CARTESIAN_POINT('Ctrl Pts',(2.34145780222227,-2.21443774663565,32.666608849857));
#21122=CARTESIAN_POINT('Ctrl Pts',(2.35055030056911,-2.20478507446713,32.6674267097068));
#21123=CARTESIAN_POINT('Ctrl Pts',(2.35520411191296,-2.19981306780473,32.6678455366032));
#21124=CARTESIAN_POINT('Ctrl Pts',(2.37699462063653,-2.17638426085354,32.6698078668024));
#21125=CARTESIAN_POINT('Ctrl Pts',(2.39393090330502,-2.15774113325243,32.6713367334204));
#21126=CARTESIAN_POINT('Ctrl Pts',(2.49796256946775,-2.04049227147627,32.6807653659123));
#21127=CARTESIAN_POINT('Ctrl Pts',(2.57918012713303,-1.93681784657678,32.6882954021693));
#21128=CARTESIAN_POINT('Ctrl Pts',(2.71718240244353,-1.73652014046452,32.7020071237146));
#21129=CARTESIAN_POINT('Ctrl Pts',(2.77570634492024,-1.64135230951347,32.7082109445752));
#21130=CARTESIAN_POINT('Ctrl Pts',(2.86103061052913,-1.48493993474693,32.7181891857034));
#21131=CARTESIAN_POINT('Ctrl Pts',(2.8910708539342,-1.42557066091932,32.7219289446648));
#21132=CARTESIAN_POINT('Ctrl Pts',(2.9806195008897,-1.23410208416092,32.7339312444352));
#21133=CARTESIAN_POINT('Ctrl Pts',(3.03306388312251,-1.09891595040438,32.7423280633316));
#21134=CARTESIAN_POINT('Ctrl Pts',(3.08263348383184,-0.940185612816217,
32.7523337165343));
#21135=CARTESIAN_POINT('Ctrl Pts',(3.08882619650378,-0.919636273651769,
32.7536315586163));
#21136=CARTESIAN_POINT('Ctrl Pts',(3.09842944465002,-0.886578024626569,
32.7557240922569));
#21137=CARTESIAN_POINT('Ctrl Pts',(3.10197061356489,-0.874107500308189,
32.7565145123079));
#21138=CARTESIAN_POINT('Ctrl Pts',(3.10812579449117,-0.851922999431207,
32.7579226460436));
#21139=CARTESIAN_POINT('Ctrl Pts',(3.11076976037074,-0.842217457465309,
32.7585393741851));
#21140=CARTESIAN_POINT('Ctrl Pts',(3.11618551295834,-0.821963720052884,
32.7598278621795));
#21141=CARTESIAN_POINT('Ctrl Pts',(3.11894927622815,-0.811413529519908,
32.7604998740183));
#21142=CARTESIAN_POINT('Ctrl Pts',(3.12443655062962,-0.790024492918964,
32.7618640536353));
#21143=CARTESIAN_POINT('Ctrl Pts',(3.12715733847663,-0.779185108730077,
32.7625562994536));
#21144=CARTESIAN_POINT('Ctrl Pts',(3.13370547461799,-0.752511091504904,
32.764262145044));
#21145=CARTESIAN_POINT('Ctrl Pts',(3.13746921185679,-0.736661301681656,
32.7652777837164));
#21146=CARTESIAN_POINT('Ctrl Pts',(3.15412750157559,-0.664065945541543,
32.7699392589516));
#21147=CARTESIAN_POINT('Ctrl Pts',(3.16560312076216,-0.607009102859284,
32.7736301123873));
#21148=CARTESIAN_POINT('Ctrl Pts',(3.20712647278227,-0.367124868945356,
32.7892681278082));
#21149=CARTESIAN_POINT('Ctrl Pts',(3.22292030341193,-0.182219354745417,
32.801640427985));
#21150=CARTESIAN_POINT('Ctrl Pts',(3.22274861527754,0.00298751178999402,
32.8141617710204));
#21151=CARTESIAN_POINT('Ctrl Pts',(3.22274861544609,0.00298732996773646,
32.8141617587279));
#21152=CARTESIAN_POINT('Ctrl Pts',(3.22254821683741,0.219178492523581,32.82877786743));
#21153=CARTESIAN_POINT('Ctrl Pts',(3.20059451488405,0.434825313060781,32.8435351721082));
#21154=CARTESIAN_POINT('Ctrl Pts',(3.15408936426525,0.661875181097467,32.8583473192536));
#21155=CARTESIAN_POINT('Ctrl Pts',(3.15086501835497,0.677058439667333,32.8593340847704));
#21156=CARTESIAN_POINT('Ctrl Pts',(3.14562904415603,0.70086652878365,32.8608748524812));
#21157=CARTESIAN_POINT('Ctrl Pts',(3.14369139333282,0.709507154534677,32.8614326852729));
#21158=CARTESIAN_POINT('Ctrl Pts',(3.13995805039784,0.725839783878309,32.8624843996454));
#21159=CARTESIAN_POINT('Ctrl Pts',(3.13816964987695,0.733533367913012,32.8629786759137));
#21160=CARTESIAN_POINT('Ctrl Pts',(3.1350438339135,0.746759747290711,32.8638263518822));
#21161=CARTESIAN_POINT('Ctrl Pts',(3.13372001865912,0.752295691454266,32.8641805273361));
#21162=CARTESIAN_POINT('Ctrl Pts',(3.13112769980832,0.763010694757067,32.8648648069713));
#21163=CARTESIAN_POINT('Ctrl Pts',(3.12986100981597,0.768190115164842,32.8651950172635));
#21164=CARTESIAN_POINT('Ctrl Pts',(3.12641332444486,0.78213740374081,32.8660827740626));
#21165=CARTESIAN_POINT('Ctrl Pts',(3.12420828330465,0.790899361946299,32.8666389418758));
#21166=CARTESIAN_POINT('Ctrl Pts',(3.11591133141757,0.823291956719157,32.8686897652535));
#21167=CARTESIAN_POINT('Ctrl Pts',(3.10958774924866,0.846863143310266,32.8701716232201));
#21168=CARTESIAN_POINT('Ctrl Pts',(3.05224328908114,1.05130666770391,32.8829512843741));
#21169=CARTESIAN_POINT('Ctrl Pts',(2.9857523953139,1.22749198326639,32.8934769757778));
#21170=CARTESIAN_POINT('Ctrl Pts',(2.85690170263137,1.49538435153591,32.9100933422932));
#21171=CARTESIAN_POINT('Ctrl Pts',(2.80455186790844,1.59139869031303,32.916182351003));
#21172=CARTESIAN_POINT('Ctrl Pts',(2.67304713907188,1.80587507789757,32.930415745757));
#21173=CARTESIAN_POINT('Ctrl Pts',(2.5907229696946,1.92211170615877,32.9386139946019));
#21174=CARTESIAN_POINT('Ctrl Pts',(2.47952014550147,2.05894556251995,32.9491446161738));
#21175=CARTESIAN_POINT('Ctrl Pts',(2.45762858796366,2.085027235062,32.951194098938));
#21176=CARTESIAN_POINT('Ctrl Pts',(2.42806696076517,2.11913456861155,32.9539333114126));
#21177=CARTESIAN_POINT('Ctrl Pts',(2.4207623075483,2.12747510711607,32.9546079398342));
#21178=CARTESIAN_POINT('Ctrl Pts',(2.40622730457362,2.14389956536553,32.9559460528837));
#21179=CARTESIAN_POINT('Ctrl Pts',(2.39899889462704,2.15198501079376,32.9566094515741));
#21180=CARTESIAN_POINT('Ctrl Pts',(2.38497382522173,2.16751448005937,32.957892758171));
#21181=CARTESIAN_POINT('Ctrl Pts',(2.3781827741766,2.17496341513716,32.9585124241679));
#21182=CARTESIAN_POINT('Ctrl Pts',(2.36248675336626,2.19201858559234,32.9599407805972));
#21183=CARTESIAN_POINT('Ctrl Pts',(2.35355798497797,2.20160258507677,32.9607504852929));
#21184=CARTESIAN_POINT('Ctrl Pts',(2.32952925950451,2.22708141768664,32.9629221910417));
#21185=CARTESIAN_POINT('Ctrl Pts',(2.31432532477309,2.24287682779098,32.9642886817434));
#21186=CARTESIAN_POINT('Ctrl Pts',(2.18341077532949,2.37613583205806,32.9759925231601));
#21187=CARTESIAN_POINT('Ctrl Pts',(2.05902228151188,2.4846964403543,32.9867221900102));
#21188=CARTESIAN_POINT('Ctrl Pts',(1.76922500931947,2.70086120576445,33.0108420739501));
#21189=CARTESIAN_POINT('Ctrl Pts',(1.60112989837387,2.80378071718617,33.0243037573606));
#21190=CARTESIAN_POINT('Ctrl Pts',(1.35795709729627,2.92362921898249,33.0424335399758));
#21191=CARTESIAN_POINT('Ctrl Pts',(1.29008363437771,2.95420733859527,33.047356494781));
#21192=CARTESIAN_POINT('Ctrl Pts',(1.18415103180865,2.99758358768472,33.0547710194766));
#21193=CARTESIAN_POINT('Ctrl Pts',(1.14681231389973,3.01206621750124,33.057334478464));
#21194=CARTESIAN_POINT('Ctrl Pts',(1.09939746123825,3.02944748105969,33.0605185647441));
#21195=CARTESIAN_POINT('Ctrl Pts',(1.08956592616303,3.03299734881753,33.0611749712198));
#21196=CARTESIAN_POINT('Ctrl Pts',(1.07379673868955,3.03860454967796,33.0622215054983));
#21197=CARTESIAN_POINT('Ctrl Pts',(1.06787013768976,3.04069242377124,33.0626134091202));
#21198=CARTESIAN_POINT('Ctrl Pts',(1.05663236657261,3.0446144543874,33.0633537819896));
#21199=CARTESIAN_POINT('Ctrl Pts',(1.05132257400911,3.04645203142315,33.0637024433731));
#21200=CARTESIAN_POINT('Ctrl Pts',(1.03910012166671,3.05064613410803,33.0645023873519));
#21201=CARTESIAN_POINT('Ctrl Pts',(1.03218424126177,3.05299305484908,33.0649530975991));
#21202=CARTESIAN_POINT('Ctrl Pts',(1.01364752562713,3.05921334658098,33.0661561430386));
#21203=CARTESIAN_POINT('Ctrl Pts',(1.00201235182477,3.06304405191075,33.0669060276449));
#21204=CARTESIAN_POINT('Ctrl Pts',(0.915072190078493,3.09111938239442,33.0724722238561));
#21205=CARTESIAN_POINT('Ctrl Pts',(0.838912354402849,3.11265232139756,33.0771414306856));
#21206=CARTESIAN_POINT('Ctrl Pts',(0.74199109393293,3.13623853415201,33.0829144391046));
#21207=CARTESIAN_POINT('Ctrl Pts',(0.721904909761096,3.14092283494992,33.084101812259));
#21208=CARTESIAN_POINT('Ctrl Pts',(0.454419000164066,3.20060174343823,33.0998101881616));
#21209=CARTESIAN_POINT('Ctrl Pts',(0.20141314845607,3.22642107870538,33.1135645299833));
#21210=CARTESIAN_POINT('Ctrl Pts',(-0.132664001225616,3.22102836787693,
33.1326942396608));
#21211=CARTESIAN_POINT('Ctrl Pts',(-0.213230584116318,3.21669936634752,
33.1373746806528));
#21212=CARTESIAN_POINT('Ctrl Pts',(-0.344158407653682,3.20472395039108,
33.1451489266051));
#21213=CARTESIAN_POINT('Ctrl Pts',(-0.394651927594301,3.19889825270692,
33.1481879731844));
#21214=CARTESIAN_POINT('Ctrl Pts',(-0.46101225057508,3.18964686862244,33.1522443825089));
#21215=CARTESIAN_POINT('Ctrl Pts',(-0.477022638378892,3.18729177034332,
33.1532278479773));
#21216=CARTESIAN_POINT('Ctrl Pts',(-0.503734737244689,3.18315669688949,
33.1548769780555));
#21217=CARTESIAN_POINT('Ctrl Pts',(-0.514446535684941,3.18144306877094,
33.1555405279324));
#21218=CARTESIAN_POINT('Ctrl Pts',(-0.535093716633112,3.17803301812316,
33.1568239277939));
#21219=CARTESIAN_POINT('Ctrl Pts',(-0.545030206689636,3.17634400214676,
33.1574435347979));
#21220=CARTESIAN_POINT('Ctrl Pts',(-0.567855859021335,3.17235381230553,
33.1588714696059));
#21221=CARTESIAN_POINT('Ctrl Pts',(-0.580739181956499,3.17002065947254,
33.1596808097193));
#21222=CARTESIAN_POINT('Ctrl Pts',(-0.615136785905561,3.1635745720031,33.1618509018918));
#21223=CARTESIAN_POINT('Ctrl Pts',(-0.636623658660753,3.15932075246752,
33.1632161331257));
#21224=CARTESIAN_POINT('Ctrl Pts',(-0.818491299351512,3.12138525397779,
33.1748556051346));
#21225=CARTESIAN_POINT('Ctrl Pts',(-0.97610611102545,3.07573992396352,33.1855171897619));
#21226=CARTESIAN_POINT('Ctrl Pts',(-1.36735229938579,2.92932350690405,33.2133794792506));
#21227=CARTESIAN_POINT('Ctrl Pts',(-1.59379437568799,2.8125438999033,33.2309059472695));
#21228=CARTESIAN_POINT('Ctrl Pts',(-1.85090986964421,2.63883130783127,33.2512063647467));
#21229=CARTESIAN_POINT('Ctrl Pts',(-1.8968064756676,2.6060360954482,33.254843313869));
#21230=CARTESIAN_POINT('Ctrl Pts',(-1.95113970410506,2.56501612638892,33.2591424493099));
#21231=CARTESIAN_POINT('Ctrl Pts',(-1.96041948655533,2.55793067149038,33.2598764805809));
#21232=CARTESIAN_POINT('Ctrl Pts',(-1.97481003762952,2.54681864355279,33.261014137641));
#21233=CARTESIAN_POINT('Ctrl Pts',(-1.97994735291098,2.54282684611979,33.2614201449728));
#21234=CARTESIAN_POINT('Ctrl Pts',(-1.98946915422156,2.53538186350542,33.262172369432));
#21235=CARTESIAN_POINT('Ctrl Pts',(-1.99385671619039,2.53193287932558,33.2625188649474));
#21236=CARTESIAN_POINT('Ctrl Pts',(-2.00378408823138,2.5240873414287,33.2633025954733));
#21237=CARTESIAN_POINT('Ctrl Pts',(-2.00931838567896,2.51968394975133,33.2637393332713));
#21238=CARTESIAN_POINT('Ctrl Pts',(-2.0256997282627,2.50656175786473,33.2650316931065));
#21239=CARTESIAN_POINT('Ctrl Pts',(-2.03650500789702,2.49779074465531,33.2658836611756));
#21240=CARTESIAN_POINT('Ctrl Pts',(-2.11807225260702,2.43069866689546,33.2723142811886));
#21241=CARTESIAN_POINT('Ctrl Pts',(-2.18638002951525,2.36944546507828,33.2776956308852));
#21242=CARTESIAN_POINT('Ctrl Pts',(-2.42595840876775,2.13541320832331,33.2969539229055));
#21243=CARTESIAN_POINT('Ctrl Pts',(-2.58013914309783,1.94631934001491,33.3101740128229));
#21244=CARTESIAN_POINT('Ctrl Pts',(-2.76123876379042,1.66436750957209,33.3292521348975));
#21245=CARTESIAN_POINT('Ctrl Pts',(-2.80755951247119,1.58498150596806,33.3345553115394));
#21246=CARTESIAN_POINT('Ctrl Pts',(-2.87658702718598,1.45413505750464,33.3432788514775));
#21247=CARTESIAN_POINT('Ctrl Pts',(-2.90145027763158,1.40386872650688,33.3466257985369));
#21248=CARTESIAN_POINT('Ctrl Pts',(-2.93219686171064,1.33739819360027,33.3510576133749));
#21249=CARTESIAN_POINT('Ctrl Pts',(-2.93928035569805,1.32175766951851,33.3521008182964));
#21250=CARTESIAN_POINT('Ctrl Pts',(-2.95063461634486,1.29614451234264,33.3538101517333));
#21251=CARTESIAN_POINT('Ctrl Pts',(-2.95498066420527,1.28620546790602,33.354473683928));
#21252=CARTESIAN_POINT('Ctrl Pts',(-2.96326786817708,1.26698961851998,33.3557570728668));
#21253=CARTESIAN_POINT('Ctrl Pts',(-2.96721585127729,1.25771588216632,33.3563766867554));
#21254=CARTESIAN_POINT('Ctrl Pts',(-2.97619240891793,1.23635259936775,33.3578046708032));
#21255=CARTESIAN_POINT('Ctrl Pts',(-2.98119091300347,1.22425068387007,33.3586140535));
#21256=CARTESIAN_POINT('Ctrl Pts',(-2.99435464763178,1.19182116285148,33.3607843341181));
#21257=CARTESIAN_POINT('Ctrl Pts',(-3.00238648521609,1.17144047869872,33.3621497124367));
#21258=CARTESIAN_POINT('Ctrl Pts',(-3.06877958779751,0.997799595134482,
33.3737966676907));
#21259=CARTESIAN_POINT('Ctrl Pts',(-3.11556275071706,0.840396463538818,
33.3844661647027));
#21260=CARTESIAN_POINT('Ctrl Pts',(-3.20380085196605,0.431708309118718,
33.4123533144407));
#21261=CARTESIAN_POINT('Ctrl Pts',(-3.22786115138708,0.177818998295027,
33.4298972485246));
#21262=CARTESIAN_POINT('Ctrl Pts',(-3.22052108757301,-0.132306711781043,
33.4501884075272));
#21263=CARTESIAN_POINT('Ctrl Pts',(-3.21773183101023,-0.1883186410448,33.4538037002444));
#21264=CARTESIAN_POINT('Ctrl Pts',(-3.21259889385944,-0.255854954542151,
33.4580807577507));
#21265=CARTESIAN_POINT('Ctrl Pts',(-3.21165254418778,-0.267472158926023,
33.4588135267291));
#21266=CARTESIAN_POINT('Ctrl Pts',(-3.21008015760449,-0.28556122520582,
33.4599496571486));
#21267=CARTESIAN_POINT('Ctrl Pts',(-3.20949753802068,-0.292036618935335,
33.4603553900228));
#21268=CARTESIAN_POINT('Ctrl Pts',(-3.20837833855174,-0.304067675371715,
33.4611073666807));
#21269=CARTESIAN_POINT('Ctrl Pts',(-3.207846927222,-0.309623653353343,33.4614538872164));
#21270=CARTESIAN_POINT('Ctrl Pts',(-3.20660883806567,-0.322222629696172,
33.4622380063206));
#21271=CARTESIAN_POINT('Ctrl Pts',(-3.20589339118047,-0.329264680906096,
33.4626751056123));
#21272=CARTESIAN_POINT('Ctrl Pts',(-3.20369958877302,-0.350172751837709,
33.4639695279551));
#21273=CARTESIAN_POINT('Ctrl Pts',(-3.20215441087964,-0.364031806872042,
33.4648231797169));
#21274=CARTESIAN_POINT('Ctrl Pts',(-3.18966937048855,-0.469775800286934,
33.4713061363506));
#21275=CARTESIAN_POINT('Ctrl Pts',(-3.17486552036997,-0.561170539849794,
33.4767344907806));
#21276=CARTESIAN_POINT('Ctrl Pts',(-3.10716912956218,-0.888965110141979,
33.4959732949462));
#21277=CARTESIAN_POINT('Ctrl Pts',(-3.03161728829047,-1.11985196555058,
33.5091401015489));
#21278=CARTESIAN_POINT('Ctrl Pts',(-2.89266269291002,-1.42375561537799,
33.5281638821857));
#21279=CARTESIAN_POINT('Ctrl Pts',(-2.85085485522526,-1.50572313829151,
33.5334727086058));
#21280=CARTESIAN_POINT('Ctrl Pts',(-2.77798835726111,-1.63463983206211,
33.5422046933284));
#21281=CARTESIAN_POINT('Ctrl Pts',(-2.74910544859249,-1.68276122763449,
33.5455542491201));
#21282=CARTESIAN_POINT('Ctrl Pts',(-2.70976221439132,-1.74459200784426,
33.5499890377277));
#21283=CARTESIAN_POINT('Ctrl Pts',(-2.70042661011467,-1.75900785615045,
33.55103253664));
#21284=CARTESIAN_POINT('Ctrl Pts',(-2.68500669728452,-1.78240688256158,
33.5527422307683));
#21285=CARTESIAN_POINT('Ctrl Pts',(-2.67899138624992,-1.79143529252744,
33.553405827549));
#21286=CARTESIAN_POINT('Ctrl Pts',(-2.66730001727916,-1.80879234905369,
33.5546892564034));
#21287=CARTESIAN_POINT('Ctrl Pts',(-2.66163024240726,-1.81712509013346,
33.5553088451646));
#21288=CARTESIAN_POINT('Ctrl Pts',(-2.64850644800981,-1.83621963140854,
33.5567366494497));
#21289=CARTESIAN_POINT('Ctrl Pts',(-2.64102579390097,-1.84696282792607,
33.5575458766783));
#21290=CARTESIAN_POINT('Ctrl Pts',(-2.6208577448739,-1.87555371791103,33.5597154693262));
#21291=CARTESIAN_POINT('Ctrl Pts',(-2.60805372459752,-1.89331793395098,
33.5610803106803));
#21292=CARTESIAN_POINT('Ctrl Pts',(-2.49807986736813,-2.04266242620315,
33.572699992241));
#21293=CARTESIAN_POINT('Ctrl Pts',(-2.3912186061171,-2.16677912507858,33.583340654715));
#21294=CARTESIAN_POINT('Ctrl Pts',(-2.09604642557909,-2.46106918579612,
33.6111384574185));
#21295=CARTESIAN_POINT('Ctrl Pts',(-1.89623078275139,-2.61812451795397,
33.6286200839546));
#21296=CARTESIAN_POINT('Ctrl Pts',(-1.63124165278221,-2.78000817298476,
33.6489449574626));
#21297=CARTESIAN_POINT('Ctrl Pts',(-1.58159924147276,-2.80854759089056,
33.6526381635886));
#21298=CARTESIAN_POINT('Ctrl Pts',(-1.52090135742906,-2.84132260140222,
33.6569945872463));
#21299=CARTESIAN_POINT('Ctrl Pts',(-1.51055283545487,-2.84683775539471,
33.6577318552148));
#21300=CARTESIAN_POINT('Ctrl Pts',(-1.49440648798576,-2.85532997758415,
33.6588734260387));
#21301=CARTESIAN_POINT('Ctrl Pts',(-1.4886294712769,-2.85834608318441,33.6592801364429));
#21302=CARTESIAN_POINT('Ctrl Pts',(-1.48031571465441,-2.86265454636422,
33.6598629068856));
#21303=CARTESIAN_POINT('Ctrl Pts',(-1.47778642730061,-2.86396105806136,
33.6600398669396));
#21304=CARTESIAN_POINT('Ctrl Pts',(-1.47525540501188,-2.8652642203614,33.660216611122));
#21305=CARTESIAN_POINT('Origin',(0.,0.,4.68922655072688));
#21306=CARTESIAN_POINT('',(-1.47525552646581,-2.8652641578277,35.1563175586878));
#21307=CARTESIAN_POINT('',(-1.47525540445791,-2.86526422064663,34.9063554765866));
#21308=CARTESIAN_POINT('',(-1.47525540501186,-2.86526422036142,4.68922655072688));
#21309=CARTESIAN_POINT('',(3.22274903069615,-0.00249952936660396,34.3127207581881));
#21310=CARTESIAN_POINT('Ctrl Pts',(-1.47525552646581,-2.8652641578277,35.1563175586878));
#21311=CARTESIAN_POINT('Ctrl Pts',(-1.5179786368742,-2.84326705694414,35.1534900287168));
#21312=CARTESIAN_POINT('Ctrl Pts',(-1.56021632410078,-2.82031103518203,
35.150632229143));
#21313=CARTESIAN_POINT('Ctrl Pts',(-1.62096631363004,-2.78551014190289,
35.146421317202));
#21314=CARTESIAN_POINT('Ctrl Pts',(-1.63988409403924,-2.7744150126229,35.1450954968172));
#21315=CARTESIAN_POINT('Ctrl Pts',(-1.6699213053194,-2.75638387962761,35.1429663459599));
#21316=CARTESIAN_POINT('Ctrl Pts',(-1.68111443427663,-2.74957151366147,
35.1421675300128));
#21317=CARTESIAN_POINT('Ctrl Pts',(-1.70084704537755,-2.73739631176315,
35.1407495369148));
#21318=CARTESIAN_POINT('Ctrl Pts',(-1.70940353540863,-2.73206127107097,
35.1401313914053));
#21319=CARTESIAN_POINT('Ctrl Pts',(-1.72711415399747,-2.72090278595853,
35.1388450421301));
#21320=CARTESIAN_POINT('Ctrl Pts',(-1.73626418293619,-2.71507310288679,
35.1381766115914));
#21321=CARTESIAN_POINT('Ctrl Pts',(-1.75981505434774,-2.69990059222446,
35.1364460971715));
#21322=CARTESIAN_POINT('Ctrl Pts',(-1.77417085675511,-2.6904888005836,35.135381439547));
#21323=CARTESIAN_POINT('Ctrl Pts',(-1.83503964978362,-2.64988367822589,
35.130824774063));
#21324=CARTESIAN_POINT('Ctrl Pts',(-1.88080814757814,-2.61759700897596,
35.1272915814473));
#21325=CARTESIAN_POINT('Ctrl Pts',(-1.99924781255354,-2.52933522155223,
35.1178552546094));
#21326=CARTESIAN_POINT('Ctrl Pts',(-2.07040678604797,-2.47142503715811,
35.1118808696354));
#21327=CARTESIAN_POINT('Ctrl Pts',(-2.32202096135386,-2.24815717635066,
35.0896297664439));
#21328=CARTESIAN_POINT('Ctrl Pts',(-2.48593682768389,-2.06545269928067,
35.0727943646564));
#21329=CARTESIAN_POINT('Ctrl Pts',(-2.68002016186566,-1.7921516345158,35.0505052130097));
#21330=CARTESIAN_POINT('Ctrl Pts',(-2.72931560658516,-1.71614543216571,
35.0445815800732));
#21331=CARTESIAN_POINT('Ctrl Pts',(-2.78240414784869,-1.62620336552493,
35.0379665134103));
#21332=CARTESIAN_POINT('Ctrl Pts',(-2.7893825488052,-1.61420421283992,35.037091854403));
#21333=CARTESIAN_POINT('Ctrl Pts',(-2.79979613030385,-1.59602917237582,
35.0357792620165));
#21334=CARTESIAN_POINT('Ctrl Pts',(-2.80328877516139,-1.58988664239112,
35.0353377469127));
#21335=CARTESIAN_POINT('Ctrl Pts',(-2.80950444728965,-1.57887095232093,
35.0345497698746));
#21336=CARTESIAN_POINT('Ctrl Pts',(-2.81223503144743,-1.574002176899,35.0342028264667));
#21337=CARTESIAN_POINT('Ctrl Pts',(-2.81812494196711,-1.5634359004169,35.0334527747247));
#21338=CARTESIAN_POINT('Ctrl Pts',(-2.82127963779431,-1.55773592447216,
35.0330499638339));
#21339=CARTESIAN_POINT('Ctrl Pts',(-2.83005619289586,-1.54176412620451,
35.0319261826464));
#21340=CARTESIAN_POINT('Ctrl Pts',(-2.83563945374104,-1.53147104902214,
35.0312076395943));
#21341=CARTESIAN_POINT('Ctrl Pts',(-2.86803336675817,-1.47096639833774,
35.0270157530493));
#21342=CARTESIAN_POINT('Ctrl Pts',(-2.89356790136217,-1.42007861040143,
35.0236181149031));
#21343=CARTESIAN_POINT('Ctrl Pts',(-3.02542968025674,-1.138947318291,35.0053923346017));
#21344=CARTESIAN_POINT('Ctrl Pts',(-3.10565204760635,-0.897428543206136,
34.9916298287095));
#21345=CARTESIAN_POINT('Ctrl Pts',(-3.18966930973458,-0.488757482110987,
34.9680616591426));
#21346=CARTESIAN_POINT('Ctrl Pts',(-3.21035909838568,-0.326279391726797,
34.9586348844414));
#21347=CARTESIAN_POINT('Ctrl Pts',(-3.21973544117005,-0.141070877135228,
34.9474808597557));
#21348=CARTESIAN_POINT('Ctrl Pts',(-3.22061982517785,-0.119185606911457,
34.9461567220849));
#21349=CARTESIAN_POINT('Ctrl Pts',(-3.22167637508481,-0.0842043726205361,
34.9440297635706));
#21350=CARTESIAN_POINT('Ctrl Pts',(-3.22199192258901,-0.0711131842581894,
34.9432314424066));
#21351=CARTESIAN_POINT('Ctrl Pts',(-3.22240918699982,-0.0479400138150561,
34.9418140219369));
#21352=CARTESIAN_POINT('Ctrl Pts',(-3.22254339392139,-0.0378587375628033,
34.9411959515001));
#21353=CARTESIAN_POINT('Ctrl Pts',(-3.22272383388549,-0.0169245308703073,
34.9399094535703));
#21354=CARTESIAN_POINT('Ctrl Pts',(-3.22276255398095,-0.00607167879688278,
34.9392407977888));
#21355=CARTESIAN_POINT('Ctrl Pts',(-3.22272096316074,0.0219632680854339,
34.9375090447834));
#21356=CARTESIAN_POINT('Ctrl Pts',(-3.22255806208995,0.0391447259466706,
34.9364433668175));
#21357=CARTESIAN_POINT('Ctrl Pts',(-3.22127641534352,0.112467131535375,
34.931876414891));
#21358=CARTESIAN_POINT('Ctrl Pts',(-3.21882795275129,0.168572151615786,
34.9283337245431));
#21359=CARTESIAN_POINT('Ctrl Pts',(-3.20850071668411,0.316407724861215,
34.9188655845864));
#21360=CARTESIAN_POINT('Ctrl Pts',(-3.19815547125634,0.407908995153394,
34.9128682853862));
#21361=CARTESIAN_POINT('Ctrl Pts',(-3.14655836853488,0.737236912508392,
34.8908150037665));
#21362=CARTESIAN_POINT('Ctrl Pts',(-3.08255485188429,0.970664025651237,
34.8742217351011));
#21363=CARTESIAN_POINT('Ctrl Pts',(-2.95853734549217,1.28135465067181,34.8519555482104));
#21364=CARTESIAN_POINT('Ctrl Pts',(-2.9202214309433,1.36642720062402,34.8458487216998));
#21365=CARTESIAN_POINT('Ctrl Pts',(-2.87198078471137,1.46220351821693,34.8390556949436));
#21366=CARTESIAN_POINT('Ctrl Pts',(-2.86561476281879,1.47464056779452,34.8381752450757));
#21367=CARTESIAN_POINT('Ctrl Pts',(-2.85589862950396,1.49332206248369,34.8368556904724));
#21368=CARTESIAN_POINT('Ctrl Pts',(-2.85260857298831,1.49959731124572,34.836412948579));
#21369=CARTESIAN_POINT('Ctrl Pts',(-2.84668878298526,1.51079836932837,34.8356236486531));
#21370=CARTESIAN_POINT('Ctrl Pts',(-2.84406692746556,1.51572822551384,34.8352766022834));
#21371=CARTESIAN_POINT('Ctrl Pts',(-2.83836494384229,1.52638273865082,34.8345273123887));
#21372=CARTESIAN_POINT('Ctrl Pts',(-2.83528031325231,1.53210488098275,34.8341253610044));
#21373=CARTESIAN_POINT('Ctrl Pts',(-2.82662178978973,1.54805116811146,34.8330064032023));
#21374=CARTESIAN_POINT('Ctrl Pts',(-2.82100969894211,1.55825461646311,34.8322917904595));
#21375=CARTESIAN_POINT('Ctrl Pts',(-2.78816334376455,1.61721413353522,34.828169109464));
#21376=CARTESIAN_POINT('Ctrl Pts',(-2.75971890279074,1.66528941530197,34.8248338584807));
#21377=CARTESIAN_POINT('Ctrl Pts',(-2.59485495346103,1.92809660837726,34.806611540719));
#21378=CARTESIAN_POINT('Ctrl Pts',(-2.43462180274939,2.12684576768699,34.7928077704821));
#21379=CARTESIAN_POINT('Ctrl Pts',(-2.13546398142824,2.41924988661233,34.7691793709168));
#21380=CARTESIAN_POINT('Ctrl Pts',(-2.00971121895142,2.52468350588945,34.7597358335645));
#21381=CARTESIAN_POINT('Ctrl Pts',(-1.85865160309898,2.6328717424318,34.7485606173765));
#21382=CARTESIAN_POINT('Ctrl Pts',(-1.84067598858579,2.64546995112959,34.7472336376699));
#21383=CARTESIAN_POINT('Ctrl Pts',(-1.81176215150119,2.66529685266751,34.7451029764889));
#21384=CARTESIAN_POINT('Ctrl Pts',(-1.80090588407834,2.67264427022651,34.7443038197812));
#21385=CARTESIAN_POINT('Ctrl Pts',(-1.78161939419822,2.68552631557019,34.7428854321714));
#21386=CARTESIAN_POINT('Ctrl Pts',(-1.77320740509473,2.69108802387602,34.7422672348207));
#21387=CARTESIAN_POINT('Ctrl Pts',(-1.75569344848455,2.70254985767915,34.7409809872404));
#21388=CARTESIAN_POINT('Ctrl Pts',(-1.74658753157699,2.70844368747574,34.7403127112793));
#21389=CARTESIAN_POINT('Ctrl Pts',(-1.72300384022498,2.72353990556162,34.7385830469685));
#21390=CARTESIAN_POINT('Ctrl Pts',(-1.70848217389009,2.73267277473435,34.7375190896748));
#21391=CARTESIAN_POINT('Ctrl Pts',(-1.64633024919451,2.77107188781397,34.7329694710051));
#21392=CARTESIAN_POINT('Ctrl Pts',(-1.59801811703694,2.79921063210115,34.7294427831501));
#21393=CARTESIAN_POINT('Ctrl Pts',(-1.46878126175548,2.87004663105121,34.7200282214757));
#21394=CARTESIAN_POINT('Ctrl Pts',(-1.38673240735123,2.91057671298835,34.7140695049439));
#21395=CARTESIAN_POINT('Ctrl Pts',(-1.07752064500466,3.04727510124331,34.6917090704481));
#21396=CARTESIAN_POINT('Ctrl Pts',(-0.841289158798219,3.12076164626857,
34.6747360586032));
#21397=CARTESIAN_POINT('Ctrl Pts',(-0.511487963635961,3.18314790046483,
34.6524296120023));
#21398=CARTESIAN_POINT('Ctrl Pts',(-0.423315214009551,3.19606912650404,
34.6466057424536));
#21399=CARTESIAN_POINT('Ctrl Pts',(-0.320958914875676,3.20675757697304,
34.6400878871736));
#21400=CARTESIAN_POINT('Ctrl Pts',(-0.307196072076568,3.20810526198146,
34.6392165556126));
#21401=CARTESIAN_POINT('Ctrl Pts',(-0.286399184222595,3.21000667291289,
34.6379079656637));
#21402=CARTESIAN_POINT('Ctrl Pts',(-0.279371504714646,3.2106259354637,34.63746715723));
#21403=CARTESIAN_POINT('Ctrl Pts',(-0.266780355377734,3.21169378307977,
34.6366799401552));
#21404=CARTESIAN_POINT('Ctrl Pts',(-0.261217723788742,3.21215099530102,
34.6363330539973));
#21405=CARTESIAN_POINT('Ctrl Pts',(-0.249151434329551,3.21311121403159,
34.6355825540068));
#21406=CARTESIAN_POINT('Ctrl Pts',(-0.2426474483865,3.21360892588635,34.6351792407081));
#21407=CARTESIAN_POINT('Ctrl Pts',(-0.224426021197621,3.21494767094675,
34.6340526372061));
#21408=CARTESIAN_POINT('Ctrl Pts',(-0.212705285095834,3.21574439865924,
34.6333317939887));
#21409=CARTESIAN_POINT('Ctrl Pts',(-0.143531063224039,3.22006672147503,
34.6290986971581));
#21410=CARTESIAN_POINT('Ctrl Pts',(-0.0859918400459616,3.22211688353137,
34.6256638969262));
#21411=CARTESIAN_POINT('Ctrl Pts',(0.224690982271083,3.22485720710771,34.6074355426114));
#21412=CARTESIAN_POINT('Ctrl Pts',(0.477210918067906,3.19726231678148,34.5936972384264));
#21413=CARTESIAN_POINT('Ctrl Pts',(0.882997323517739,3.10372099632879,34.5701722845915));
#21414=CARTESIAN_POINT('Ctrl Pts',(1.03903925025733,3.05502133960133,34.5607635991275));
#21415=CARTESIAN_POINT('Ctrl Pts',(1.21110359190262,2.98660799894657,34.5496268051806));
#21416=CARTESIAN_POINT('Ctrl Pts',(1.23141426288627,2.97829114197304,34.5483000212053));
#21417=CARTESIAN_POINT('Ctrl Pts',(1.26371703297937,2.96467681913491,34.5461696150097));
#21418=CARTESIAN_POINT('Ctrl Pts',(1.27576472674439,2.95951241514302,34.5453705158263));
#21419=CARTESIAN_POINT('Ctrl Pts',(1.29702459954135,2.9502451495681,34.5439521948226));
#21420=CARTESIAN_POINT('Ctrl Pts',(1.30624970885962,2.94617225375542,34.5433340062312));
#21421=CARTESIAN_POINT('Ctrl Pts',(1.31567272496999,2.94195902417196,34.5426997017919));
#21422=CARTESIAN_POINT('Ctrl Pts',(1.31588997109556,2.94186185996344,34.5426850764488));
#21423=CARTESIAN_POINT('Ctrl Pts',(1.31629475420398,2.94168076527172,34.5426578229276));
#21424=CARTESIAN_POINT('Ctrl Pts',(1.31648229330338,2.9415968411957,34.5426451950033));
#21425=CARTESIAN_POINT('Ctrl Pts',(1.31683173916775,2.94144042344731,34.5426216629428));
#21426=CARTESIAN_POINT('Ctrl Pts',(1.31699364873046,2.94136793400149,34.5426107589135));
#21427=CARTESIAN_POINT('Ctrl Pts',(1.31729535455267,2.94123282567668,34.5425904384942));
#21428=CARTESIAN_POINT('Ctrl Pts',(1.31743515342947,2.94117020970759,34.5425810221479));
#21429=CARTESIAN_POINT('Ctrl Pts',(1.31769567254005,2.94105350080004,34.5425634733212));
#21430=CARTESIAN_POINT('Ctrl Pts',(1.31781639534897,2.94099940974958,34.5425553408311));
#21431=CARTESIAN_POINT('Ctrl Pts',(1.31804137848477,2.94089858719322,34.5425401839488));
#21432=CARTESIAN_POINT('Ctrl Pts',(1.31814564144904,2.94085185677228,34.542533159501));
#21433=CARTESIAN_POINT('Ctrl Pts',(1.31833996008483,2.94076475119691,34.5425200671157));
#21434=CARTESIAN_POINT('Ctrl Pts',(1.31843001851718,2.94072437649475,34.5425139990832));
#21435=CARTESIAN_POINT('Ctrl Pts',(1.31862851262776,2.9406353773132,34.5425006241901));
#21436=CARTESIAN_POINT('Ctrl Pts',(1.31873694992053,2.94058674987464,34.5424933171002));
#21437=CARTESIAN_POINT('Ctrl Pts',(1.31895027736526,2.94049107149664,34.5424789411808));
#21438=CARTESIAN_POINT('Ctrl Pts',(1.31905516160011,2.94044402367551,34.5424718727752));
#21439=CARTESIAN_POINT('Ctrl Pts',(1.3192615000385,2.94035145337773,34.5424579664067));
#21440=CARTESIAN_POINT('Ctrl Pts',(1.31936295515624,2.94030593092374,34.5424511284054));
#21441=CARTESIAN_POINT('Ctrl Pts',(1.31956255669724,2.94021635820134,34.5424376747366));
#21442=CARTESIAN_POINT('Ctrl Pts',(1.31966070412971,2.94017230788393,34.5424310590229));
#21443=CARTESIAN_POINT('Ctrl Pts',(1.31985380705667,2.94008562823101,34.5424180421238));
#21444=CARTESIAN_POINT('Ctrl Pts',(1.3199487636481,2.94004299878011,34.5424116408848));
#21445=CARTESIAN_POINT('Ctrl Pts',(1.32013559730026,2.93995911151546,34.5423990454179));
#21446=CARTESIAN_POINT('Ctrl Pts',(1.32022747551323,2.93991785353631,34.5423928511312));
#21447=CARTESIAN_POINT('Ctrl Pts',(1.3204082604511,2.93983666174328,34.5423806623413));
#21448=CARTESIAN_POINT('Ctrl Pts',(1.32049716845465,2.93979672768375,34.5423746677694));
#21449=CARTESIAN_POINT('Ctrl Pts',(1.32067211699855,2.93971813798157,34.5423628714479));
#21450=CARTESIAN_POINT('Ctrl Pts',(1.32075815890107,2.93967948203387,34.5423570696229));
#21451=CARTESIAN_POINT('Ctrl Pts',(1.32092747520156,2.93960340455824,34.542345652104));
#21452=CARTESIAN_POINT('Ctrl Pts',(1.3210107511155,2.93956598263577,34.5423400363233));
#21453=CARTESIAN_POINT('Ctrl Pts',(1.32117463172044,2.9394923307955,34.5423289844459));
#21454=CARTESIAN_POINT('Ctrl Pts',(1.32125523799563,2.9394561004335,34.5423235482569));
#21455=CARTESIAN_POINT('Ctrl Pts',(1.32141387197333,2.93938479086568,34.5423128493576));
#21456=CARTESIAN_POINT('Ctrl Pts',(1.3214919013374,2.93934971116318,34.5423075865486));
#21457=CARTESIAN_POINT('Ctrl Pts',(1.3216454634901,2.93928066679447,34.5422972289189));
#21458=CARTESIAN_POINT('Ctrl Pts',(1.3217209981069,2.93924670154207,34.542292133988));
#21459=CARTESIAN_POINT('Ctrl Pts',(1.3218696909511,2.93917983272141,34.5422821040443));
#21460=CARTESIAN_POINT('Ctrl Pts',(1.32194283000676,2.93914693799495,34.542277170337));
#21461=CARTESIAN_POINT('Ctrl Pts',(1.32208678870919,2.9390821852495,34.5422674590326));
#21462=CARTESIAN_POINT('Ctrl Pts',(1.32215760841277,2.93905032740962,34.5422626814427));
#21463=CARTESIAN_POINT('Ctrl Pts',(1.32229700782549,2.93898761332045,34.5422532770486));
#21464=CARTESIAN_POINT('Ctrl Pts',(1.3223655876245,2.93895675722216,34.5422486502487));
#21465=CARTESIAN_POINT('Ctrl Pts',(1.32250058381878,2.93889601272373,34.5422395422978));
#21466=CARTESIAN_POINT('Ctrl Pts',(1.32256700024262,2.9388661244898,34.5422350611546));
#21467=CARTESIAN_POINT('Ctrl Pts',(1.33311176898568,2.93412041483154,34.5415235780819));
#21468=CARTESIAN_POINT('Ctrl Pts',(1.34356471549355,2.92934863871387,34.540814648167));
#21469=CARTESIAN_POINT('Ctrl Pts',(1.37246739732528,2.9159673044564,34.5388441983968));
#21470=CARTESIAN_POINT('Ctrl Pts',(1.39086115781958,2.90723877353556,34.5375785684478));
#21471=CARTESIAN_POINT('Ctrl Pts',(1.43171135774812,2.88737741563289,34.534741268517));
#21472=CARTESIAN_POINT('Ctrl Pts',(1.45412292327897,2.87615580575706,34.5331665602155));
#21473=CARTESIAN_POINT('Ctrl Pts',(1.52313576622269,2.84058784527043,34.5282603735897));
#21474=CARTESIAN_POINT('Ctrl Pts',(1.56927196686695,2.81536264999635,34.5248987128684));
#21475=CARTESIAN_POINT('Ctrl Pts',(1.74957968961034,2.71096932119611,34.5114304655076));
#21476=CARTESIAN_POINT('Ctrl Pts',(1.87853929317941,2.62325443148371,34.5010420051069));
#21477=CARTESIAN_POINT('Ctrl Pts',(2.17973946380182,2.38475215573849,34.4751049975089));
#21478=CARTESIAN_POINT('Ctrl Pts',(2.34326390700389,2.22428327706668,34.4594586098844));
#21479=CARTESIAN_POINT('Ctrl Pts',(2.50360585802273,2.02944428320449,34.443311334839));
#21480=CARTESIAN_POINT('Ctrl Pts',(2.51855678428998,2.01086006328894,34.4417972879391));
#21481=CARTESIAN_POINT('Ctrl Pts',(2.53883459739856,1.98507344998785,34.4397340726004));
#21482=CARTESIAN_POINT('Ctrl Pts',(2.54433939956032,1.97801282583329,34.4391729631644));
#21483=CARTESIAN_POINT('Ctrl Pts',(2.55306660819457,1.96672233149081,34.4382818971493));
#21484=CARTESIAN_POINT('Ctrl Pts',(2.55630804374984,1.96250733030496,34.4379506075629));
#21485=CARTESIAN_POINT('Ctrl Pts',(2.5630058776689,1.95375305104818,34.4372654012395));
#21486=CARTESIAN_POINT('Ctrl Pts',(2.56646065984225,1.94921260907553,34.4369116067553));
#21487=CARTESIAN_POINT('Ctrl Pts',(2.57470967460473,1.93831140353089,34.4360659227143));
#21488=CARTESIAN_POINT('Ctrl Pts',(2.57949245926113,1.9319419404734,34.4355748371941));
#21489=CARTESIAN_POINT('Ctrl Pts',(2.59576009918418,1.91010943970282,34.4339016621769));
#21490=CARTESIAN_POINT('Ctrl Pts',(2.60713018343652,1.89456084951831,34.4327273145807));
#21491=CARTESIAN_POINT('Ctrl Pts',(2.67097802574282,1.8055855418721,34.4260987947794));
#21492=CARTESIAN_POINT('Ctrl Pts',(2.72049729680197,1.73007522473557,34.4208242942289));
#21493=CARTESIAN_POINT('Ctrl Pts',(2.88656355252998,1.45204330706498,34.4022542725769));
#21494=CARTESIAN_POINT('Ctrl Pts',(2.98418871767681,1.23907513865428,34.3895292051052));
#21495=CARTESIAN_POINT('Ctrl Pts',(3.07801820237266,0.957061803149152,34.3726252674123));
#21496=CARTESIAN_POINT('Ctrl Pts',(3.09630667715089,0.896129295454213,34.3689737956609));
#21497=CARTESIAN_POINT('Ctrl Pts',(3.13389207215579,0.755964727717972,34.3605307986982));
#21498=CARTESIAN_POINT('Ctrl Pts',(3.15200826748489,0.676464634466203,34.3557105247701));
#21499=CARTESIAN_POINT('Ctrl Pts',(3.17082219257112,0.576550803667215,34.3495760843915));
#21500=CARTESIAN_POINT('Ctrl Pts',(3.17436763943063,0.556699440708546,34.3483536059036));
#21501=CARTESIAN_POINT('Ctrl Pts',(3.17966402239292,0.525347092388165,34.3464166042813));
#21502=CARTESIAN_POINT('Ctrl Pts',(3.18153942383196,0.513867445738512,34.3457060511851));
#21503=CARTESIAN_POINT('Ctrl Pts',(3.1848887561866,0.492644172432872,34.3443898598164));
#21504=CARTESIAN_POINT('Ctrl Pts',(3.18638022699749,0.482903422517895,34.343784787708));
#21505=CARTESIAN_POINT('Ctrl Pts',(3.18922158457901,0.463760148369837,34.3425936596155));
#21506=CARTESIAN_POINT('Ctrl Pts',(3.19057462295564,0.45435818801226,34.3420077105624));
#21507=CARTESIAN_POINT('Ctrl Pts',(3.19350633385335,0.433327336422162,34.3406948654309));
#21508=CARTESIAN_POINT('Ctrl Pts',(3.19506308599622,0.42169557204803,34.3399672814295));
#21509=CARTESIAN_POINT('Ctrl Pts',(3.1988005096575,0.392560785323828,34.3381410688746));
#21510=CARTESIAN_POINT('Ctrl Pts',(3.20090106324127,0.375048042408418,34.3370399251383));
#21511=CARTESIAN_POINT('Ctrl Pts',(3.2162032193755,0.237962742477789,34.3283928718386));
#21512=CARTESIAN_POINT('Ctrl Pts',(3.22284231002605,0.117769459684636,34.320641953786));
#21513=CARTESIAN_POINT('Ctrl Pts',(3.22274903069615,-0.00249952936660396,
34.3127207581881));
#21514=CARTESIAN_POINT('Ctrl Pts',(3.22274903383091,-0.00249548431075094,
34.3127210246048));
#21515=CARTESIAN_POINT('Ctrl Pts',(3.22268950634448,-0.0793712028058863,
34.3076578131117));
#21516=CARTESIAN_POINT('Ctrl Pts',(3.21987931323977,-0.156217567601901,
34.3025303727163));
#21517=CARTESIAN_POINT('Ctrl Pts',(3.19547714771155,-0.493017212895797,
34.2798330297308));
#21518=CARTESIAN_POINT('Ctrl Pts',(3.14512276324906,-0.749903483919484,
34.2618427002657));
#21519=CARTESIAN_POINT('Ctrl Pts',(3.05768831627768,-1.01839253467862,34.2438188480235));
#21520=CARTESIAN_POINT('Ctrl Pts',(3.05081570427129,-1.03879968789257,34.2424545719402));
#21521=CARTESIAN_POINT('Ctrl Pts',(3.04100169487757,-1.06700310258475,34.2405784727192));
#21522=CARTESIAN_POINT('Ctrl Pts',(3.03823401117646,-1.07485860752131,34.2400569377746));
#21523=CARTESIAN_POINT('Ctrl Pts',(3.03349591789615,-1.08814218853226,34.2391768560884));
#21524=CARTESIAN_POINT('Ctrl Pts',(3.03154132825663,-1.09357582415768,34.2388173795929));
#21525=CARTESIAN_POINT('Ctrl Pts',(3.02778667665852,-1.10392609148478,34.2381336619764));
#21526=CARTESIAN_POINT('Ctrl Pts',(3.02598922875553,-1.10884361530394,34.2378092631707));
#21527=CARTESIAN_POINT('Ctrl Pts',(3.02123293376603,-1.1217583660426,34.2369584146775));
#21528=CARTESIAN_POINT('Ctrl Pts',(3.01825429336274,-1.12974833318804,34.2364331420981));
#21529=CARTESIAN_POINT('Ctrl Pts',(3.00775757135357,-1.15756712588858,34.2346078981426));
#21530=CARTESIAN_POINT('Ctrl Pts',(3.00007532909418,-1.17733399413061,34.2333173609062));
#21531=CARTESIAN_POINT('Ctrl Pts',(2.89878571381708,-1.43052738545369,34.2168519096544));
#21532=CARTESIAN_POINT('Ctrl Pts',(2.77834642053627,-1.65233126494079,34.2030944086737));
#21533=CARTESIAN_POINT('Ctrl Pts',(2.56374626208711,-1.95649825046023,34.1822393187374));
#21534=CARTESIAN_POINT('Ctrl Pts',(2.4886974495452,-2.05111249664109,34.1754271339013));
#21535=CARTESIAN_POINT('Ctrl Pts',(2.36751379097276,-2.18741988250985,34.1648665552193));
#21536=CARTESIAN_POINT('Ctrl Pts',(2.32518847037112,-2.23235866016078,34.161250204236));
#21537=CARTESIAN_POINT('Ctrl Pts',(2.25222757386477,-2.30549740826488,34.1551086869342));
#21538=CARTESIAN_POINT('Ctrl Pts',(2.22228822264614,-2.3343697561343,34.1526129566688));
#21539=CARTESIAN_POINT('Ctrl Pts',(2.18071636178537,-2.37293536823143,34.1491756555924));
#21540=CARTESIAN_POINT('Ctrl Pts',(2.16956113449442,-2.38313880919625,34.1482559879938));
#21541=CARTESIAN_POINT('Ctrl Pts',(2.15141039797253,-2.39950782501703,34.1467636921517));
#21542=CARTESIAN_POINT('Ctrl Pts',(2.14445911070324,-2.40572226627519,34.146193138504));
#21543=CARTESIAN_POINT('Ctrl Pts',(2.12993388445581,-2.41859482021741,34.1450028561489));
#21544=CARTESIAN_POINT('Ctrl Pts',(2.12235547675775,-2.4252477158267,34.1443829181036));
#21545=CARTESIAN_POINT('Ctrl Pts',(2.10485433732945,-2.44046668035701,34.1429536725555));
#21546=CARTESIAN_POINT('Ctrl Pts',(2.09491036727475,-2.44900795103457,34.1421433482938));
#21547=CARTESIAN_POINT('Ctrl Pts',(2.06817704819276,-2.47168829963303,34.1399693918505));
#21548=CARTESIAN_POINT('Ctrl Pts',(2.051295125002,-2.48571672256823,34.1386012572402));
#21549=CARTESIAN_POINT('Ctrl Pts',(1.90719021310976,-2.6029962413126,34.1269603572193));
#21550=CARTESIAN_POINT('Ctrl Pts',(1.77242687335144,-2.69656304193151,34.116300449036));
#21551=CARTESIAN_POINT('Ctrl Pts',(1.41181132049793,-2.90819308711693,34.0884122781505));
#21552=CARTESIAN_POINT('Ctrl Pts',(1.1780151099184,-3.01049395687655,34.0708561732097));
#21553=CARTESIAN_POINT('Ctrl Pts',(0.881064106395242,-3.10048002765734,
34.0505612559151));
#21554=CARTESIAN_POINT('Ctrl Pts',(0.827080387910012,-3.11531528010423,
34.0469523067093));
#21555=CARTESIAN_POINT('Ctrl Pts',(0.761421516496155,-3.1315316721138,34.0426815383601));
#21556=CARTESIAN_POINT('Ctrl Pts',(0.750093829549569,-3.1342642830331,34.041948964279));
#21557=CARTESIAN_POINT('Ctrl Pts',(0.732422321404646,-3.13842594050333,
34.0408129829799));
#21558=CARTESIAN_POINT('Ctrl Pts',(0.726088711568406,-3.13989729539397,
34.0404072063414));
#21559=CARTESIAN_POINT('Ctrl Pts',(0.714308106891325,-3.14259648490657,
34.0396550532596));
#21560=CARTESIAN_POINT('Ctrl Pts',(0.708862427310016,-3.14382932080825,
34.0393084004734));
#21561=CARTESIAN_POINT('Ctrl Pts',(0.696501187692453,-3.1465940042048,34.0385238530142));
#21562=CARTESIAN_POINT('Ctrl Pts',(0.689583781090896,-3.14811720602539,
34.0380864587749));
#21563=CARTESIAN_POINT('Ctrl Pts',(0.669017730390513,-3.1525747781179,34.0367907708732));
#21564=CARTESIAN_POINT('Ctrl Pts',(0.655354772481322,-3.15544332760685,
34.0359361578871));
#21565=CARTESIAN_POINT('Ctrl Pts',(0.550616301565407,-3.17672361120095,
34.0294289845426));
#21566=CARTESIAN_POINT('Ctrl Pts',(0.458792277435907,-3.19127942205414,
34.0239790548164));
#21567=CARTESIAN_POINT('Ctrl Pts',(0.126334080150407,-3.22933003436166,
34.0047486253465));
#21568=CARTESIAN_POINT('Ctrl Pts',(-0.116127361853904,-3.22971513974557,
33.9916057746218));
#21569=CARTESIAN_POINT('Ctrl Pts',(-0.447806915516332,-3.19281253952173,
33.9726072663028));
#21570=CARTESIAN_POINT('Ctrl Pts',(-0.538766487281882,-3.1787279978541,
33.9672968283315));
#21571=CARTESIAN_POINT('Ctrl Pts',(-0.684048714342601,-3.14981681050214,
33.9585622101595));
#21572=CARTESIAN_POINT('Ctrl Pts',(-0.738804759303616,-3.13742498452496,
33.9552116788161));
#21573=CARTESIAN_POINT('Ctrl Pts',(-0.809858678038751,-3.11938161277064,
33.9507755535829));
#21574=CARTESIAN_POINT('Ctrl Pts',(-0.826476112126096,-3.11502005495813,
33.9497317183468));
#21575=CARTESIAN_POINT('Ctrl Pts',(-0.853532251035079,-3.10768692701975,
33.9480214601672));
#21576=CARTESIAN_POINT('Ctrl Pts',(-0.863992360011152,-3.1047950877977,
33.9473576372978));
#21577=CARTESIAN_POINT('Ctrl Pts',(-0.884141689813732,-3.09911482343423,
33.9460737612706));
#21578=CARTESIAN_POINT('Ctrl Pts',(-0.893832836294111,-3.09633365023407,
33.9454539515525));
#21579=CARTESIAN_POINT('Ctrl Pts',(-0.916081501794201,-3.08983555388284,
33.9440256226661));
#21580=CARTESIAN_POINT('Ctrl Pts',(-0.928629669906202,-3.08608749001063,
33.9432160909879));
#21581=CARTESIAN_POINT('Ctrl Pts',(-0.962105929169504,-3.07586567213532,
33.9410456427013));
#21582=CARTESIAN_POINT('Ctrl Pts',(-0.982991155717204,-3.0692549261134,
33.9396802464519));
#21583=CARTESIAN_POINT('Ctrl Pts',(-1.15955612529272,-3.01138028586811,
33.9280391039708));
#21584=CARTESIAN_POINT('Ctrl Pts',(-1.31115926822677,-2.94852985574958,
33.9173759002481));
#21585=CARTESIAN_POINT('Ctrl Pts',(-1.46330007080683,-2.87139610820017,
33.9059988892074));
#21586=CARTESIAN_POINT('Ctrl Pts',(-1.46928281327957,-2.86833936373547,
33.9055504022586));
#21587=CARTESIAN_POINT('Ctrl Pts',(-1.47525541125577,-2.86526421714657,
33.905101584668));
#21588=CARTESIAN_POINT('Ctrl Pts',(-1.47525540501188,-2.8652642203614,33.660216611122));
#21589=CARTESIAN_POINT('Ctrl Pts',(-1.4728255803023,-2.86651527846996,33.6603862885616));
#21590=CARTESIAN_POINT('Ctrl Pts',(-1.47039415665903,-2.8677632496416,33.6605557677759));
#21591=CARTESIAN_POINT('Ctrl Pts',(-1.46167854320598,-2.8722226938255,33.6611621794057));
#21592=CARTESIAN_POINT('Ctrl Pts',(-1.45538535560231,-2.87541663686004,
33.661598000429));
#21593=CARTESIAN_POINT('Ctrl Pts',(-1.43671419720623,-2.88481569470146,
33.6628851366076));
#21594=CARTESIAN_POINT('Ctrl Pts',(-1.42430648638582,-2.89096183400143,
33.6637328414822));
#21595=CARTESIAN_POINT('Ctrl Pts',(-1.33126250157591,-2.93630658633081,
33.6700355573838));
#21596=CARTESIAN_POINT('Ctrl Pts',(-1.24905349074832,-2.97220873530523,
33.6753020303906));
#21597=CARTESIAN_POINT('Ctrl Pts',(-0.936276528111629,-3.09352942048674,
33.6946120711626));
#21598=CARTESIAN_POINT('Ctrl Pts',(-0.6976818284038,-3.15591384426281,33.7079655080248));
#21599=CARTESIAN_POINT('Ctrl Pts',(-0.363631015283433,-3.20347904668118,
33.7271781807225));
#21600=CARTESIAN_POINT('Ctrl Pts',(-0.272456666410673,-3.21251785526814,
33.7324653244585));
#21601=CARTESIAN_POINT('Ctrl Pts',(-0.125168380193548,-3.22080430612031,
33.7411648944585));
#21602=CARTESIAN_POINT('Ctrl Pts',(-0.0692412687039754,-3.22249167207284,
33.7445044316557));
#21603=CARTESIAN_POINT('Ctrl Pts',(0.00385470494090011,-3.22279335776465,
33.7489277989379));
#21604=CARTESIAN_POINT('Ctrl Pts',(0.0210104335126121,-3.22272717268788,
33.7499701676234));
#21605=CARTESIAN_POINT('Ctrl Pts',(0.0490084758830552,-3.22239559004677,
33.7516784751288));
#21606=CARTESIAN_POINT('Ctrl Pts',(0.0598515659565342,-3.22221243169464,
33.7523418236397));
#21607=CARTESIAN_POINT('Ctrl Pts',(0.0807712680053874,-3.22175343200752,
33.7536250993456));
#21608=CARTESIAN_POINT('Ctrl Pts',(0.090847929069417,-3.22148503403112,
33.7542447849867));
#21609=CARTESIAN_POINT('Ctrl Pts',(0.114017320656081,-3.22075910938433,
33.7556732816598));
#21610=CARTESIAN_POINT('Ctrl Pts',(0.127108784992515,-3.22026901651443,
33.7564831076047));
#21611=CARTESIAN_POINT('Ctrl Pts',(0.162106333256662,-3.21874510321659,
33.7586553500724));
#21612=CARTESIAN_POINT('Ctrl Pts',(0.184005162566524,-3.21756749183474,
33.7600222597301));
#21613=CARTESIAN_POINT('Ctrl Pts',(0.370772083119689,-3.20561120434231,
33.7717476540309));
#21614=CARTESIAN_POINT('Ctrl Pts',(0.534572270148137,-3.1823941588063,33.7825001276244));
#21615=CARTESIAN_POINT('Ctrl Pts',(0.946774793484743,-3.09124199611811,
33.8106669531751));
#21616=CARTESIAN_POINT('Ctrl Pts',(1.19014951736551,-3.00594405680605,33.8284144525443));
#21617=CARTESIAN_POINT('Ctrl Pts',(1.46783231030705,-2.86955237620585,33.8486081438843));
#21618=CARTESIAN_POINT('Ctrl Pts',(1.51429135732856,-2.84530929170618,33.8519810455534));
#21619=CARTESIAN_POINT('Ctrl Pts',(1.5701368502739,-2.81441260636867,33.8560100276764));
#21620=CARTESIAN_POINT('Ctrl Pts',(1.58010281171686,-2.8088295001861,33.8567280166059));
#21621=CARTESIAN_POINT('Ctrl Pts',(1.59564990909331,-2.80001081084744,33.857846259732));
#21622=CARTESIAN_POINT('Ctrl Pts',(1.60125125696268,-2.79681132489487,33.8582487683439));
#21623=CARTESIAN_POINT('Ctrl Pts',(1.61168646774392,-2.79080911428948,33.8589978790069));
#21624=CARTESIAN_POINT('Ctrl Pts',(1.61652259638009,-2.78801066689778,33.859344738483));
#21625=CARTESIAN_POINT('Ctrl Pts',(1.62753129229085,-2.7816021616959,33.8601336273992));
#21626=CARTESIAN_POINT('Ctrl Pts',(1.6336991261263,-2.77798413619602,33.8605751324405));
#21627=CARTESIAN_POINT('Ctrl Pts',(1.652576780305,-2.76682596804097,33.8619251009243));
#21628=CARTESIAN_POINT('Ctrl Pts',(1.66524703277727,-2.75921878280522,33.8628293142991));
#21629=CARTESIAN_POINT('Ctrl Pts',(1.78032396427632,-2.68904549225664,33.8710290424274));
#21630=CARTESIAN_POINT('Ctrl Pts',(1.8792260589973,-2.62088445911598,33.877985041915));
#21631=CARTESIAN_POINT('Ctrl Pts',(2.13890018400492,-2.41964683188631,33.8966527980937));
#21632=CARTESIAN_POINT('Ctrl Pts',(2.29091481011329,-2.27624657864255,33.9080743785994));
#21633=CARTESIAN_POINT('Ctrl Pts',(2.49068672697253,-2.04735945558316,33.9253434938951));
#21634=CARTESIAN_POINT('Ctrl Pts',(2.55013727647008,-1.97281496236439,33.9308361593201));
#21635=CARTESIAN_POINT('Ctrl Pts',(2.64005201187934,-1.84920409278532,33.9398423962547));
#21636=CARTESIAN_POINT('Ctrl Pts',(2.67265475293496,-1.8017620134296,33.943276159383));
#21637=CARTESIAN_POINT('Ctrl Pts',(2.71339795707468,-1.73893342349925,33.9478068573847));
#21638=CARTESIAN_POINT('Ctrl Pts',(2.72271001024555,-1.72431670718651,33.9488597311167));
#21639=CARTESIAN_POINT('Ctrl Pts',(2.73767700771383,-1.70040013220511,33.9505809297217));
#21640=CARTESIAN_POINT('Ctrl Pts',(2.74340361270457,-1.69114535784873,33.9512465883831));
#21641=CARTESIAN_POINT('Ctrl Pts',(2.75433675098675,-1.67327462332636,33.9525313185665));
#21642=CARTESIAN_POINT('Ctrl Pts',(2.75955001443458,-1.66466291394646,33.9531501322929));
#21643=CARTESIAN_POINT('Ctrl Pts',(2.77140988974836,-1.64486295434334,33.9545723266797));
#21644=CARTESIAN_POINT('Ctrl Pts',(2.77802921936733,-1.6336586436349,33.9553766930355));
#21645=CARTESIAN_POINT('Ctrl Pts',(2.7954707304801,-1.60372345436638,33.9575248130437));
#21646=CARTESIAN_POINT('Ctrl Pts',(2.80617233955122,-1.58492343251606,33.9588729044331));
#21647=CARTESIAN_POINT('Ctrl Pts',(2.89030821426618,-1.43359424892217,33.9697182053102));
#21648=CARTESIAN_POINT('Ctrl Pts',(2.95449189606819,-1.2961635487674,33.9795443543741));
#21649=CARTESIAN_POINT('Ctrl Pts',(3.08934605135885,-0.94479209763422,34.0045591141958));
#21650=CARTESIAN_POINT('Ctrl Pts',(3.1477224592756,-0.72699748881505,34.0200010606175));
#21651=CARTESIAN_POINT('Ctrl Pts',(3.19306994939233,-0.441126339361872,
34.039271776157));
#21652=CARTESIAN_POINT('Ctrl Pts',(3.20126891046095,-0.377049827926129,
34.0435240463447));
#21653=CARTESIAN_POINT('Ctrl Pts',(3.20989118319928,-0.288625181510789,
34.0492637700471));
#21654=CARTESIAN_POINT('Ctrl Pts',(3.21197264882183,-0.264457337145626,
34.0508193773346));
#21655=CARTESIAN_POINT('Ctrl Pts',(3.21509141407373,-0.222741217698234,
34.053479262443));
#21656=CARTESIAN_POINT('Ctrl Pts',(3.21625835328021,-0.205204016598402,
34.0545897819485));
#21657=CARTESIAN_POINT('Ctrl Pts',(3.21772861712967,-0.179997199387764,
34.056174099854));
#21658=CARTESIAN_POINT('Ctrl Pts',(3.21814808256899,-0.172335042338471,
34.0566541133346));
#21659=CARTESIAN_POINT('Ctrl Pts',(3.21882909996629,-0.159024398863697,
34.0574851697711));
#21660=CARTESIAN_POINT('Ctrl Pts',(3.21910315915259,-0.153376618015321,
34.0578369088213));
#21661=CARTESIAN_POINT('Ctrl Pts',(3.21964498638606,-0.141568850803734,
34.0585704110216));
#21662=CARTESIAN_POINT('Ctrl Pts',(3.219909941799,-0.135408810999306,34.058952015179));
#21663=CARTESIAN_POINT('Ctrl Pts',(3.22056378964949,-0.119118477070685,
34.0599584622756));
#21664=CARTESIAN_POINT('Ctrl Pts',(3.2209225676546,-0.108986945972917,34.0605816349504));
#21665=CARTESIAN_POINT('Ctrl Pts',(3.22223308702053,-0.0662825499948332,
34.0631972589008));
#21666=CARTESIAN_POINT('Ctrl Pts',(3.22273861344313,-0.0336966216181623,
34.0651660519612));
#21667=CARTESIAN_POINT('Ctrl Pts',(3.22284085997709,0.263913886241149,34.0829454412723));
#21668=CARTESIAN_POINT('Ctrl Pts',(3.19024154128433,0.527970392858009,34.0973245963946));
#21669=CARTESIAN_POINT('Ctrl Pts',(3.08206581443839,0.958653158441696,34.1223202205985));
#21670=CARTESIAN_POINT('Ctrl Pts',(3.024093633427,1.12826883321634,34.1325838388579));
#21671=CARTESIAN_POINT('Ctrl Pts',(2.94346373664055,1.31249003732423,34.1446763593646));
#21672=CARTESIAN_POINT('Ctrl Pts',(2.93436729250897,1.33270305097177,34.1460161419005));
#21673=CARTESIAN_POINT('Ctrl Pts',(2.91953522437539,1.36477289721287,34.1481633342022));
#21674=CARTESIAN_POINT('Ctrl Pts',(2.91393406513983,1.37669141178235,34.148966104497));
#21675=CARTESIAN_POINT('Ctrl Pts',(2.90391213803772,1.39768154042701,34.1503885099551));
#21676=CARTESIAN_POINT('Ctrl Pts',(2.89952148989016,1.40676740077379,34.1510070904597));
#21677=CARTESIAN_POINT('Ctrl Pts',(2.8903367502876,1.42554831850029,34.1522917617754));
#21678=CARTESIAN_POINT('Ctrl Pts',(2.88553638730329,1.43524015113331,34.1529580663957));
#21679=CARTESIAN_POINT('Ctrl Pts',(2.87305498665674,1.46012410543961,34.1546775653687));
#21680=CARTESIAN_POINT('Ctrl Pts',(2.86530227172579,1.47527971359988,34.1557332731608));
#21681=CARTESIAN_POINT('Ctrl Pts',(2.83210772836556,1.53892222832228,34.16020274183));
#21682=CARTESIAN_POINT('Ctrl Pts',(2.80555364506525,1.58681566690869,34.1636557592413));
#21683=CARTESIAN_POINT('Ctrl Pts',(2.73272738552284,1.71061948323202,34.1728256631441));
#21684=CARTESIAN_POINT('Ctrl Pts',(2.68451450764142,1.7853284128188,34.1786089104205));
#21685=CARTESIAN_POINT('Ctrl Pts',(2.48782569302961,2.06409703362566,34.2011452485164));
#21686=CARTESIAN_POINT('Ctrl Pts',(2.31868502308203,2.25243322258226,34.2185207336602));
#21687=CARTESIAN_POINT('Ctrl Pts',(2.06364001592,2.47692648334788,34.2410876256664));
#21688=CARTESIAN_POINT('Ctrl Pts',(1.99562036087461,2.53205001763297,34.2468060703505));
#21689=CARTESIAN_POINT('Ctrl Pts',(1.91439438169414,2.59256654014724,34.2532207524362));
#21690=CARTESIAN_POINT('Ctrl Pts',(1.90330110770706,2.60072144280946,34.2540882268972));
#21691=CARTESIAN_POINT('Ctrl Pts',(1.88645647656314,2.61293878463141,34.2553920859953));
#21692=CARTESIAN_POINT('Ctrl Pts',(1.88074367525935,2.617053755735,34.2558319846327));
#21693=CARTESIAN_POINT('Ctrl Pts',(1.87048017380436,2.62439566420057,34.2566181146173));
#21694=CARTESIAN_POINT('Ctrl Pts',(1.86593455715238,2.62762952351049,34.2569648189313));
#21695=CARTESIAN_POINT('Ctrl Pts',(1.85605025136268,2.6346228686724,34.2577155332949));
#21696=CARTESIAN_POINT('Ctrl Pts',(1.85070854347813,2.63837792679481,34.2581192397352));
#21697=CARTESIAN_POINT('Ctrl Pts',(1.83569472308831,2.64886415320818,34.2592484518159));
#21698=CARTESIAN_POINT('Ctrl Pts',(1.82599693378279,2.65555862792185,34.2599714910957));
#21699=CARTESIAN_POINT('Ctrl Pts',(1.76816082889255,2.69501680216037,34.2642474219768));
#21700=CARTESIAN_POINT('Ctrl Pts',(1.71917506605233,2.72652642660301,34.2677210106777));
#21701=CARTESIAN_POINT('Ctrl Pts',(1.45333332568138,2.88751105619469,34.2859467393601));
#21702=CARTESIAN_POINT('Ctrl Pts',(1.22266080426761,2.99249470690328,34.2996551499078));
#21703=CARTESIAN_POINT('Ctrl Pts',(0.826639648367929,3.11920150073874,34.3231453481257));
#21704=CARTESIAN_POINT('Ctrl Pts',(0.667670942802012,3.15704866566824,34.332551571068));
#21705=CARTESIAN_POINT('Ctrl Pts',(0.484914441452332,3.18613476437704,34.3436823160037));
#21706=CARTESIAN_POINT('Ctrl Pts',(0.463262042801261,3.18935494979522,34.3450057038783));
#21707=CARTESIAN_POINT('Ctrl Pts',(0.428613349125122,3.19414769256769,34.3471315440924));
#21708=CARTESIAN_POINT('Ctrl Pts',(0.41563712568302,3.19586211479855,34.3479295024848));
#21709=CARTESIAN_POINT('Ctrl Pts',(0.392651493811022,3.19875662437138,34.3493463293875));
#21710=CARTESIAN_POINT('Ctrl Pts',(0.382646260562462,3.19996890190581,34.3499641702262));
#21711=CARTESIAN_POINT('Ctrl Pts',(0.361858629613905,3.20238873522098,34.3512502398636));
#21712=CARTESIAN_POINT('Ctrl Pts',(0.351075505047797,3.20358881013814,34.3519186970447));
#21713=CARTESIAN_POINT('Ctrl Pts',(0.3232038226825,3.20654829435708,34.3536500400945));
#21714=CARTESIAN_POINT('Ctrl Pts',(0.306107057752536,3.20822554160638,34.3547155060354));
#21715=CARTESIAN_POINT('Ctrl Pts',(0.233069075445021,3.21480166838262,34.3592824360435));
#21716=CARTESIAN_POINT('Ctrl Pts',(0.177021192189369,3.21837440618064,34.3628253235261));
#21717=CARTESIAN_POINT('Ctrl Pts',(0.0289100688562121,3.22393516175409,
34.3722947096103));
#21718=CARTESIAN_POINT('Ctrl Pts',(-0.0631892968643576,3.22344509803694,
34.3782930945743));
#21719=CARTESIAN_POINT('Ctrl Pts',(-0.396139889156062,3.20739911314354,
34.4003459230898));
#21720=CARTESIAN_POINT('Ctrl Pts',(-0.635052964436707,3.1687582514174,34.416937439632));
#21721=CARTESIAN_POINT('Ctrl Pts',(-0.957227151273777,3.07872246075456,
34.4392030718179));
#21722=CARTESIAN_POINT('Ctrl Pts',(-1.04592751058867,3.04973031407694,34.445310912867));
#21723=CARTESIAN_POINT('Ctrl Pts',(-1.1463295606484,3.01201613809305,34.4521047022913));
#21724=CARTESIAN_POINT('Ctrl Pts',(-1.15937404031762,3.00701920995031,34.4529849721801));
#21725=CARTESIAN_POINT('Ctrl Pts',(-1.1789838577939,2.99936073164673,34.4543042204606));
#21726=CARTESIAN_POINT('Ctrl Pts',(-1.18557338442597,2.99676216739007,34.4547468348062));
#21727=CARTESIAN_POINT('Ctrl Pts',(-1.1973401612175,2.99207708067093,34.4555358873653));
#21728=CARTESIAN_POINT('Ctrl Pts',(-1.20252059043243,2.98999882098789,34.4558828137425));
#21729=CARTESIAN_POINT('Ctrl Pts',(-1.21372000588447,2.98547207841237,34.4566318148952));
#21730=CARTESIAN_POINT('Ctrl Pts',(-1.2197369765306,2.98301885570794,34.4570335978975));
#21731=CARTESIAN_POINT('Ctrl Pts',(-1.23651036056334,2.97612082167146,34.4581520078113));
#21732=CARTESIAN_POINT('Ctrl Pts',(-1.24725030549444,2.97163586296246,34.4588662437971));
#21733=CARTESIAN_POINT('Ctrl Pts',(-1.30933042849502,2.94531559422303,34.4629851525495));
#21734=CARTESIAN_POINT('Ctrl Pts',(-1.3601244415025,2.92220678523587,34.4663171541771));
#21735=CARTESIAN_POINT('Ctrl Pts',(-1.6389793450722,2.7864936606291,34.4845336149946));
#21736=CARTESIAN_POINT('Ctrl Pts',(-1.85370559745061,2.6485096302318,34.4983346524173));
#21737=CARTESIAN_POINT('Ctrl Pts',(-2.17659955859563,2.38232168211621,34.5219705142417));
#21738=CARTESIAN_POINT('Ctrl Pts',(-2.29503818044432,2.26844252967868,34.5314253652527));
#21739=CARTESIAN_POINT('Ctrl Pts',(-2.41887269397027,2.12970712156491,34.5426105021688));
#21740=CARTESIAN_POINT('Ctrl Pts',(-2.43329421195046,2.11321479624367,34.543934953249));
#21741=CARTESIAN_POINT('Ctrl Pts',(-2.45606470765608,2.0866324959153,34.5460621787147));
#21742=CARTESIAN_POINT('Ctrl Pts',(-2.46452243674701,2.0766362637765,34.5468604497816));
#21743=CARTESIAN_POINT('Ctrl Pts',(-2.4793822421309,2.05885474266377,34.5482776384994));
#21744=CARTESIAN_POINT('Ctrl Pts',(-2.4858091911122,2.05109039676444,34.5488955267275));
#21745=CARTESIAN_POINT('Ctrl Pts',(-2.49907709557057,2.03490759017481,34.5501815021643));
#21746=CARTESIAN_POINT('Ctrl Pts',(-2.50591217278991,2.02648449483665,34.5508498167971));
#21747=CARTESIAN_POINT('Ctrl Pts',(-2.52345516515957,2.00464120262812,34.5525803760308));
#21748=CARTESIAN_POINT('Ctrl Pts',(-2.5340984917923,1.99116979119174,34.5536451962752));
#21749=CARTESIAN_POINT('Ctrl Pts',(-2.57903520613856,1.93334887253686,34.5582056119943));
#21750=CARTESIAN_POINT('Ctrl Pts',(-2.61227414128307,1.88819586676661,34.561742484096));
#21751=CARTESIAN_POINT('Ctrl Pts',(-2.6968215291213,1.76683556149029,34.5711917145426));
#21752=CARTESIAN_POINT('Ctrl Pts',(-2.74607575513466,1.68926602187381,34.5771755793808));
#21753=CARTESIAN_POINT('Ctrl Pts',(-2.91358124290104,1.39873667276134,34.5993598767689));
#21754=CARTESIAN_POINT('Ctrl Pts',(-3.01090014482924,1.17468513655043,34.6161114129974));
#21755=CARTESIAN_POINT('Ctrl Pts',(-3.10878701675985,0.854357027892131,
34.6383912175558));
#21756=CARTESIAN_POINT('Ctrl Pts',(-3.13178297586233,0.76578156239024,34.6443769437342));
#21757=CARTESIAN_POINT('Ctrl Pts',(-3.15390009751464,0.662740663365961,
34.6510521895322));
#21758=CARTESIAN_POINT('Ctrl Pts',(-3.1567310133967,0.649122744523126,34.6519286477451));
#21759=CARTESIAN_POINT('Ctrl Pts',(-3.16086796299769,0.628554910666711,
34.6532433138618));
#21760=CARTESIAN_POINT('Ctrl Pts',(-3.16223938941499,0.621618533769253,
34.6536851211943));
#21761=CARTESIAN_POINT('Ctrl Pts',(-3.16465241468779,0.609199311869242,
34.6544733029363));
#21762=CARTESIAN_POINT('Ctrl Pts',(-3.16570260643867,0.60371824266424,34.6548201609968));
#21763=CARTESIAN_POINT('Ctrl Pts',(-3.16794647384673,0.591840386406922,
34.6555696606333));
#21764=CARTESIAN_POINT('Ctrl Pts',(-3.1691350119311,0.585442723125801,34.6559720069591));
#21765=CARTESIAN_POINT('Ctrl Pts',(-3.17240293322075,0.567550558853649,
34.657093577287));
#21766=CARTESIAN_POINT('Ctrl Pts',(-3.17443923746657,0.556048149832419,
34.6578103884036));
#21767=CARTESIAN_POINT('Ctrl Pts',(-3.18595801147179,0.488856137763672,
34.6619744338813));
#21768=CARTESIAN_POINT('Ctrl Pts',(-3.19403809728417,0.43293222306134,34.665347122134));
#21769=CARTESIAN_POINT('Ctrl Pts',(-3.23032081244044,0.12475387467685,34.6835656797003));
#21770=CARTESIAN_POINT('Ctrl Pts',(-3.23011976760302,-0.129959484163719,
34.6973396808747));
#21771=CARTESIAN_POINT('Ctrl Pts',(-3.18060479565052,-0.544714443388395,
34.7209335717263));
#21772=CARTESIAN_POINT('Ctrl Pts',(-3.14880858468423,-0.705659088372832,
34.7303748316575));
#21773=CARTESIAN_POINT('Ctrl Pts',(-3.09905095561747,-0.884579272956763,
34.7415447641064));
#21774=CARTESIAN_POINT('Ctrl Pts',(-3.09296751080527,-0.905620923168818,
34.742868919011));
#21775=CARTESIAN_POINT('Ctrl Pts',(-3.08290575764763,-0.939138473665273,
34.7449957585969));
#21776=CARTESIAN_POINT('Ctrl Pts',(-3.07906501170587,-0.951655204895223,
34.7457939425712));
#21777=CARTESIAN_POINT('Ctrl Pts',(-3.07213280761211,-0.973765455228551,
34.747211030499));
#21778=CARTESIAN_POINT('Ctrl Pts',(-3.06907239689361,-0.98336858215175,
34.7478289055177));
#21779=CARTESIAN_POINT('Ctrl Pts',(-3.0626246217544,-1.00327746414113,34.7491149071457));
#21780=CARTESIAN_POINT('Ctrl Pts',(-3.05923017317437,-1.01358077466077,
34.7497832614461));
#21781=CARTESIAN_POINT('Ctrl Pts',(-3.05032844770001,-1.0401484419375,34.7515140388028));
#21782=CARTESIAN_POINT('Ctrl Pts',(-3.04474313928114,-1.05638611194859,
34.7525790387347));
#21783=CARTESIAN_POINT('Ctrl Pts',(-3.02036166261241,-1.12546825988132,
34.7571412663421));
#21784=CARTESIAN_POINT('Ctrl Pts',(-3.00031839562588,-1.17785918683693,
34.7606798114443));
#21785=CARTESIAN_POINT('Ctrl Pts',(-2.94384900810734,-1.31465517888829,
34.7701346459885));
#21786=CARTESIAN_POINT('Ctrl Pts',(-2.90516325351745,-1.39806622594099,
34.7761225474268));
#21787=CARTESIAN_POINT('Ctrl Pts',(-2.75142987754299,-1.69551340725513,
34.7982722767553));
#21788=CARTESIAN_POINT('Ctrl Pts',(-2.61586033812479,-1.89799678043436,
34.8149814582973));
#21789=CARTESIAN_POINT('Ctrl Pts',(-2.3994112719973,-2.15346113835054,34.8372572014884));
#21790=CARTESIAN_POINT('Ctrl Pts',(-2.33700121942408,-2.22103535195844,
34.8432749163128));
#21791=CARTESIAN_POINT('Ctrl Pts',(-2.26190437589437,-2.2956698477108,34.8499812455905));
#21792=CARTESIAN_POINT('Ctrl Pts',(-2.25196415784003,-2.30542163251187,
34.8508587199754));
#21793=CARTESIAN_POINT('Ctrl Pts',(-2.23687916253723,-2.3200300031454,34.8521746078523));
#21794=CARTESIAN_POINT('Ctrl Pts',(-2.23178124087571,-2.32493442884553,
34.8526166304943));
#21795=CARTESIAN_POINT('Ctrl Pts',(-2.22263247016308,-2.33367812965707,
34.853405044379));
#21796=CARTESIAN_POINT('Ctrl Pts',(-2.21858777281354,-2.33752369103636,
34.8537519204768));
#21797=CARTESIAN_POINT('Ctrl Pts',(-2.20980738000018,-2.34582847095305,
34.8545012862538));
#21798=CARTESIAN_POINT('Ctrl Pts',(-2.20506818236936,-2.35028385194338,
34.8549034816138));
#21799=CARTESIAN_POINT('Ctrl Pts',(-2.19178901696946,-2.36269224545409,
34.8560242047182));
#21800=CARTESIAN_POINT('Ctrl Pts',(-2.1832191914672,-2.37061336226623,34.8567403254728));
#21801=CARTESIAN_POINT('Ctrl Pts',(-2.13305380186929,-2.4164786266356,34.8608922072046));
#21802=CARTESIAN_POINT('Ctrl Pts',(-2.09050983496426,-2.45337665240373,
34.8642539298408));
#21803=CARTESIAN_POINT('Ctrl Pts',(-1.87028138285107,-2.63448778882551,
34.8809967045372));
#21804=CARTESIAN_POINT('Ctrl Pts',(-1.67860838796915,-2.76056267662292,
34.8935046039807));
#21805=CARTESIAN_POINT('Ctrl Pts',(-1.4752554044579,-2.86526422064663,34.9063554765866));
#21806=CARTESIAN_POINT('Origin',(0.,0.,4.68922655072688));
#21807=CARTESIAN_POINT('',(-1.47525545662511,-2.865264193787,36.4017031386693));
#21808=CARTESIAN_POINT('',(-1.47525533429856,-2.86526425676998,36.1542047394732));
#21809=CARTESIAN_POINT('',(-1.47525540501186,-2.86526422036142,4.68922655072688));
#21810=CARTESIAN_POINT('Ctrl Pts',(-1.4752554566251,-2.865264193787,36.4017031386693));
#21811=CARTESIAN_POINT('Ctrl Pts',(-1.66869427635609,-2.76566720899584,
36.3893221826344));
#21812=CARTESIAN_POINT('Ctrl Pts',(-1.85161275111611,-2.64670560438004,
36.3774197811539));
#21813=CARTESIAN_POINT('Ctrl Pts',(-2.09281079697536,-2.45249159555157,
36.3597902555439));
#21814=CARTESIAN_POINT('Ctrl Pts',(-2.16192269046745,-2.39179020980833,
36.3544830894472));
#21815=CARTESIAN_POINT('Ctrl Pts',(-2.26887596446572,-2.28942515554214,
36.3457533615933));
#21816=CARTESIAN_POINT('Ctrl Pts',(-2.30838825200233,-2.24957969103573,
36.3424043407513));
#21817=CARTESIAN_POINT('Ctrl Pts',(-2.35861129851129,-2.19621614818392,
36.3379699373801));
#21818=CARTESIAN_POINT('Ctrl Pts',(-2.37028355000504,-2.183613633822,36.3369262723467));
#21819=CARTESIAN_POINT('Ctrl Pts',(-2.38916441559391,-2.16289822266887,
36.3352162229861));
#21820=CARTESIAN_POINT('Ctrl Pts',(-2.39643388059001,-2.15484105626593,
36.3345524375081));
#21821=CARTESIAN_POINT('Ctrl Pts',(-2.41037868396717,-2.13922738878082,
36.3332685845929));
#21822=CARTESIAN_POINT('Ctrl Pts',(-2.4170595355309,-2.13167596483264,36.3326487603306));
#21823=CARTESIAN_POINT('Ctrl Pts',(-2.43233722136632,-2.11424330367405,
36.3312203273868));
#21824=CARTESIAN_POINT('Ctrl Pts',(-2.44090943012627,-2.10434081159747,
36.330410705713));
#21825=CARTESIAN_POINT('Ctrl Pts',(-2.46366055643201,-2.077732978578,36.3282398591823));
#21826=CARTESIAN_POINT('Ctrl Pts',(-2.47772967263198,-2.06093505444706,
36.3268741521003));
#21827=CARTESIAN_POINT('Ctrl Pts',(-2.59564432521869,-1.91719733185216,
36.3152262642827));
#21828=CARTESIAN_POINT('Ctrl Pts',(-2.68981555077983,-1.78266448109943,
36.3045561258471));
#21829=CARTESIAN_POINT('Ctrl Pts',(-2.90296655650853,-1.42255880187577,
36.2766451192449));
#21830=CARTESIAN_POINT('Ctrl Pts',(-3.00619697526368,-1.1889757742665,36.2590762793693));
#21831=CARTESIAN_POINT('Ctrl Pts',(-3.09723001100283,-0.892406918471076,
36.2387879909886));
#21832=CARTESIAN_POINT('Ctrl Pts',(-3.11220098758202,-0.838707191176308,
36.2351947135659));
#21833=CARTESIAN_POINT('Ctrl Pts',(-3.12860596231211,-0.77335485671857,
36.2309399339579));
#21834=CARTESIAN_POINT('Ctrl Pts',(-3.1313783140909,-0.762051747337994,
36.23020828139));
#21835=CARTESIAN_POINT('Ctrl Pts',(-3.13560336091536,-0.744413435422304,
36.2290734147302));
#21836=CARTESIAN_POINT('Ctrl Pts',(-3.13709819101134,-0.738088572967554,
36.2286678385843));
#21837=CARTESIAN_POINT('Ctrl Pts',(-3.13984177468579,-0.72632112201274,
36.2279158659925));
#21838=CARTESIAN_POINT('Ctrl Pts',(-3.14109550405649,-0.720879863391161,
36.2275691944005));
#21839=CARTESIAN_POINT('Ctrl Pts',(-3.14390848360291,-0.708524692862517,
36.2267843606805));
#21840=CARTESIAN_POINT('Ctrl Pts',(-3.14545906890058,-0.7016088951856,36.2263467005048));
#21841=CARTESIAN_POINT('Ctrl Pts',(-3.15000053601545,-0.681035719783496,
36.2250494938298));
#21842=CARTESIAN_POINT('Ctrl Pts',(-3.15292541978737,-0.667363725563551,
36.2241936408038));
#21843=CARTESIAN_POINT('Ctrl Pts',(-3.17473630572985,-0.562066480390239,
36.217646818863));
#21844=CARTESIAN_POINT('Ctrl Pts',(-3.18971552183379,-0.469667736758124,
36.2121612808798));
#21845=CARTESIAN_POINT('Ctrl Pts',(-3.22881685393737,-0.137475661207952,
36.1929448764684));
#21846=CARTESIAN_POINT('Ctrl Pts',(-3.23006391976129,0.104198470726065,
36.1798418610527));
#21847=CARTESIAN_POINT('Ctrl Pts',(-3.19454133368619,0.435317819656115,
36.160884215462));
#21848=CARTESIAN_POINT('Ctrl Pts',(-3.18080107331359,0.526401492349101,
36.1555698766831));
#21849=CARTESIAN_POINT('Ctrl Pts',(-3.15243249578763,0.671893889730702,
36.1468294285881));
#21850=CARTESIAN_POINT('Ctrl Pts',(-3.14024503129078,0.726727324839323,
36.1434770969363));
#21851=CARTESIAN_POINT('Ctrl Pts',(-3.12246623469435,0.797883107871334,
36.1390389195492));
#21852=CARTESIAN_POINT('Ctrl Pts',(-3.11816761874797,0.814520425915876,
36.1379948815497));
#21853=CARTESIAN_POINT('Ctrl Pts',(-3.11093724354449,0.841608473586556,
36.1362843746005));
#21854=CARTESIAN_POINT('Ctrl Pts',(-3.10808534167546,0.852080313344894,
36.1356205071843));
#21855=CARTESIAN_POINT('Ctrl Pts',(-3.10248225175357,0.872251734680528,
36.1343366035991));
#21856=CARTESIAN_POINT('Ctrl Pts',(-3.09973833263651,0.881953216784308,
36.1337168111851));
#21857=CARTESIAN_POINT('Ctrl Pts',(-3.09332614644484,0.904224736958464,
36.1322886061585));
#21858=CARTESIAN_POINT('Ctrl Pts',(-3.08962672060242,0.916785548758172,
36.1314791816102));
#21859=CARTESIAN_POINT('Ctrl Pts',(-3.07953558225134,0.950293529925363,
36.129309207357));
#21860=CARTESIAN_POINT('Ctrl Pts',(-3.07300680849741,0.971198389648268,
36.1279441810858));
#21861=CARTESIAN_POINT('Ctrl Pts',(-3.0159472071808,1.14756308465134,36.1163308383265));
#21862=CARTESIAN_POINT('Ctrl Pts',(-2.95387687150754,1.29901325345948,36.105697220258));
#21863=CARTESIAN_POINT('Ctrl Pts',(-2.76697646274527,1.67157634412449,36.0778999850928));
#21864=CARTESIAN_POINT('Ctrl Pts',(-2.62704589908076,1.8838659841783,36.0604107198992));
#21865=CARTESIAN_POINT('Ctrl Pts',(-2.4268025361608,2.12132573757848,36.0400797143045));
#21866=CARTESIAN_POINT('Ctrl Pts',(-2.38874354333528,2.16409303804695,36.0363872694324));
#21867=CARTESIAN_POINT('Ctrl Pts',(-2.34153542950344,2.2143773270336,36.0320314379602));
#21868=CARTESIAN_POINT('Ctrl Pts',(-2.33346121713322,2.22288413378063,36.0312940349814));
#21869=CARTESIAN_POINT('Ctrl Pts',(-2.32082720425748,2.23605034476201,36.0301522142088));
#21870=CARTESIAN_POINT('Ctrl Pts',(-2.31629950050604,2.24074020851906,36.029745388234));
#21871=CARTESIAN_POINT('Ctrl Pts',(-2.30786846486906,2.24942034050592,36.0289922854517));
#21872=CARTESIAN_POINT('Ctrl Pts',(-2.30396903297706,2.2534141685973,36.0286457260504));
#21873=CARTESIAN_POINT('Ctrl Pts',(-2.29511360627042,2.26243694868658,36.0278626538892));
#21874=CARTESIAN_POINT('Ctrl Pts',(-2.290151462035,2.26745974510023,36.0274266337121));
#21875=CARTESIAN_POINT('Ctrl Pts',(-2.27540346167664,2.28229020923059,36.0261387796157));
#21876=CARTESIAN_POINT('Ctrl Pts',(-2.26557067601711,2.29205127353722,36.0252905607156));
#21877=CARTESIAN_POINT('Ctrl Pts',(-2.19153366999279,2.3646062912491,36.0189783980574));
#21878=CARTESIAN_POINT('Ctrl Pts',(-2.12478637581597,2.42476159288578,36.0137036131672));
#21879=CARTESIAN_POINT('Ctrl Pts',(-1.86643674046048,2.63872350758135,35.9943970810265));
#21880=CARTESIAN_POINT('Ctrl Pts',(-1.65997040785983,2.77325803802885,35.981053019721));
#21881=CARTESIAN_POINT('Ctrl Pts',(-1.35827624099663,2.92396860341079,35.961850542876));
#21882=CARTESIAN_POINT('Ctrl Pts',(-1.27463637834816,2.96138598143209,35.9565630524638));
#21883=CARTESIAN_POINT('Ctrl Pts',(-1.1375192048237,3.01584123027732,35.9478627399254));
#21884=CARTESIAN_POINT('Ctrl Pts',(-1.08499093539938,3.03513465362525,35.944522811462));
#21885=CARTESIAN_POINT('Ctrl Pts',(-1.0157326370007,3.05854528327568,35.9400987738295));
#21886=CARTESIAN_POINT('Ctrl Pts',(-0.999432527825012,3.06391035187438,
35.9390561348554));
#21887=CARTESIAN_POINT('Ctrl Pts',(-0.972759502201917,3.07245409982136,
35.9373473443108));
#21888=CARTESIAN_POINT('Ctrl Pts',(-0.962411873305188,3.07571107651609,
35.9366837842103));
#21889=CARTESIAN_POINT('Ctrl Pts',(-0.942414204529635,3.08189466328807,
35.9354000702273));
#21890=CARTESIAN_POINT('Ctrl Pts',(-0.932766472689344,3.08482835053112,
35.9347801579221));
#21891=CARTESIAN_POINT('Ctrl Pts',(-0.910548242818551,3.09147072288122,
35.9333510959763));
#21892=CARTESIAN_POINT('Ctrl Pts',(-0.897968636476481,3.09514808251229,
35.9325409304278));
#21893=CARTESIAN_POINT('Ctrl Pts',(-0.864270272341653,3.10477629925755,
35.9303676766413));
#21894=CARTESIAN_POINT('Ctrl Pts',(-0.84311287625281,3.11058830633781,35.9290000905431));
#21895=CARTESIAN_POINT('Ctrl Pts',(-0.661863218807286,3.15839317942911,
35.917255867631));
#21896=CARTESIAN_POINT('Ctrl Pts',(-0.498840065700016,3.18820543149673,
35.9064838119598));
#21897=CARTESIAN_POINT('Ctrl Pts',(-0.0775209154443138,3.23214251743292,
35.8782184628344));
#21898=CARTESIAN_POINT('Ctrl Pts',(0.181502930681532,3.22797267735349,35.8603879234517));
#21899=CARTESIAN_POINT('Ctrl Pts',(0.487863319199088,3.18601893455163,35.8402195684928));
#21900=CARTESIAN_POINT('Ctrl Pts',(0.538307763061424,3.17788494441735,35.8369327137392));
#21901=CARTESIAN_POINT('Ctrl Pts',(0.599688383849988,3.16648384856296,35.8329920686422));
#21902=CARTESIAN_POINT('Ctrl Pts',(0.610825264923671,3.1643543773893,35.8322794622434));
#21903=CARTESIAN_POINT('Ctrl Pts',(0.628263365765897,3.16092456329657,35.8311676523732));
#21904=CARTESIAN_POINT('Ctrl Pts',(0.634572195913244,3.15966407732031,35.8307662369272));
#21905=CARTESIAN_POINT('Ctrl Pts',(0.646357797563831,3.15727262567872,35.8300179358789));
#21906=CARTESIAN_POINT('Ctrl Pts',(0.651835339067373,3.15614630945402,35.8296708001458));
#21907=CARTESIAN_POINT('Ctrl Pts',(0.664341425809498,3.15354080655823,35.8288796893868));
#21908=CARTESIAN_POINT('Ctrl Pts',(0.671367963211146,3.15205238043466,35.8284362492664));
#21909=CARTESIAN_POINT('Ctrl Pts',(0.692987271204733,3.14739720691011,35.8270749245637));
#21910=CARTESIAN_POINT('Ctrl Pts',(0.707563300445875,3.1441524663894,35.8261613932797));
#21911=CARTESIAN_POINT('Ctrl Pts',(0.850396354165353,3.11131309319946,35.8172470247137));
#21912=CARTESIAN_POINT('Ctrl Pts',(0.976765664063272,3.07398449267316,35.8096553219812));
#21913=CARTESIAN_POINT('Ctrl Pts',(1.28116377243312,2.96339000666203,35.7913234671513));
#21914=CARTESIAN_POINT('Ctrl Pts',(1.45558247647445,2.88172568056682,35.780760304734));
#21915=CARTESIAN_POINT('Ctrl Pts',(1.70654800596999,2.73559036088559,35.7642735856097));
#21916=CARTESIAN_POINT('Ctrl Pts',(1.78910043840985,2.68232698899493,35.7586216402397));
#21917=CARTESIAN_POINT('Ctrl Pts',(1.91698293481149,2.59128356765466,35.7493783783071));
#21918=CARTESIAN_POINT('Ctrl Pts',(1.9639329974732,2.55588353055802,35.745872467841));
#21919=CARTESIAN_POINT('Ctrl Pts',(2.02353954300244,2.508328195338,35.7412594877645));
#21920=CARTESIAN_POINT('Ctrl Pts',(2.03710357511151,2.49732489340492,35.7401985238074));
#21921=CARTESIAN_POINT('Ctrl Pts',(2.05899814435663,2.47926669655605,35.7384672422277));
#21922=CARTESIAN_POINT('Ctrl Pts',(2.06738357303326,2.47227867936313,35.7377996490559));
#21923=CARTESIAN_POINT('Ctrl Pts',(2.0834294887869,2.45876805592077,35.7365133556708));
#21924=CARTESIAN_POINT('Ctrl Pts',(2.09109526081211,2.45225190266198,35.7358949252326));
#21925=CARTESIAN_POINT('Ctrl Pts',(2.10856282331383,2.43726245061999,35.7344766745273));
#21926=CARTESIAN_POINT('Ctrl Pts',(2.11834423121709,2.42876576541529,35.7336758885155));
#21927=CARTESIAN_POINT('Ctrl Pts',(2.14416746548818,2.40605957695487,35.7315440229543));
#21928=CARTESIAN_POINT('Ctrl Pts',(2.16011903659429,2.39174884129328,35.7302087106815));
#21929=CARTESIAN_POINT('Ctrl Pts',(2.28178596952608,2.28038701143607,35.7198793175012));
#21930=CARTESIAN_POINT('Ctrl Pts',(2.38104065298987,2.17654485412815,35.7105913832565));
#21931=CARTESIAN_POINT('Ctrl Pts',(2.60610116272965,1.9072020843764,35.6873192778303));
#21932=CARTESIAN_POINT('Ctrl Pts',(2.72346917200883,1.73547943336091,35.6731209344519));
#21933=CARTESIAN_POINT('Ctrl Pts',(2.86327716762166,1.48140730809603,35.6536685706928));
#21934=CARTESIAN_POINT('Ctrl Pts',(2.90026300488421,1.40762216183968,35.6481915085174));
#21935=CARTESIAN_POINT('Ctrl Pts',(2.95217899339544,1.29329433477463,35.6400426875703));
#21936=CARTESIAN_POINT('Ctrl Pts',(2.96919330260592,1.25373944989675,35.6372828773444));
#21937=CARTESIAN_POINT('Ctrl Pts',(2.9894558456152,1.20390474923328,35.6338900495056));
#21938=CARTESIAN_POINT('Ctrl Pts',(2.99345118547411,1.19393588856406,35.6332155142094));
#21939=CARTESIAN_POINT('Ctrl Pts',(2.99971151516166,1.17808662315959,35.6321498891079));
#21940=CARTESIAN_POINT('Ctrl Pts',(3.00200917756625,1.17221933326814,35.6317568749454));
#21941=CARTESIAN_POINT('Ctrl Pts',(3.00632254169706,1.16110890536614,35.6310154895963));
#21942=CARTESIAN_POINT('Ctrl Pts',(3.00834171820475,1.15586730284646,35.6306669200337));
#21943=CARTESIAN_POINT('Ctrl Pts',(3.01294585228916,1.14382158984963,35.6298685788811));
#21944=CARTESIAN_POINT('Ctrl Pts',(3.01552146961116,1.13701398715773,35.629419370794));
#21945=CARTESIAN_POINT('Ctrl Pts',(3.02233856552016,1.11880964888251,35.6282232474624));
#21946=CARTESIAN_POINT('Ctrl Pts',(3.02653868850251,1.10739740513477,35.6274787377006));
#21947=CARTESIAN_POINT('Ctrl Pts',(3.0568196732153,1.0236610669434,35.6220530591413));
#21948=CARTESIAN_POINT('Ctrl Pts',(3.08037192600609,0.95044167935542,35.6175107525742));
#21949=CARTESIAN_POINT('Ctrl Pts',(3.11097997869764,0.842135496686508,35.6109890728551));
#21950=CARTESIAN_POINT('Ctrl Pts',(3.12010599606352,0.807667834496542,35.6089422944302));
#21951=CARTESIAN_POINT('Ctrl Pts',(3.19099536871426,0.520768915049164,35.5920907939819));
#21952=CARTESIAN_POINT('Ctrl Pts',(3.22258956834844,0.26187146746877,35.5779830578411));
#21953=CARTESIAN_POINT('Ctrl Pts',(3.22277045874783,-0.0322773699741125,
35.5610272103996));
#21954=CARTESIAN_POINT('Ctrl Pts',(3.22224523984713,-0.066533945178146,
35.5590399266099));
#21955=CARTESIAN_POINT('Ctrl Pts',(3.21890748730524,-0.173222058847471,
35.5528027301262));
#21956=CARTESIAN_POINT('Ctrl Pts',(3.21419767276895,-0.245567538508346,
35.5485036776561));
#21957=CARTESIAN_POINT('Ctrl Pts',(3.20514311002084,-0.33697288876932,35.5429577596319));
#21958=CARTESIAN_POINT('Ctrl Pts',(3.20305899040129,-0.356238911551028,
35.541782396898));
#21959=CARTESIAN_POINT('Ctrl Pts',(3.19946716450695,-0.386857263082903,
35.5399037846077));
#21960=CARTESIAN_POINT('Ctrl Pts',(3.1980724597936,-0.398222570088934,35.5392041122974));
#21961=CARTESIAN_POINT('Ctrl Pts',(3.19535127629391,-0.419460375111782,
35.537892182604));
#21962=CARTESIAN_POINT('Ctrl Pts',(3.19403953329945,-0.429334649629104,
35.5372803993823));
#21963=CARTESIAN_POINT('Ctrl Pts',(3.19101107114512,-0.451349357235508,
35.5359123039807));
#21964=CARTESIAN_POINT('Ctrl Pts',(3.18927080993015,-0.463486345758742,
35.5351552527041));
#21965=CARTESIAN_POINT('Ctrl Pts',(3.18396657084568,-0.499034276468238,
35.5329295583531));
#21966=CARTESIAN_POINT('Ctrl Pts',(3.18021382781233,-0.52241582519382,35.5314549444777));
#21967=CARTESIAN_POINT('Ctrl Pts',(3.14448045485697,-0.730378754707215,
35.5182414144364));
#21968=CARTESIAN_POINT('Ctrl Pts',(3.09672586591152,-0.911854036969413,
35.505990195684));
#21969=CARTESIAN_POINT('Ctrl Pts',(2.9656460481618,-1.27727914256669,35.4799597309547));
#21970=CARTESIAN_POINT('Ctrl Pts',(2.88025696302375,-1.45966344587103,35.466189726902));
#21971=CARTESIAN_POINT('Ctrl Pts',(2.73622269328183,-1.70474207114958,35.4473403881831));
#21972=CARTESIAN_POINT('Ctrl Pts',(2.69123067814493,-1.77491978094744,35.4419040066358));
#21973=CARTESIAN_POINT('Ctrl Pts',(2.63578119894601,-1.85444337392499,35.4357656432674));
#21974=CARTESIAN_POINT('Ctrl Pts',(2.62792686323624,-1.86555706765961,35.4349083201578));
#21975=CARTESIAN_POINT('Ctrl Pts',(2.61592162305662,-1.88231791459035,35.4336165957597));
#21976=CARTESIAN_POINT('Ctrl Pts',(2.6118224261631,-1.88800166471346,35.4331787764034));
#21977=CARTESIAN_POINT('Ctrl Pts',(2.6044269530751,-1.89818569295259,35.4323947565128));
#21978=CARTESIAN_POINT('Ctrl Pts',(2.60113751873638,-1.90269080224331,35.4320480952229));
#21979=CARTESIAN_POINT('Ctrl Pts',(2.59395485720042,-1.91247451749451,35.4312956204062));
#21980=CARTESIAN_POINT('Ctrl Pts',(2.5900572199996,-1.91774976996398,35.4308901207858));
#21981=CARTESIAN_POINT('Ctrl Pts',(2.579034956004,-1.93257294270851,35.4297512096261));
#21982=CARTESIAN_POINT('Ctrl Pts',(2.57187336579427,-1.94209342818767,35.4290203320154));
#21983=CARTESIAN_POINT('Ctrl Pts',(2.52804589648987,-1.99968924852045,35.4246010107285));
#21984=CARTESIAN_POINT('Ctrl Pts',(2.49008323391232,-2.04676811675291,35.4209981831955));
#21985=CARTESIAN_POINT('Ctrl Pts',(2.28489354975244,-2.28706488110814,35.40249454867));
#21986=CARTESIAN_POINT('Ctrl Pts',(2.09643850884567,-2.46097052873984,35.3886395806164));
#21987=CARTESIAN_POINT('Ctrl Pts',(1.76143196867848,-2.70341046135735,35.3652458027176));
#21988=CARTESIAN_POINT('Ctrl Pts',(1.62684207387483,-2.78647554838319,35.356126270503));
#21989=CARTESIAN_POINT('Ctrl Pts',(1.467387265963,-2.86938439405468,35.3453154817556));
#21990=CARTESIAN_POINT('Ctrl Pts',(1.44795700712991,-2.87923820809416,35.3439983244115));
#21991=CARTESIAN_POINT('Ctrl Pts',(1.41672087715647,-2.89468307490204,35.3418804623409));
#21992=CARTESIAN_POINT('Ctrl Pts',(1.40497811468858,-2.90040077183462,35.3410841959532));
#21993=CARTESIAN_POINT('Ctrl Pts',(1.38411443619748,-2.91040312218429,35.339669150958));
#21994=CARTESIAN_POINT('Ctrl Pts',(1.37500751912376,-2.91471669717657,35.3390513897142));
#21995=CARTESIAN_POINT('Ctrl Pts',(1.3560369876221,-2.92359357021239,35.3377642617047));
#21996=CARTESIAN_POINT('Ctrl Pts',(1.34617023405761,-2.92814982060188,35.3370946603137));
#21997=CARTESIAN_POINT('Ctrl Pts',(1.32058308736153,-2.93980874357326,35.3353577093626));
#21998=CARTESIAN_POINT('Ctrl Pts',(1.30482853168874,-2.94683518773189,35.3342877496162));
#21999=CARTESIAN_POINT('Ctrl Pts',(1.23698173352815,-2.9764437312877,35.3296773755474));
#22000=CARTESIAN_POINT('Ctrl Pts',(1.18435676770846,-2.99777241964207,35.3260945593449));
#22001=CARTESIAN_POINT('Ctrl Pts',(1.04366031753545,-3.05051313782734,35.3164915764213));
#22002=CARTESIAN_POINT('Ctrl Pts',(0.954743117662606,-3.07949999194473,
35.3103969897814));
#22003=CARTESIAN_POINT('Ctrl Pts',(0.656845778650454,-3.16247139270354,
35.2899247795844));
#22004=CARTESIAN_POINT('Ctrl Pts',(0.443710345811826,-3.199340739048,35.2751505480742));
#22005=CARTESIAN_POINT('Ctrl Pts',(0.113232386153195,-3.22283315364041,
35.2529448366808));
#22006=CARTESIAN_POINT('Ctrl Pts',(-0.00242276030634944,-3.22482174519131,
35.2453152469946));
#22007=CARTESIAN_POINT('Ctrl Pts',(-0.132683918455096,-3.2200512461733,
35.2370526009332));
#22008=CARTESIAN_POINT('Ctrl Pts',(-0.147417957322412,-3.21941035215556,
35.2361228164553));
#22009=CARTESIAN_POINT('Ctrl Pts',(-0.169284399981222,-3.21830878263779,
35.2347506128558));
#22010=CARTESIAN_POINT('Ctrl Pts',(-0.176420262156259,-3.21792549974631,
35.2343040230992));
#22011=CARTESIAN_POINT('Ctrl Pts',(-0.189134577961852,-3.21720016603975,
35.2335105456669));
#22012=CARTESIAN_POINT('Ctrl Pts',(-0.194713460213433,-3.21686733749034,
35.2331631481637));
#22013=CARTESIAN_POINT('Ctrl Pts',(-0.206736929684483,-3.21611864022215,
35.2324161189759));
#22014=CARTESIAN_POINT('Ctrl Pts',(-0.213181122619191,-3.2156979144143,
35.2320167632884));
#22015=CARTESIAN_POINT('Ctrl Pts',(-0.23104695915257,-3.21447755572762,
35.2309123357424));
#22016=CARTESIAN_POINT('Ctrl Pts',(-0.242465805131233,-3.21363641318313,
35.2302095577113));
#22017=CARTESIAN_POINT('Ctrl Pts',(-0.30647150506476,-3.20857848651103,
35.2262865344371));
#22018=CARTESIAN_POINT('Ctrl Pts',(-0.358956472586155,-3.20313154328421,
35.2231311068008));
#22019=CARTESIAN_POINT('Ctrl Pts',(-0.665949292365562,-3.16363011399075,
35.2049125407654));
#22020=CARTESIAN_POINT('Ctrl Pts',(-0.915807722760667,-3.10054341059219,
35.1909852445635));
#22021=CARTESIAN_POINT('Ctrl Pts',(-1.2646773558253,-2.96654253713258,35.1698817324028));
#22022=CARTESIAN_POINT('Ctrl Pts',(-1.37140074843424,-2.91873648247267,
35.1631909462925));
#22023=CARTESIAN_POINT('Ctrl Pts',(-1.4752555264658,-2.86526415782771,35.1563175586878));
#22024=CARTESIAN_POINT('',(3.22274857165764,-0.00244669484556194,35.3125278845694));
#22025=CARTESIAN_POINT('Ctrl Pts',(-1.47525540445791,-2.86526422064663,
34.9063554765866));
#22026=CARTESIAN_POINT('Ctrl Pts',(-1.45292930620259,-2.87675938987894,
34.9077663722593));
#22027=CARTESIAN_POINT('Ctrl Pts',(-1.43046239099383,-2.88799693977385,
34.9091808614218));
#22028=CARTESIAN_POINT('Ctrl Pts',(-1.26043613777036,-2.97056855777938,
34.9198572862357));
#22029=CARTESIAN_POINT('Ctrl Pts',(-1.10778616152534,-3.03080454484676,
34.9293011572805));
#22030=CARTESIAN_POINT('Ctrl Pts',(-0.930291869104101,-3.08563686439293,
34.9404746320225));
#22031=CARTESIAN_POINT('Ctrl Pts',(-0.909288411363604,-3.09189139027313,
34.9417994740626));
#22032=CARTESIAN_POINT('Ctrl Pts',(-0.875634271945152,-3.10154053545866,
34.9439272088911));
#22033=CARTESIAN_POINT('Ctrl Pts',(-0.863023620240147,-3.10507315441357,
34.9447255949124));
#22034=CARTESIAN_POINT('Ctrl Pts',(-0.840669612786261,-3.11118848065654,
34.9461429166753));
#22035=CARTESIAN_POINT('Ctrl Pts',(-0.830934958741308,-3.11380253881126,
34.9467608223501));
#22036=CARTESIAN_POINT('Ctrl Pts',(-0.810699682232674,-3.11913469368569,
34.9480467632726));
#22037=CARTESIAN_POINT('Ctrl Pts',(-0.800197293731507,-3.12184552766872,
34.9487150255927));
#22038=CARTESIAN_POINT('Ctrl Pts',(-0.773040014159932,-3.12870921128487,
34.9504452971621));
#22039=CARTESIAN_POINT('Ctrl Pts',(-0.756365435618884,-3.13278207057212,
34.9515098804302));
#22040=CARTESIAN_POINT('Ctrl Pts',(-0.685127757610212,-3.14958037949171,
34.9560679076935));
#22041=CARTESIAN_POINT('Ctrl Pts',(-0.630273073406979,-3.16101436698318,
34.9596025745661));
#22042=CARTESIAN_POINT('Ctrl Pts',(-0.484851301103759,-3.18739063269344,
34.9690444199729));
#22043=CARTESIAN_POINT('Ctrl Pts',(-0.39390078102764,-3.19990304455322,
34.9750229661058));
#22044=CARTESIAN_POINT('Ctrl Pts',(-0.0691548172338245,-3.23052492976057,
34.9965997093589));
#22045=CARTESIAN_POINT('Ctrl Pts',(0.165917127999895,-3.22700031323257,
35.0126988713293));
#22046=CARTESIAN_POINT('Ctrl Pts',(0.418350219005723,-3.19554380295184,
35.0296712679666));
#22047=CARTESIAN_POINT('Ctrl Pts',(0.438162186753174,-3.19288756849992,
35.0310006946464));
#22048=CARTESIAN_POINT('Ctrl Pts',(0.538410711821889,-3.17849635255725,
35.0377104753343));
#22049=CARTESIAN_POINT('Ctrl Pts',(0.618415001021133,-3.16390431477802,
35.0430099104089));
#22050=CARTESIAN_POINT('Ctrl Pts',(0.710989412689877,-3.14337310041445,
35.0490132261124));
#22051=CARTESIAN_POINT('Ctrl Pts',(0.724171874476634,-3.14036232060865,
35.0498649965779));
#22052=CARTESIAN_POINT('Ctrl Pts',(0.744137358248051,-3.1356699409744,35.0511499399372));
#22053=CARTESIAN_POINT('Ctrl Pts',(0.750934309816619,-3.13404914626411,
35.0515864797157));
#22054=CARTESIAN_POINT('Ctrl Pts',(0.763144882370624,-3.13109542068199,
35.0523690271339));
#22055=CARTESIAN_POINT('Ctrl Pts',(0.768560335508649,-3.12977054383343,
35.0527154888963));
#22056=CARTESIAN_POINT('Ctrl Pts',(0.780350562240213,-3.12685364745952,
35.0534684685532));
#22057=CARTESIAN_POINT('Ctrl Pts',(0.786723894018734,-3.12525618934163,
35.0538746676402));
#22058=CARTESIAN_POINT('Ctrl Pts',(0.80469689099108,-3.12069284333201,35.0550179272153));
#22059=CARTESIAN_POINT('Ctrl Pts',(0.816285121816515,-3.11768175398948,
35.0557524216429));
#22060=CARTESIAN_POINT('Ctrl Pts',(0.887394488285968,-3.09878101651963,
35.060244858625));
#22061=CARTESIAN_POINT('Ctrl Pts',(0.946471035216613,-3.0812508002563,35.063913850737));
#22062=CARTESIAN_POINT('Ctrl Pts',(1.25864133498492,-2.97879114230051,35.0831396542036));
#22063=CARTESIAN_POINT('Ctrl Pts',(1.50096483369849,-2.86435117756486,35.0975670168958));
#22064=CARTESIAN_POINT('Ctrl Pts',(1.84950045737443,-2.64323899408243,35.120997180681));
#22065=CARTESIAN_POINT('Ctrl Pts',(1.96713019752114,-2.55690344213947,35.1294438775362));
#22066=CARTESIAN_POINT('Ctrl Pts',(2.09496623624399,-2.44901979951021,35.1395081131937));
#22067=CARTESIAN_POINT('Ctrl Pts',(2.11128724137151,-2.43496358479719,35.1408105703398));
#22068=CARTESIAN_POINT('Ctrl Pts',(2.13722039559061,-2.41217229639306,35.1429091243416));
#22069=CARTESIAN_POINT('Ctrl Pts',(2.14692294891978,-2.40354073201732,35.1437009098924));
#22070=CARTESIAN_POINT('Ctrl Pts',(2.16405060814628,-2.38811720508672,35.1451106139376));
#22071=CARTESIAN_POINT('Ctrl Pts',(2.1714966111556,-2.38134862713143,35.1457275392704));
#22072=CARTESIAN_POINT('Ctrl Pts',(2.18577929560792,-2.36824266797561,35.14691885616));
#22073=CARTESIAN_POINT('Ctrl Pts',(2.19262042788094,-2.36191026921959,35.1474930313998));
#22074=CARTESIAN_POINT('Ctrl Pts',(2.21046113508075,-2.34525195816643,35.1489998132359));
#22075=CARTESIAN_POINT('Ctrl Pts',(2.22141574557196,-2.33487842292567,35.1499344685525));
#22076=CARTESIAN_POINT('Ctrl Pts',(2.26262368632985,-2.29530380858307,35.1534867380244));
#22077=CARTESIAN_POINT('Ctrl Pts',(2.29237629209639,-2.2655895888391,35.1561267090831));
#22078=CARTESIAN_POINT('Ctrl Pts',(2.36498724047232,-2.19017740471364,35.1627633713943));
#22079=CARTESIAN_POINT('Ctrl Pts',(2.40710902354072,-2.14379733402282,35.1667898613596));
#22080=CARTESIAN_POINT('Ctrl Pts',(2.52683000432368,-2.00399387390788,35.1787689156205));
#22081=CARTESIAN_POINT('Ctrl Pts',(2.60052735404878,-1.9073841069181,35.1868540777386));
#22082=CARTESIAN_POINT('Ctrl Pts',(2.80829628852151,-1.60052450429051,35.2118120830906));
#22083=CARTESIAN_POINT('Ctrl Pts',(2.92360460029175,-1.37867950457497,35.2289539029287));
#22084=CARTESIAN_POINT('Ctrl Pts',(3.01975798738673,-1.12589116364772,35.2462198111673));
#22085=CARTESIAN_POINT('Ctrl Pts',(3.02711712655888,-1.1059526089785,35.2475666645863));
#22086=CARTESIAN_POINT('Ctrl Pts',(3.03715400392429,-1.07790812734312,35.2494387003354));
#22087=CARTESIAN_POINT('Ctrl Pts',(3.03999741382545,-1.06986265586188,35.2499731902159));
#22088=CARTESIAN_POINT('Ctrl Pts',(3.04453383113319,-1.05686267995059,35.250832584171));
#22089=CARTESIAN_POINT('Ctrl Pts',(3.04624675537791,-1.05191524348307,35.2511586578931));
#22090=CARTESIAN_POINT('Ctrl Pts',(3.0498223232361,-1.04150595757504,35.2518426002686));
#22091=CARTESIAN_POINT('Ctrl Pts',(3.05168236362497,-1.03604324970668,35.2522003070227));
#22092=CARTESIAN_POINT('Ctrl Pts',(3.05618729722679,-1.02269542692598,35.2530714324032));
#22093=CARTESIAN_POINT('Ctrl Pts',(3.05881638239471,-1.01480494401201,35.2535839185662));
#22094=CARTESIAN_POINT('Ctrl Pts',(3.06812182888641,-0.98651245021176,35.2554129612008));
#22095=CARTESIAN_POINT('Ctrl Pts',(3.07462502953678,-0.966053495529832,
35.2567196951894));
#22096=CARTESIAN_POINT('Ctrl Pts',(3.11354420921741,-0.839238949451706,
35.264730398011));
#22097=CARTESIAN_POINT('Ctrl Pts',(3.14064605225898,-0.73131878439612,35.2711631847051));
#22098=CARTESIAN_POINT('Ctrl Pts',(3.20228605224234,-0.418056310754366,
35.2892997880465));
#22099=CARTESIAN_POINT('Ctrl Pts',(3.22259086965953,-0.210506202816104,
35.3006989395904));
#22100=CARTESIAN_POINT('Ctrl Pts',(3.2227490683711,-0.00245047203661506,
35.3125268034609));
#22101=CARTESIAN_POINT('Ctrl Pts',(3.22274907127793,-0.00244664611808667,
35.3125270209625));
#22102=CARTESIAN_POINT('Ctrl Pts',(3.222822198994,0.0938779826516697,35.3180030298239));
#22103=CARTESIAN_POINT('Ctrl Pts',(3.2185767818221,0.190152796939803,35.3235561489518));
#22104=CARTESIAN_POINT('Ctrl Pts',(3.20588205807585,0.332591966317148,35.3319873302714));
#22105=CARTESIAN_POINT('Ctrl Pts',(3.20072779093437,0.378996656346596,35.3347679097327));
#22106=CARTESIAN_POINT('Ctrl Pts',(3.19245693920111,0.441125918843006,35.3385432245935));
#22107=CARTESIAN_POINT('Ctrl Pts',(3.19022835540884,0.456964343398726,35.3395102459607));
#22108=CARTESIAN_POINT('Ctrl Pts',(3.18626032428469,0.483719859681448,35.3411518760625));
#22109=CARTESIAN_POINT('Ctrl Pts',(3.18458242116393,0.494645888305743,35.3418245401713));
#22110=CARTESIAN_POINT('Ctrl Pts',(3.18138073222578,0.514802606888697,35.343069798848));
#22111=CARTESIAN_POINT('Ctrl Pts',(3.17987289518586,0.524035738267946,35.3436418822315));
#22112=CARTESIAN_POINT('Ctrl Pts',(3.17667380192803,0.543102830753287,35.3448267903223));
#22113=CARTESIAN_POINT('Ctrl Pts',(3.17497703570969,0.552935753749137,35.3454397847159));
#22114=CARTESIAN_POINT('Ctrl Pts',(3.17104917621089,0.575083752271063,35.3468249504617));
#22115=CARTESIAN_POINT('Ctrl Pts',(3.16879196380773,0.587393976037243,35.347597947873));
#22116=CARTESIAN_POINT('Ctrl Pts',(3.16283206722838,0.61886319151895,35.3495820765352));
#22117=CARTESIAN_POINT('Ctrl Pts',(3.15902701529105,0.63800205714112,35.3507964632919));
#22118=CARTESIAN_POINT('Ctrl Pts',(3.13493297705785,0.753688096794359,35.3581845259994));
#22119=CARTESIAN_POINT('Ctrl Pts',(3.11039519341025,0.849287276382102,35.3644936335693));
#22120=CARTESIAN_POINT('Ctrl Pts',(3.06261102411507,1.00533551957057,35.3751383797574));
#22121=CARTESIAN_POINT('Ctrl Pts',(3.0418578526508,1.06648292520211,35.379399773773));
#22122=CARTESIAN_POINT('Ctrl Pts',(2.94398912463826,1.32868619866432,35.3980416007017));
#22123=CARTESIAN_POINT('Ctrl Pts',(2.84867416605034,1.52234281914099,35.4128122584179));
#22124=CARTESIAN_POINT('Ctrl Pts',(2.68796576556024,1.78010743066332,35.4330477547681));
#22125=CARTESIAN_POINT('Ctrl Pts',(2.63809033463233,1.85322009616731,35.4388531537061));
#22126=CARTESIAN_POINT('Ctrl Pts',(2.5738869008461,1.93948110285755,35.4457007292539));
#22127=CARTESIAN_POINT('Ctrl Pts',(2.5623729990046,1.9546675885902,35.4469061530209));
#22128=CARTESIAN_POINT('Ctrl Pts',(2.54587837315102,1.97602726308972,35.4486003580822));
#22129=CARTESIAN_POINT('Ctrl Pts',(2.54100879890514,1.98228522730869,35.449096577208));
#22130=CARTESIAN_POINT('Ctrl Pts',(2.53260068933571,1.99300872320809,35.4499465348641));
#22131=CARTESIAN_POINT('Ctrl Pts',(2.5290733341092,1.99748293987475,35.4503010600482));
#22132=CARTESIAN_POINT('Ctrl Pts',(2.52222693279569,2.00611993793479,35.4509851924609));
#22133=CARTESIAN_POINT('Ctrl Pts',(2.51890943473924,2.01028385221078,35.4513149097283));
#22134=CARTESIAN_POINT('Ctrl Pts',(2.50996017443316,2.02145946404088,35.4521996216935));
#22135=CARTESIAN_POINT('Ctrl Pts',(2.50430930530922,2.02845590286812,35.4527532546306));
#22136=CARTESIAN_POINT('Ctrl Pts',(2.4833899848165,2.05413581198401,35.454784834301));
#22137=CARTESIAN_POINT('Ctrl Pts',(2.46794069348604,2.07267184186707,35.4562502916358));
#22138=CARTESIAN_POINT('Ctrl Pts',(2.32053141693219,2.24554782791318,35.469927795437));
#22139=CARTESIAN_POINT('Ctrl Pts',(2.17445047837928,2.38728703534737,35.4812353044151));
#22140=CARTESIAN_POINT('Ctrl Pts',(1.88435771502452,2.61988086240072,35.5020094141611));
#22141=CARTESIAN_POINT('Ctrl Pts',(1.74465664835936,2.71491207884529,35.5114319292465));
#22142=CARTESIAN_POINT('Ctrl Pts',(1.5464281871252,2.82811377439754,35.5246682146053));
#22143=CARTESIAN_POINT('Ctrl Pts',(1.4938808924124,2.85621898990891,35.5281632300493));
#22144=CARTESIAN_POINT('Ctrl Pts',(1.41606868102879,2.89510246998893,35.5333379420563));
#22145=CARTESIAN_POINT('Ctrl Pts',(1.3913956644315,2.90704091091488,35.5349786056314));
#22146=CARTESIAN_POINT('Ctrl Pts',(1.34675667191248,2.92794174274711,35.5379484416452));
#22147=CARTESIAN_POINT('Ctrl Pts',(1.32684582374589,2.93701830193329,35.5392736405939));
#22148=CARTESIAN_POINT('Ctrl Pts',(1.29603469935726,2.95068660944577,35.541325790494));
#22149=CARTESIAN_POINT('Ctrl Pts',(1.28519874229726,2.9554224056854,35.5420477859514));
#22150=CARTESIAN_POINT('Ctrl Pts',(1.26608673208441,2.96365022108519,35.5433217974865));
#22151=CARTESIAN_POINT('Ctrl Pts',(1.25782164012358,2.96716749866542,35.5438729422159));
#22152=CARTESIAN_POINT('Ctrl Pts',(1.23917063255296,2.97501265594226,35.5451171384687));
#22153=CARTESIAN_POINT('Ctrl Pts',(1.22877657943962,2.97932077364512,35.5458108548017));
#22154=CARTESIAN_POINT('Ctrl Pts',(1.20077530730874,2.9907552592962,35.5476807175804));
#22155=CARTESIAN_POINT('Ctrl Pts',(1.18312750074961,2.99778045421981,35.5488602712433));
#22156=CARTESIAN_POINT('Ctrl Pts',(1.10360230784894,3.02862604087624,35.5541811551656));
#22157=CARTESIAN_POINT('Ctrl Pts',(1.0410645080087,3.05068801941584,35.5583808882861));
#22158=CARTESIAN_POINT('Ctrl Pts',(0.670324953753376,3.16874962926328,35.5833851699237));
#22159=CARTESIAN_POINT('Ctrl Pts',(0.349804969398493,3.21991791190272,35.6056886694998));
#22160=CARTESIAN_POINT('Ctrl Pts',(-0.0350210707554559,3.22315930273634,
35.6312791652481));
#22161=CARTESIAN_POINT('Ctrl Pts',(-0.0971925808733141,3.22188406580124,
35.6353675708624));
#22162=CARTESIAN_POINT('Ctrl Pts',(-0.182893561452371,3.21764291224097,
35.6409071917649));
#22163=CARTESIAN_POINT('Ctrl Pts',(-0.206482432798357,3.21621532886052,
35.6424218546974));
#22164=CARTESIAN_POINT('Ctrl Pts',(-0.247231118304599,3.21329906704435,
35.6450184917643));
#22165=CARTESIAN_POINT('Ctrl Pts',(-0.264398353381229,3.21193207610899,
35.646106333131));
#22166=CARTESIAN_POINT('Ctrl Pts',(-0.289135386438601,3.20976264022414,
35.6476642406725));
#22167=CARTESIAN_POINT('Ctrl Pts',(-0.296714242463301,3.20907091529585,
35.6481402449312));
#22168=CARTESIAN_POINT('Ctrl Pts',(-0.309910016238329,3.20781938479212,
35.6489666766877));
#22169=CARTESIAN_POINT('Ctrl Pts',(-0.31552801204594,3.2072716597146,35.6493177779765));
#22170=CARTESIAN_POINT('Ctrl Pts',(-0.327307768498945,3.20609194379902,
35.6500523711005));
#22171=CARTESIAN_POINT('Ctrl Pts',(-0.333469149909224,3.20545694948554,
35.6504356918027));
#22172=CARTESIAN_POINT('Ctrl Pts',(-0.349836035200082,3.20372247086048,
35.6514516121746));
#22173=CARTESIAN_POINT('Ctrl Pts',(-0.360038282121318,3.20259197586956,
35.6520824847972));
#22174=CARTESIAN_POINT('Ctrl Pts',(-0.40367289845304,3.19754574518788,35.6547711014066));
#22175=CARTESIAN_POINT('Ctrl Pts',(-0.437049586291402,3.19315493961492,
35.6568035218393));
#22176=CARTESIAN_POINT('Ctrl Pts',(-0.476615547774752,3.18731787825588,
35.6591906079939));
#22177=CARTESIAN_POINT('Ctrl Pts',(-0.482875551191465,3.1863755021517,35.6595676223802));
#22178=CARTESIAN_POINT('Ctrl Pts',(-0.78807014476277,3.13951168803674,35.6779176620613));
#22179=CARTESIAN_POINT('Ctrl Pts',(-1.07909311969837,3.05175323564138,35.6941078273691));
#22180=CARTESIAN_POINT('Ctrl Pts',(-1.43660826328232,2.88628354462794,35.7165410559189));
#22181=CARTESIAN_POINT('Ctrl Pts',(-1.51789998880267,2.84437228964257,35.7218192810321));
#22182=CARTESIAN_POINT('Ctrl Pts',(-1.64582570326363,2.77137102702872,35.7305055138283));
#22183=CARTESIAN_POINT('Ctrl Pts',(-1.69362443773071,2.74242143171488,35.7338409247734));
#22184=CARTESIAN_POINT('Ctrl Pts',(-1.7550761634918,2.70298340343429,35.7382595874149));
#22185=CARTESIAN_POINT('Ctrl Pts',(-1.76943349387717,2.69360663645655,35.7393014896748));
#22186=CARTESIAN_POINT('Ctrl Pts',(-1.79274581969509,2.67811455287119,35.7410092249677));
#22187=CARTESIAN_POINT('Ctrl Pts',(-1.80174611087036,2.67206775358597,35.7416724710425));
#22188=CARTESIAN_POINT('Ctrl Pts',(-1.81905491081398,2.66031171451251,35.7429556837871));
#22189=CARTESIAN_POINT('Ctrl Pts',(-1.82736749378812,2.65460867660189,35.7435754096296));
#22190=CARTESIAN_POINT('Ctrl Pts',(-1.8464241598826,2.64140249025563,35.745004193069));
#22191=CARTESIAN_POINT('Ctrl Pts',(-1.85714945377346,2.63387266053652,35.7458142669076));
#22192=CARTESIAN_POINT('Ctrl Pts',(-1.88571089358673,2.6135595504263,35.7479876068367));
#22193=CARTESIAN_POINT('Ctrl Pts',(-1.90346265497794,2.60065933571649,35.7493553731951));
#22194=CARTESIAN_POINT('Ctrl Pts',(-2.05259145839286,2.48994252587534,35.7609923150584));
#22195=CARTESIAN_POINT('Ctrl Pts',(-2.17644666712245,2.38243797731905,35.7716483608506));
#22196=CARTESIAN_POINT('Ctrl Pts',(-2.47009394478667,2.0854759631843,35.7995028679659));
#22197=CARTESIAN_POINT('Ctrl Pts',(-2.62663991601537,1.8844978151653,35.8170272932151));
#22198=CARTESIAN_POINT('Ctrl Pts',(-2.78717237984905,1.61894177903155,35.8373288032252));
#22199=CARTESIAN_POINT('Ctrl Pts',(-2.81509616944046,1.56988433892823,35.8409682944937));
#22200=CARTESIAN_POINT('Ctrl Pts',(-2.84722706337797,1.50981852463014,35.8452700206613));
#22201=CARTESIAN_POINT('Ctrl Pts',(-2.8526792567236,1.49949157912259,35.8460041995074));
#22202=CARTESIAN_POINT('Ctrl Pts',(-2.86108165915521,1.48336496995739,35.8471420350367));
#22203=CARTESIAN_POINT('Ctrl Pts',(-2.86407057471238,1.47758574685005,35.8475480744458));
#22204=CARTESIAN_POINT('Ctrl Pts',(-2.86959073405829,1.46683254934182,35.8483003279048));
#22205=CARTESIAN_POINT('Ctrl Pts',(-2.87212653543665,1.46186109940702,35.8486468205337));
#22206=CARTESIAN_POINT('Ctrl Pts',(-2.87784626086216,1.45057521985763,35.8494305058163));
#22207=CARTESIAN_POINT('Ctrl Pts',(-2.88102231595407,1.44425689780227,35.8498672014981));
#22208=CARTESIAN_POINT('Ctrl Pts',(-2.89038546486611,1.42547641484685,35.8511593211402));
#22209=CARTESIAN_POINT('Ctrl Pts',(-2.89651277506788,1.41298439653568,35.8520110931471));
#22210=CARTESIAN_POINT('Ctrl Pts',(-2.94236488448253,1.31795195014025,35.8584356891103));
#22211=CARTESIAN_POINT('Ctrl Pts',(-2.97863920195295,1.23378293082401,35.8638116284189));
#22212=CARTESIAN_POINT('Ctrl Pts',(-3.09796907748042,0.920820293972021,
35.8830722180209));
#22213=CARTESIAN_POINT('Ctrl Pts',(-3.15863409748303,0.684372923629414,
35.896298481329));
#22214=CARTESIAN_POINT('Ctrl Pts',(-3.20474754755038,0.352348715279247,
35.9153828810517));
#22215=CARTESIAN_POINT('Ctrl Pts',(-3.21348774603249,0.260865942913228,
35.9206853786294));
#22216=CARTESIAN_POINT('Ctrl Pts',(-3.22125103730935,0.113149652394659,
35.9294079034964));
#22217=CARTESIAN_POINT('Ctrl Pts',(-3.22273185991701,0.0570952960618219,
35.9327545369201));
#22218=CARTESIAN_POINT('Ctrl Pts',(-3.22275533909513,-0.0161359277741507,
35.9371859942254));
#22219=CARTESIAN_POINT('Ctrl Pts',(-3.22262364041845,-0.0333046288324061,
35.9382291637872));
#22220=CARTESIAN_POINT('Ctrl Pts',(-3.22218487970022,-0.0613174874208513,
35.9399384538424));
#22221=CARTESIAN_POINT('Ctrl Pts',(-3.22196023686762,-0.0721627377965504,
35.9406019782694));
#22222=CARTESIAN_POINT('Ctrl Pts',(-3.22142124196038,-0.0930824086395146,
35.9418853624112));
#22223=CARTESIAN_POINT('Ctrl Pts',(-3.2211143726453,-0.10315690769907,35.9425049793255));
#22224=CARTESIAN_POINT('Ctrl Pts',(-3.22030020351147,-0.126315525354007,
35.9439329850104));
#22225=CARTESIAN_POINT('Ctrl Pts',(-3.21976041510896,-0.139398256247839,
35.9447423864189));
#22226=CARTESIAN_POINT('Ctrl Pts',(-3.21810443471131,-0.174359777866476,
35.9469127498439));
#22227=CARTESIAN_POINT('Ctrl Pts',(-3.21684487112074,-0.196230786862113,
35.948278192795));
#22228=CARTESIAN_POINT('Ctrl Pts',(-3.20426121056356,-0.381757946721685,
35.9599284392866));
#22229=CARTESIAN_POINT('Ctrl Pts',(-3.18068132286312,-0.544316657537262,
35.9706014164879));
#22230=CARTESIAN_POINT('Ctrl Pts',(-3.0892667155855,-0.952469482132061,
35.998499587124));
#22231=CARTESIAN_POINT('Ctrl Pts',(-3.00453278854938,-1.19312402986472,
36.0160512963132));
#22232=CARTESIAN_POINT('Ctrl Pts',(-2.86773749741407,-1.47150484730143,
36.0363383813135));
#22233=CARTESIAN_POINT('Ctrl Pts',(-2.84177029808648,-1.52104810623624,
36.0399440790494));
#22234=CARTESIAN_POINT('Ctrl Pts',(-2.80885164644733,-1.58006507235858,
36.0442113504063));
#22235=CARTESIAN_POINT('Ctrl Pts',(-2.8031230808684,-1.59020571245238,36.0449435571804));
#22236=CARTESIAN_POINT('Ctrl Pts',(-2.79411210041919,-1.60595684151635,
36.0460790076063));
#22237=CARTESIAN_POINT('Ctrl Pts',(-2.7908675420878,-1.61158871019074,36.0464846181944));
#22238=CARTESIAN_POINT('Ctrl Pts',(-2.78480502505577,-1.62203874467475,
36.0472364846307));
#22239=CARTESIAN_POINT('Ctrl Pts',(-2.78199161484652,-1.62685935852861,
36.0475830165017));
#22240=CARTESIAN_POINT('Ctrl Pts',(-2.77558059952186,-1.63777899505023,
36.0483673095912));
#22241=CARTESIAN_POINT('Ctrl Pts',(-2.77197541752484,-1.64387347079022,
36.0488045706096));
#22242=CARTESIAN_POINT('Ctrl Pts',(-2.76120457265491,-1.66194514565416,
36.0500999161951));
#22243=CARTESIAN_POINT('Ctrl Pts',(-2.75398105038895,-1.67388791430352,
36.050954321706));
#22244=CARTESIAN_POINT('Ctrl Pts',(-2.69807807434776,-1.76497171935793,
36.0574610713057));
#22245=CARTESIAN_POINT('Ctrl Pts',(-2.64606923707545,-1.84202919295389,
36.0629107944885));
#22246=CARTESIAN_POINT('Ctrl Pts',(-2.44705131726415,-2.11103574983077,
36.0821409989197));
#22247=CARTESIAN_POINT('Ctrl Pts',(-2.28190073615814,-2.28855277342994,
36.0952837718125));
#22248=CARTESIAN_POINT('Ctrl Pts',(-2.02860552848562,-2.50586217024917,
36.1142829562129));
#22249=CARTESIAN_POINT('Ctrl Pts',(-1.95623474136634,-2.56275814472599,
36.119594215877));
#22250=CARTESIAN_POINT('Ctrl Pts',(-1.83595694390226,-2.6492510166241,36.1283298372918));
#22251=CARTESIAN_POINT('Ctrl Pts',(-1.78953488430647,-2.68082695623838,
36.1316805162257));
#22252=CARTESIAN_POINT('Ctrl Pts',(-1.72786376367948,-2.72045941322018,
36.1361165850886));
#22253=CARTESIAN_POINT('Ctrl Pts',(-1.71333981160578,-2.7296298791251,36.1371602105065));
#22254=CARTESIAN_POINT('Ctrl Pts',(-1.68952376613095,-2.74440243281156,
36.1388700598438));
#22255=CARTESIAN_POINT('Ctrl Pts',(-1.68027534400173,-2.75007455050425,
36.1395336844176));
#22256=CARTESIAN_POINT('Ctrl Pts',(-1.66238055990656,-2.7609255721317,36.140817130465));
#22257=CARTESIAN_POINT('Ctrl Pts',(-1.65373818681447,-2.76611083411253,
36.1414367084293));
#22258=CARTESIAN_POINT('Ctrl Pts',(-1.63381552198751,-2.77793731968781,
36.1428644354347));
#22259=CARTESIAN_POINT('Ctrl Pts',(-1.62251886347597,-2.784550491828,36.1436735958224));
#22260=CARTESIAN_POINT('Ctrl Pts',(-1.59222088829513,-2.80204024783262,
36.145842892712));
#22261=CARTESIAN_POINT('Ctrl Pts',(-1.57314875726316,-2.81279218160706,
36.1472075032309));
#22262=CARTESIAN_POINT('Ctrl Pts',(-1.52791931900792,-2.83768642883583,
36.1504420200467));
#22263=CARTESIAN_POINT('Ctrl Pts',(-1.50167885936097,-2.85165942216976,
36.1523172954271));
#22264=CARTESIAN_POINT('Ctrl Pts',(-1.47525533429856,-2.86526425676998,
36.1542047394732));
#22265=CARTESIAN_POINT('Origin',(0.,0.,4.68922655072688));
#22266=CARTESIAN_POINT('',(-1.47642198135621,-2.8675770180324,37.6538374877124));
#22267=CARTESIAN_POINT('',(-1.47525540431025,-2.86526422072265,37.4085260041042));
#22268=CARTESIAN_POINT('',(-1.47525540501186,-2.86526422036142,4.68922655072688));
#22269=CARTESIAN_POINT('',(3.22710931890567,0.00161487490920624,36.8107734492731));
#22270=CARTESIAN_POINT('Ctrl Pts',(3.22710931890567,0.00161487490920624,
36.8107734492731));
#22271=CARTESIAN_POINT('Ctrl Pts',(3.22766820945557,0.092902302212634,36.8164301670323));
#22272=CARTESIAN_POINT('Ctrl Pts',(3.18268013141034,1.25374923679401,36.8883978642459));
#22273=CARTESIAN_POINT('Ctrl Pts',(1.77912732379145,3.37157490318388,37.0266765409141));
#22274=CARTESIAN_POINT('Ctrl Pts',(-1.875636683147,3.31885498005365,37.2256094792775));
#22275=CARTESIAN_POINT('Ctrl Pts',(-3.806119388409,0.2150966389413,37.4245424176409));
#22276=CARTESIAN_POINT('Ctrl Pts',(-2.68065523427354,-2.1538654548464,37.5672850871192));
#22277=CARTESIAN_POINT('Ctrl Pts',(-1.62254331928945,-2.79407246625599,
37.6437167771431));
#22278=CARTESIAN_POINT('Ctrl Pts',(-1.47642198135613,-2.86757701803244,
37.6538374877124));
#22279=CARTESIAN_POINT('Ctrl Pts',(3.22274952067548,0.00175769336351857,
36.8082682062519));
#22280=CARTESIAN_POINT('Ctrl Pts',(3.22276605484594,-0.0285578844381251,
36.80650283569));
#22281=CARTESIAN_POINT('Ctrl Pts',(3.22235483219543,-0.05887312616645,36.8047522247304));
#22282=CARTESIAN_POINT('Ctrl Pts',(3.21327137318411,-0.387005561556071,
36.7859214086916));
#22283=CARTESIAN_POINT('Ctrl Pts',(3.16376992247395,-0.68224905193963,36.7698842931772));
#22284=CARTESIAN_POINT('Ctrl Pts',(3.04938585646319,-1.04609995332455,36.7476979918744));
#22285=CARTESIAN_POINT('Ctrl Pts',(3.02128342954484,-1.1246883395346,36.742763256182));
#22286=CARTESIAN_POINT('Ctrl Pts',(2.98285032186027,-1.22028936190716,36.7365420512188));
#22287=CARTESIAN_POINT('Ctrl Pts',(2.9753694133729,-1.23841794118675,36.7353524918587));
#22288=CARTESIAN_POINT('Ctrl Pts',(2.96328290429647,-1.266965558166,36.7334631611481));
#22289=CARTESIAN_POINT('Ctrl Pts',(2.95878664247503,-1.27743058344845,36.7327671204464));
#22290=CARTESIAN_POINT('Ctrl Pts',(2.95025209269912,-1.2970078992249,36.7314584368492));
#22291=CARTESIAN_POINT('Ctrl Pts',(2.94622681528071,-1.30612574068935,36.7308462461957));
#22292=CARTESIAN_POINT('Ctrl Pts',(2.93712178009111,-1.32649371637484,36.7294725934711));
#22293=CARTESIAN_POINT('Ctrl Pts',(2.93201957254121,-1.33773358711513,36.7287103643352));
#22294=CARTESIAN_POINT('Ctrl Pts',(2.91892192023341,-1.36615204620692,36.7267723867528));
#22295=CARTESIAN_POINT('Ctrl Pts',(2.91083939729689,-1.38328976290622,36.7255936367331));
#22296=CARTESIAN_POINT('Ctrl Pts',(2.86351639764259,-1.48137920989517,36.7187880237311));
#22297=CARTESIAN_POINT('Ctrl Pts',(2.82105450547159,-1.56072400536159,36.7130492195396));
#22298=CARTESIAN_POINT('Ctrl Pts',(2.63326649012482,-1.87886563895286,36.6890430908086));
#22299=CARTESIAN_POINT('Ctrl Pts',(2.46050134454939,-2.10002863479042,36.669822646677));
#22300=CARTESIAN_POINT('Ctrl Pts',(2.20945924073325,-2.34728117032595,36.6462732745994));
#22301=CARTESIAN_POINT('Ctrl Pts',(2.1557594856927,-2.39669386755196,36.6414506258617));
#22302=CARTESIAN_POINT('Ctrl Pts',(2.0804396760161,-2.46141884193578,36.6350203875209));
#22303=CARTESIAN_POINT('Ctrl Pts',(2.0602432364287,-2.47834821289421,36.6333272889481));
#22304=CARTESIAN_POINT('Ctrl Pts',(2.02986562523331,-2.50318379611761,36.6308294108307));
#22305=CARTESIAN_POINT('Ctrl Pts',(2.01984151149068,-2.51127932629666,36.6300128964112));
#22306=CARTESIAN_POINT('Ctrl Pts',(2.00160723725369,-2.52582561469292,36.6285419920877));
#22307=CARTESIAN_POINT('Ctrl Pts',(1.99341382175586,-2.5322969633083,36.6278862401827));
#22308=CARTESIAN_POINT('Ctrl Pts',(1.98027247466594,-2.54257299615543,36.6268429385855));
#22309=CARTESIAN_POINT('Ctrl Pts',(1.97534477213949,-2.54640325703751,36.62645360774));
#22310=CARTESIAN_POINT('Ctrl Pts',(1.96619282674201,-2.5534744324519,36.6257340567563));
#22311=CARTESIAN_POINT('Ctrl Pts',(1.96197172778946,-2.55671915723209,36.6254035717015));
#22312=CARTESIAN_POINT('Ctrl Pts',(1.95207787242992,-2.56428555302981,36.624632163286));
#22313=CARTESIAN_POINT('Ctrl Pts',(1.94639880479212,-2.56859886173743,36.624191832511));
#22314=CARTESIAN_POINT('Ctrl Pts',(1.92899148777409,-2.58172901126351,36.6228494776079));
#22315=CARTESIAN_POINT('Ctrl Pts',(1.91721711122963,-2.59048478375062,36.6219516327591));
#22316=CARTESIAN_POINT('Ctrl Pts',(1.75489781846419,-2.70947723984751,36.6097061108786));
#22317=CARTESIAN_POINT('Ctrl Pts',(1.59509190662659,-2.80653453996464,36.5991877727189));
#22318=CARTESIAN_POINT('Ctrl Pts',(1.2958759370638,-2.95439752107189,36.5805075949685));
#22319=CARTESIAN_POINT('Ctrl Pts',(1.15968358011756,-3.01046368765049,36.5723406741485));
#22320=CARTESIAN_POINT('Ctrl Pts',(0.932892404282599,-3.08614478306714,
36.5587297343269));
#22321=CARTESIAN_POINT('Ctrl Pts',(0.844441674176579,-3.111509952806,36.5534208244709));
#22322=CARTESIAN_POINT('Ctrl Pts',(0.700471980442569,-3.14620505278839,
36.5446884902619));
#22323=CARTESIAN_POINT('Ctrl Pts',(0.645580608867946,-3.15792532051728,
36.5413386643411));
#22324=CARTESIAN_POINT('Ctrl Pts',(0.573525407193728,-3.17135322634818,
36.536903343233));
#22325=CARTESIAN_POINT('Ctrl Pts',(0.556612567602607,-3.17436530833754,
36.5358595874755));
#22326=CARTESIAN_POINT('Ctrl Pts',(0.52897770913344,-3.17905928174248,36.5341494268078));
#22327=CARTESIAN_POINT('Ctrl Pts',(0.518269707133551,-3.18082250993434,
36.5334856213996));
#22328=CARTESIAN_POINT('Ctrl Pts',(0.497596464884699,-3.18411949787508,
36.5322017561688));
#22329=CARTESIAN_POINT('Ctrl Pts',(0.487632518424355,-3.18566064449777,
36.5315819396622));
#22330=CARTESIAN_POINT('Ctrl Pts',(0.464709565415272,-3.18909612670047,
36.5301535621975));
#22331=CARTESIAN_POINT('Ctrl Pts',(0.451745981609123,-3.19095826445369,
36.5293439885043));
#22332=CARTESIAN_POINT('Ctrl Pts',(0.417066885607546,-3.19572413789937,
36.5271733542962));
#22333=CARTESIAN_POINT('Ctrl Pts',(0.395332806374885,-3.19848549887924,
36.5258078129339));
#22334=CARTESIAN_POINT('Ctrl Pts',(0.210804253310464,-3.2200207344675,36.5141683524406));
#22335=CARTESIAN_POINT('Ctrl Pts',(0.0468498156986263,-3.22657130235436,
36.5035071245191));
#22336=CARTESIAN_POINT('Ctrl Pts',(-0.370926724992662,-3.21141096296261,
36.4756243991621));
#22337=CARTESIAN_POINT('Ctrl Pts',(-0.622986109466305,-3.17216495732823,
36.4580755360971));
#22338=CARTESIAN_POINT('Ctrl Pts',(-0.921844436026495,-3.08860298168915,
36.4377768145144));
#22339=CARTESIAN_POINT('Ctrl Pts',(-0.975479136866018,-3.07208510679403,
36.4341589201158));
#22340=CARTESIAN_POINT('Ctrl Pts',(-1.03970943635549,-3.05045206800001,
36.4298790289116));
#22341=CARTESIAN_POINT('Ctrl Pts',(-1.05073997555764,-3.04667015687418,
36.4291459310195));
#22342=CARTESIAN_POINT('Ctrl Pts',(-1.06789081565318,-3.04068562500645,
36.4280093161713));
#22343=CARTESIAN_POINT('Ctrl Pts',(-1.07402525303346,-3.03852425066817,
36.4276034256032));
#22344=CARTESIAN_POINT('Ctrl Pts',(-1.0854135811211,-3.03447295164859,36.4268511698193));
#22345=CARTESIAN_POINT('Ctrl Pts',(-1.09066905278063,-3.03258796317373,
36.4265045275812));
#22346=CARTESIAN_POINT('Ctrl Pts',(-1.10257831092685,-3.02828148707774,
36.425720142159));
#22347=CARTESIAN_POINT('Ctrl Pts',(-1.10922901640343,-3.02585172937019,
36.4252828985485));
#22348=CARTESIAN_POINT('Ctrl Pts',(-1.12895768572347,-3.01857030311774,
36.4239880705158));
#22349=CARTESIAN_POINT('Ctrl Pts',(-1.14201241672374,-3.01365555221201,
36.4231341595343));
#22350=CARTESIAN_POINT('Ctrl Pts',(-1.24129942132,-2.9755388743415,36.4166589295455));
#22351=CARTESIAN_POINT('Ctrl Pts',(-1.32610848080994,-2.93872346122117,
36.4112379686349));
#22352=CARTESIAN_POINT('Ctrl Pts',(-1.4313674177628,-2.8875441186618,36.4045101853076));
#22353=CARTESIAN_POINT('Ctrl Pts',(-1.45337870525942,-2.87652800565308,
36.4031033493262));
#22354=CARTESIAN_POINT('Ctrl Pts',(-1.47525545662511,-2.865264193787,36.4017031386693));
#22355=CARTESIAN_POINT('Ctrl Pts',(-1.47525533429857,-2.86526425676998,
36.1542047394732));
#22356=CARTESIAN_POINT('Ctrl Pts',(-1.35648519049259,-2.92641613405012,
36.1626885432144));
#22357=CARTESIAN_POINT('Ctrl Pts',(-1.23401696002696,-2.98012972438504,
36.171426215797));
#22358=CARTESIAN_POINT('Ctrl Pts',(-0.871056753745843,-3.11309363011468,
36.1972043428991));
#22359=CARTESIAN_POINT('Ctrl Pts',(-0.62415665607532,-3.17183152281709,
36.2146603565864));
#22360=CARTESIAN_POINT('Ctrl Pts',(-0.315582863209829,-3.20778098899618,
36.2349996513337));
#22361=CARTESIAN_POINT('Ctrl Pts',(-0.258057652374377,-3.21292057905945,
36.2387254237883));
#22362=CARTESIAN_POINT('Ctrl Pts',(-0.188689003787312,-3.21724295097161,
36.2431149691367));
#22363=CARTESIAN_POINT('Ctrl Pts',(-0.176952494959484,-3.21790981388537,
36.2438540833031));
#22364=CARTESIAN_POINT('Ctrl Pts',(-0.158697769992497,-3.21884686376737,
36.2449978860274));
#22365=CARTESIAN_POINT('Ctrl Pts',(-0.152182082262523,-3.21916149489491,
36.2454049970216));
#22366=CARTESIAN_POINT('Ctrl Pts',(-0.140091921436821,-3.21970851840367,
36.2461582237465));
#22367=CARTESIAN_POINT('Ctrl Pts',(-0.134517851565134,-3.21994621667609,
36.246504624429));
#22368=CARTESIAN_POINT('Ctrl Pts',(-0.121899983884943,-3.22045146537396,
36.2472868186752));
#22369=CARTESIAN_POINT('Ctrl Pts',(-0.114855926478386,-3.22071038208709,
36.2477221232154));
#22370=CARTESIAN_POINT('Ctrl Pts',(-0.0940122937803075,-3.2214080568381,
36.2490063209519));
#22371=CARTESIAN_POINT('Ctrl Pts',(-0.0802104780147182,-3.2217812581072,
36.249851628328));
#22372=CARTESIAN_POINT('Ctrl Pts',(0.0221298499941792,-3.22389048050423,
36.2560850492217));
#22373=CARTESIAN_POINT('Ctrl Pts',(0.110712612917276,-3.22206538514645,
36.2612892835029));
#22374=CARTESIAN_POINT('Ctrl Pts',(0.445915510658712,-3.2013154222992,36.2806307746532));
#22375=CARTESIAN_POINT('Ctrl Pts',(0.690145716217482,-3.15768500635991,
36.2940591626006));
#22376=CARTESIAN_POINT('Ctrl Pts',(1.01452756133985,-3.06026212167359,36.3133462070023));
#22377=CARTESIAN_POINT('Ctrl Pts',(1.10089540739617,-3.03026365611643,36.3186227453361));
#22378=CARTESIAN_POINT('Ctrl Pts',(1.23781003456563,-2.97608206240529,36.327306455389));
#22379=CARTESIAN_POINT('Ctrl Pts',(1.28920685994301,-2.95418063542867,36.3306410855843));
#22380=CARTESIAN_POINT('Ctrl Pts',(1.35560046236527,-2.92382608149794,36.3350588579925));
#22381=CARTESIAN_POINT('Ctrl Pts',(1.37113718712766,-2.91657236577657,36.3361006719362));
#22382=CARTESIAN_POINT('Ctrl Pts',(1.39640277016724,-2.90452998414118,36.337808298884));
#22383=CARTESIAN_POINT('Ctrl Pts',(1.40616678114284,-2.89981552936949,36.3384715255641));
#22384=CARTESIAN_POINT('Ctrl Pts',(1.42496266930354,-2.89062287066295,36.3397547264029));
#22385=CARTESIAN_POINT('Ctrl Pts',(1.43399770170545,-2.88615137806843,36.3403744598718));
#22386=CARTESIAN_POINT('Ctrl Pts',(1.45472976009375,-2.87576957325743,36.341803297677));
#22387=CARTESIAN_POINT('Ctrl Pts',(1.46641195118515,-2.86983018568026,36.342613418507));
#22388=CARTESIAN_POINT('Ctrl Pts',(1.49755967260083,-2.85375441088964,36.3447869664951));
#22389=CARTESIAN_POINT('Ctrl Pts',(1.51695816490364,-2.84349030209702,36.3461548952742));
#22390=CARTESIAN_POINT('Ctrl Pts',(1.68083909316897,-2.75462355953177,36.357835068579));
#22391=CARTESIAN_POINT('Ctrl Pts',(1.81919097537173,-2.66527678924624,36.3685375908901));
#22392=CARTESIAN_POINT('Ctrl Pts',(2.15338260351415,-2.41127628278103,36.3965392768757));
#22393=CARTESIAN_POINT('Ctrl Pts',(2.33757028432234,-2.23317501815466,36.4141675774876));
#22394=CARTESIAN_POINT('Ctrl Pts',(2.53323312048606,-1.99294232868106,36.4344160582179));
#22395=CARTESIAN_POINT('Ctrl Pts',(2.56658298813822,-1.94980557244468,36.4379287022976));
#22396=CARTESIAN_POINT('Ctrl Pts',(2.60566044690566,-1.89651913145639,36.4421009236364));
#22397=CARTESIAN_POINT('Ctrl Pts',(2.61244621916695,-1.88716081510612,36.4428275825417));
#22398=CARTESIAN_POINT('Ctrl Pts',(2.62295753273703,-1.87249922315853,36.4439563210097));
#22399=CARTESIAN_POINT('Ctrl Pts',(2.62671759778278,-1.86722098920448,36.4443607233275));
#22400=CARTESIAN_POINT('Ctrl Pts',(2.63368774521397,-1.85737384537279,36.4451115070263));
#22401=CARTESIAN_POINT('Ctrl Pts',(2.63690184234078,-1.85280798122805,36.4454581572087));
#22402=CARTESIAN_POINT('Ctrl Pts',(2.64418024368227,-1.84241116954627,36.4462441981131));
#22403=CARTESIAN_POINT('Ctrl Pts',(2.64823712627546,-1.83657512888788,36.4466830793902));
#22404=CARTESIAN_POINT('Ctrl Pts',(2.65871239544762,-1.82139902013144,36.447818410412));
#22405=CARTESIAN_POINT('Ctrl Pts',(2.66510094696543,-1.81203833942282,36.4485128787553));
#22406=CARTESIAN_POINT('Ctrl Pts',(2.70510337492795,-1.75275647877739,36.4528757988539));
#22407=CARTESIAN_POINT('Ctrl Pts',(2.73736513833007,-1.70193205234039,36.4564596009306));
#22408=CARTESIAN_POINT('Ctrl Pts',(2.93892976009823,-1.36381649689437,36.4794989374551));
#22409=CARTESIAN_POINT('Ctrl Pts',(3.06420210421427,-1.05262467792409,36.4972114672141));
#22410=CARTESIAN_POINT('Ctrl Pts',(3.15914205093584,-0.643036144895613,
36.521630007708));
#22411=CARTESIAN_POINT('Ctrl Pts',(3.17533518873855,-0.557600584126361,
36.526765492885));
#22412=CARTESIAN_POINT('Ctrl Pts',(3.19095975778362,-0.451981742642096,
36.533210627656));
#22413=CARTESIAN_POINT('Ctrl Pts',(3.19368337042743,-0.43231721414448,36.5344146060057));
#22414=CARTESIAN_POINT('Ctrl Pts',(3.19768988748429,-0.401282733161163,
36.5363215020611));
#22415=CARTESIAN_POINT('Ctrl Pts',(3.19909424851081,-0.389928752815022,
36.5370205673367));
#22416=CARTESIAN_POINT('Ctrl Pts',(3.20160785947631,-0.368678505116161,
36.5383317097633));
#22417=CARTESIAN_POINT('Ctrl Pts',(3.20273175667167,-0.358784081663207,
36.5389433152643));
#22418=CARTESIAN_POINT('Ctrl Pts',(3.2051375239809,-0.336691909387495,36.5403114660003));
#22419=CARTESIAN_POINT('Ctrl Pts',(3.20639565045291,-0.324491780416018,
36.5410687525325));
#22420=CARTESIAN_POINT('Ctrl Pts',(3.20939615766952,-0.293672553523231,
36.5429862892245));
#22421=CARTESIAN_POINT('Ctrl Pts',(3.21104615788522,-0.275045112098162,
36.5441494336786));
#22422=CARTESIAN_POINT('Ctrl Pts',(3.21939660122333,-0.170421113847801,
36.5507066252172));
#22423=CARTESIAN_POINT('Ctrl Pts',(3.2228039392682,-0.0842040481459283,
36.5562032879677));
#22424=CARTESIAN_POINT('Ctrl Pts',(3.22263357550004,0.184970274485804,36.5736660170257));
#22425=CARTESIAN_POINT('Ctrl Pts',(3.20694277966631,0.367538399943799,36.5859673833119));
#22426=CARTESIAN_POINT('Ctrl Pts',(3.15894344069144,0.645829823717705,36.6050828408999));
#22427=CARTESIAN_POINT('Ctrl Pts',(3.13749662835673,0.743058334153712,36.6118258198534));
#22428=CARTESIAN_POINT('Ctrl Pts',(3.10457565432211,0.865131329287124,36.620278234588));
#22429=CARTESIAN_POINT('Ctrl Pts',(3.09724088761861,0.89103375506053,36.6220708041795));
#22430=CARTESIAN_POINT('Ctrl Pts',(3.06654473160006,0.994473963037814,36.6292184191876));
#22431=CARTESIAN_POINT('Ctrl Pts',(3.04058708029015,1.07121786073489,36.6344970946243));
#22432=CARTESIAN_POINT('Ctrl Pts',(3.00695581531393,1.15953299579155,36.6404799419706));
#22433=CARTESIAN_POINT('Ctrl Pts',(3.00206897881807,1.17212708571676,36.6413308873444));
#22434=CARTESIAN_POINT('Ctrl Pts',(2.99453543051912,1.19118592291648,36.6426148360029));
#22435=CARTESIAN_POINT('Ctrl Pts',(2.99194672477672,1.19767322165597,36.6430511985206));
#22436=CARTESIAN_POINT('Ctrl Pts',(2.9872538715903,1.20932334375856,36.6438335579084));
#22437=CARTESIAN_POINT('Ctrl Pts',(2.98515741117633,1.21448914159256,36.6441800079051));
#22438=CARTESIAN_POINT('Ctrl Pts',(2.98056009655472,1.22573336116057,36.6449331118216));
#22439=CARTESIAN_POINT('Ctrl Pts',(2.9780540571047,1.23180956183125,36.6453394461138));
#22440=CARTESIAN_POINT('Ctrl Pts',(2.97092667178849,1.24894189853023,36.6464834692871));
#22441=CARTESIAN_POINT('Ctrl Pts',(2.96626216830768,1.2599801246071,36.6472185866358));
#22442=CARTESIAN_POINT('Ctrl Pts',(2.93716503604649,1.32777928414764,36.651723219759));
#22443=CARTESIAN_POINT('Ctrl Pts',(2.91116378962115,1.38385794959682,36.6554032242125));
#22444=CARTESIAN_POINT('Ctrl Pts',(2.76347261567103,1.67977881225645,36.6747539223773));
#22445=CARTESIAN_POINT('Ctrl Pts',(2.61372736611706,1.90444108728551,36.6892804506745));
#22446=CARTESIAN_POINT('Ctrl Pts',(2.34376095287608,2.21665787511883,36.7127248839091));
#22447=CARTESIAN_POINT('Ctrl Pts',(2.24256419857794,2.31898376879698,36.7210616337054));
#22448=CARTESIAN_POINT('Ctrl Pts',(2.11882836152967,2.4284034428552,36.731000513484));
#22449=CARTESIAN_POINT('Ctrl Pts',(2.10263219673709,2.44244032027682,36.7322965821504));
#22450=CARTESIAN_POINT('Ctrl Pts',(2.07642359732163,2.46470088149511,36.7343868019875));
#22451=CARTESIAN_POINT('Ctrl Pts',(2.0664993079806,2.47302769761647,36.735176696898));
#22452=CARTESIAN_POINT('Ctrl Pts',(2.04878125856672,2.48771262000182,36.7365842272608));
#22453=CARTESIAN_POINT('Ctrl Pts',(2.04100738834421,2.49409453755293,36.7372008800983));
#22454=CARTESIAN_POINT('Ctrl Pts',(2.02473884915917,2.50732311237492,36.7384895474435));
#22455=CARTESIAN_POINT('Ctrl Pts',(2.016239043971,2.51416322262954,36.7391618156184));
#22456=CARTESIAN_POINT('Ctrl Pts',(1.99405204187911,2.53183305872703,36.7409140909781));
#22457=CARTESIAN_POINT('Ctrl Pts',(1.9803114508983,2.54259487947004,36.7419967975236));
#22458=CARTESIAN_POINT('Ctrl Pts',(1.91997054415686,2.58906886700687,36.7467412015817));
#22459=CARTESIAN_POINT('Ctrl Pts',(1.87248916450982,2.62361355511462,36.7504484297529));
#22460=CARTESIAN_POINT('Ctrl Pts',(1.74328790330577,2.71231859679064,36.7604747270384));
#22461=CARTESIAN_POINT('Ctrl Pts',(1.66000072818877,2.76407660133745,36.7668766405699));
#22462=CARTESIAN_POINT('Ctrl Pts',(1.40766936111291,2.90536384818186,36.786061721988));
#22463=CARTESIAN_POINT('Ctrl Pts',(1.232871877232,2.9837377322838,36.7991106145913));
#22464=CARTESIAN_POINT('Ctrl Pts',(0.926532175384797,3.08955104591862,36.8209196403535));
#22465=CARTESIAN_POINT('Ctrl Pts',(0.798307190894622,3.12514024818465,36.8297459469964));
#22466=CARTESIAN_POINT('Ctrl Pts',(0.653620244386708,3.15580756373062,36.8391233165872));
#22467=CARTESIAN_POINT('Ctrl Pts',(0.638982021735399,3.15880401407526,36.8400654689786));
#22468=CARTESIAN_POINT('Ctrl Pts',(0.617276612328088,3.16309006136898,36.8414522305245));
#22469=CARTESIAN_POINT('Ctrl Pts',(0.610225350643649,3.16445795931336,36.8419011387716));
#22470=CARTESIAN_POINT('Ctrl Pts',(0.597677836891366,3.1668485942409,36.8426970460851));
#22471=CARTESIAN_POINT('Ctrl Pts',(0.592183448714921,3.16788061333103,36.8430445684284));
#22472=CARTESIAN_POINT('Ctrl Pts',(0.58036448649849,3.17006876268273,36.8437899708233));
#22473=CARTESIAN_POINT('Ctrl Pts',(0.574039147667095,3.17122026292387,36.8441875851245));
#22474=CARTESIAN_POINT('Ctrl Pts',(0.55656201494484,3.17434789388611,36.8452826853262));
#22475=CARTESIAN_POINT('Ctrl Pts',(0.545403057365658,3.17628420356421,36.8459779394641));
#22476=CARTESIAN_POINT('Ctrl Pts',(0.48400431868569,3.18660504084151,36.8497827884402));
#22477=CARTESIAN_POINT('Ctrl Pts',(0.433578292551593,3.19385697964606,36.8528320604096));
#22478=CARTESIAN_POINT('Ctrl Pts',(0.126694374032891,3.23058801392747,36.8710472475619));
#22479=CARTESIAN_POINT('Ctrl Pts',(-0.132392916066827,3.23036419740347,
36.8850459308302));
#22480=CARTESIAN_POINT('Ctrl Pts',(-0.553144886143904,3.17924354978906,
36.9089761751536));
#22481=CARTESIAN_POINT('Ctrl Pts',(-0.715783007048575,3.14661767538846,
36.9185165948688));
#22482=CARTESIAN_POINT('Ctrl Pts',(-0.896295515390018,3.09568300091237,
36.9297975036102));
#22483=CARTESIAN_POINT('Ctrl Pts',(-0.917348495585595,3.08950976600439,
36.931123803746));
#22484=CARTESIAN_POINT('Ctrl Pts',(-0.950871975286829,3.07930702346509,
36.9332534381652));
#22485=CARTESIAN_POINT('Ctrl Pts',(-0.963384003351651,3.07541550237927,
36.9340522528097));
#22486=CARTESIAN_POINT('Ctrl Pts',(-0.985479219561552,3.06839532825165,
36.9354700707615));
#22487=CARTESIAN_POINT('Ctrl Pts',(-0.995072167840309,3.06529779299603,
36.9360880416007));
#22488=CARTESIAN_POINT('Ctrl Pts',(-1.01495353803362,3.05877499347314,36.9373738543905));
#22489=CARTESIAN_POINT('Ctrl Pts',(-1.02523950770585,3.05534271274126,36.9380419221032));
#22490=CARTESIAN_POINT('Ctrl Pts',(-1.05174915691184,3.04634788252861,36.9397711234567));
#22491=CARTESIAN_POINT('Ctrl Pts',(-1.06794594537064,3.04070767254742,36.940834825075));
#22492=CARTESIAN_POINT('Ctrl Pts',(-1.13673876207206,3.01613450103769,36.9453839773432));
#22493=CARTESIAN_POINT('Ctrl Pts',(-1.18887980529481,2.99596503961827,36.9489104514787));
#22494=CARTESIAN_POINT('Ctrl Pts',(-1.32490043599684,2.93923888201575,36.958324879121));
#22495=CARTESIAN_POINT('Ctrl Pts',(-1.40778887040859,2.90045072006253,36.9642836859241));
#22496=CARTESIAN_POINT('Ctrl Pts',(-1.70772472929498,2.74420604356364,36.9866514534945));
#22497=CARTESIAN_POINT('Ctrl Pts',(-1.91270368009395,2.60548260354482,37.0036323679565));
#22498=CARTESIAN_POINT('Ctrl Pts',(-2.16733902784523,2.38677102064044,37.0259392947688));
#22499=CARTESIAN_POINT('Ctrl Pts',(-2.23241276480209,2.32602036633145,37.0317570263363));
#22500=CARTESIAN_POINT('Ctrl Pts',(-2.30459826389271,2.25280612658301,37.0382686764267));
#22501=CARTESIAN_POINT('Ctrl Pts',(-2.3142390779141,2.24290127029268,37.0391395910877));
#22502=CARTESIAN_POINT('Ctrl Pts',(-2.32870215248365,2.22784954115069,37.0404475897907));
#22503=CARTESIAN_POINT('Ctrl Pts',(-2.33357158612701,2.22274851201286,37.0408882204375));
#22504=CARTESIAN_POINT('Ctrl Pts',(-2.34226356460735,2.2135830876514,37.0416751359755));
#22505=CARTESIAN_POINT('Ctrl Pts',(-2.346092319323,2.20952472780483,37.0420218979329));
#22506=CARTESIAN_POINT('Ctrl Pts',(-2.35437302294139,2.2007016498423,37.0427721404088));
#22507=CARTESIAN_POINT('Ctrl Pts',(-2.3588210427999,2.19593337162044,37.0431753205467));
#22508=CARTESIAN_POINT('Ctrl Pts',(-2.37123931686889,2.18253970971524,37.0443015737209));
#22509=CARTESIAN_POINT('Ctrl Pts',(-2.37917703781714,2.17388410798806,37.0450222011656));
#22510=CARTESIAN_POINT('Ctrl Pts',(-2.42573118851716,2.12255921522773,37.0492543391556));
#22511=CARTESIAN_POINT('Ctrl Pts',(-2.46324908445984,2.07890219088969,37.0526884271842));
#22512=CARTESIAN_POINT('Ctrl Pts',(-2.65930140451222,1.83800460723727,37.0709110177983));
#22513=CARTESIAN_POINT('Ctrl Pts',(-2.79536817759413,1.62360345248578,37.0846448609797));
#22514=CARTESIAN_POINT('Ctrl Pts',(-2.97573333399933,1.24813681637361,37.1081755874179));
#22515=CARTESIAN_POINT('Ctrl Pts',(-3.03518938676924,1.09565021399464,37.1175957507025));
#22516=CARTESIAN_POINT('Ctrl Pts',(-3.08920302742152,0.918379895379297,
37.1287420858921));
#22517=CARTESIAN_POINT('Ctrl Pts',(-3.09537110838261,0.897370961205556,
37.1300657795763));
#22518=CARTESIAN_POINT('Ctrl Pts',(-3.10488397570805,0.863703896920118,
37.1321920182396));
#22519=CARTESIAN_POINT('Ctrl Pts',(-3.10836660299303,0.851085176480857,
37.1329900665771));
#22520=CARTESIAN_POINT('Ctrl Pts',(-3.11439433102335,0.828714120288518,
37.1344069975532));
#22521=CARTESIAN_POINT('Ctrl Pts',(-3.11697075770407,0.818970350030057,
37.1350248520166));
#22522=CARTESIAN_POINT('Ctrl Pts',(-3.12222555820101,0.798713233184525,
37.1363108945144));
#22523=CARTESIAN_POINT('Ctrl Pts',(-3.12489663064067,0.788198140285589,
37.1369793106554));
#22524=CARTESIAN_POINT('Ctrl Pts',(-3.13165917973631,0.761001547505315,
37.1387104280406));
#22525=CARTESIAN_POINT('Ctrl Pts',(-3.13567044260096,0.744300631681173,
37.1397757080816));
#22526=CARTESIAN_POINT('Ctrl Pts',(-3.15221945776199,0.672889607208716,
37.1443407616012));
#22527=CARTESIAN_POINT('Ctrl Pts',(-3.16345965886952,0.617891803538932,
37.1478819161826));
#22528=CARTESIAN_POINT('Ctrl Pts',(-3.18931977790645,0.472039927098291,
37.1573454942228));
#22529=CARTESIAN_POINT('Ctrl Pts',(-3.20149397223313,0.380809869881011,
37.1633396944617));
#22530=CARTESIAN_POINT('Ctrl Pts',(-3.23146072734248,0.0482064408569172,
37.1854324681332));
#22531=CARTESIAN_POINT('Ctrl Pts',(-3.22596406277041,-0.194430714669504,
37.2020723137423));
#22532=CARTESIAN_POINT('Ctrl Pts',(-3.18088225099349,-0.526024420256396,
37.22434190437));
#22533=CARTESIAN_POINT('Ctrl Pts',(-3.16443211676231,-0.617321996036819,
37.2304125155196));
#22534=CARTESIAN_POINT('Ctrl Pts',(-3.14100181686343,-0.721401250402509,
37.2371701970664));
#22535=CARTESIAN_POINT('Ctrl Pts',(-3.13784956707135,-0.734991352746937,
37.238049324232));
#22536=CARTESIAN_POINT('Ctrl Pts',(-3.13296472537972,-0.755446696316358,
37.2393671989953));
#22537=CARTESIAN_POINT('Ctrl Pts',(-3.1312976444493,-0.762327190639459,
37.2398095715792));
#22538=CARTESIAN_POINT('Ctrl Pts',(-3.12827571303548,-0.774622345565591,
37.24059836306));
#22539=CARTESIAN_POINT('Ctrl Pts',(-3.12692946109608,-0.780039013078377,
37.240945268769));
#22540=CARTESIAN_POINT('Ctrl Pts',(-3.12398479059021,-0.791756810987841,
37.2416944183312));
#22541=CARTESIAN_POINT('Ctrl Pts',(-3.1223813824102,-0.798056592057209,
37.242096369373));
#22542=CARTESIAN_POINT('Ctrl Pts',(-3.11785094746984,-0.815633975101017,
37.243215721764));
#22543=CARTESIAN_POINT('Ctrl Pts',(-3.11488177370662,-0.826900754306286,
37.2439307256483));
#22544=CARTESIAN_POINT('Ctrl Pts',(-3.09728790003992,-0.89222251294425,
37.2480630269886));
#22545=CARTESIAN_POINT('Ctrl Pts',(-3.08131642639808,-0.945908721459504,
37.2514070996175));
#22546=CARTESIAN_POINT('Ctrl Pts',(-2.98515110660766,-1.24080389563577,
37.2696241341481));
#22547=CARTESIAN_POINT('Ctrl Pts',(-2.87803202414719,-1.47230447864389,
37.2834171147081));
#22548=CARTESIAN_POINT('Ctrl Pts',(-2.65885976161363,-1.82851934396009,
37.3070405146908));
#22549=CARTESIAN_POINT('Ctrl Pts',(-2.56238400196479,-1.96142702769182,
37.3164913659328));
#22550=CARTESIAN_POINT('Ctrl Pts',(-2.44203953090745,-2.10310256496634,
37.3276720280684));
#22551=CARTESIAN_POINT('Ctrl Pts',(-2.42768750438157,-2.11965346555868,
37.328996392058));
#22552=CARTESIAN_POINT('Ctrl Pts',(-2.40448948106646,-2.14586097999958,
37.3311235040547));
#22553=CARTESIAN_POINT('Ctrl Pts',(-2.39575127014583,-2.15561240804024,
37.3319217495112));
#22554=CARTESIAN_POINT('Ctrl Pts',(-2.3801819403947,-2.17277543323153,37.3333389085882));
#22555=CARTESIAN_POINT('Ctrl Pts',(-2.37337498200137,-2.18020878444696,
37.3339567929294));
#22556=CARTESIAN_POINT('Ctrl Pts',(-2.35916991163932,-2.19557567899414,
37.3352427760587));
#22557=CARTESIAN_POINT('Ctrl Pts',(-2.35176639903119,-2.20350403538454,
37.3359111023494));
#22558=CARTESIAN_POINT('Ctrl Pts',(-2.33254173034325,-2.2238843106004,37.3376417256947));
#22559=CARTESIAN_POINT('Ctrl Pts',(-2.3206609577078,-2.23627928750168,37.3387065987548));
#22560=CARTESIAN_POINT('Ctrl Pts',(-2.26956127909485,-2.28874483413571,
37.3432675469909));
#22561=CARTESIAN_POINT('Ctrl Pts',(-2.22940126084228,-2.32788116026025,
37.3468049107828));
#22562=CARTESIAN_POINT('Ctrl Pts',(-2.12079814275964,-2.4283271441839,37.3562557881338));
#22563=CARTESIAN_POINT('Ctrl Pts',(-2.05072260321249,-2.48778852983414,
37.3622408391819));
#22564=CARTESIAN_POINT('Ctrl Pts',(-1.82076289780361,-2.66659256755328,
37.3815103996241));
#22565=CARTESIAN_POINT('Ctrl Pts',(-1.65238201600226,-2.77406600268191,
37.3951166831969));
#22566=CARTESIAN_POINT('Ctrl Pts',(-1.47525540431025,-2.86526422072266,
37.4085260041042));
#22567=CARTESIAN_POINT('Origin',(0.,0.,4.68922655072688));
#22568=CARTESIAN_POINT('',(-1.47525540693158,-2.86526421937299,38.9066255640146));
#22569=CARTESIAN_POINT('',(-1.47525532932069,-2.86526425933297,38.6590632205222));
#22570=CARTESIAN_POINT('',(-1.47525540501186,-2.86526422036142,4.68922655072688));
#22571=CARTESIAN_POINT('',(3.22389497588569,-0.002876326465697,38.0607734492731));
#22572=CARTESIAN_POINT('Ctrl Pts',(-1.47525540693158,-2.86526421937299,
38.9066255640146));
#22573=CARTESIAN_POINT('Ctrl Pts',(-1.49002538501413,-2.85765951406197,
38.9055720617144));
#22574=CARTESIAN_POINT('Ctrl Pts',(-1.50473664835218,-2.84994055882525,
38.9045146246307));
#22575=CARTESIAN_POINT('Ctrl Pts',(-1.60015608991765,-2.79892942837589,
38.8976026072713));
#22576=CARTESIAN_POINT('Ctrl Pts',(-1.67904034790546,-2.75233109776619,
38.8916367201395));
#22577=CARTESIAN_POINT('Ctrl Pts',(-1.96192576918629,-2.56853496469414,
38.8693234378444));
#22578=CARTESIAN_POINT('Ctrl Pts',(-2.1520078611904,-2.4115080988086,38.8524102832026));
#22579=CARTESIAN_POINT('Ctrl Pts',(-2.38458425665035,-2.16977467697611,
38.8301117544657));
#22580=CARTESIAN_POINT('Ctrl Pts',(-2.4440582674071,-2.10255715944651,38.8242448859708));
#22581=CARTESIAN_POINT('Ctrl Pts',(-2.50939236403878,-2.02219172532073,
38.8176851083325));
#22582=CARTESIAN_POINT('Ctrl Pts',(-2.51806045907684,-2.01138781723053,
38.8168123292109));
#22583=CARTESIAN_POINT('Ctrl Pts',(-2.53104110274388,-1.99499331763225,
38.815501998755));
#22584=CARTESIAN_POINT('Ctrl Pts',(-2.53540524587758,-1.989444053651,38.8150608835902));
#22585=CARTESIAN_POINT('Ctrl Pts',(-2.54318719471073,-1.97948165202396,
38.814273337805));
#22586=CARTESIAN_POINT('Ctrl Pts',(-2.54661178932123,-1.9750739515477,38.8139264279438));
#22587=CARTESIAN_POINT('Ctrl Pts',(-2.55401143125022,-1.9654988355663,38.8131761265784));
#22588=CARTESIAN_POINT('Ctrl Pts',(-2.55798224376486,-1.9603282648401,38.8127730342564));
#22589=CARTESIAN_POINT('Ctrl Pts',(-2.56905412833189,-1.94582015119312,
38.8116476693855));
#22590=CARTESIAN_POINT('Ctrl Pts',(-2.57612003334254,-1.93645572083592,
38.8109278351649));
#22591=CARTESIAN_POINT('Ctrl Pts',(-2.6173852565759,-1.88114139013536,38.8067128592521));
#22592=CARTESIAN_POINT('Ctrl Pts',(-2.65040812344926,-1.83432173516558,
38.8032944000121));
#22593=CARTESIAN_POINT('Ctrl Pts',(-2.82260901710396,-1.57580811490179,
38.7850672734058));
#22594=CARTESIAN_POINT('Ctrl Pts',(-2.93771459729681,-1.34913028081267,
38.771318407596));
#22595=CARTESIAN_POINT('Ctrl Pts',(-3.08144711727346,-0.957870180989853,
38.7477716487388));
#22596=CARTESIAN_POINT('Ctrl Pts',(-3.12604745984707,-0.800405221279804,
38.7383519913786));
#22597=CARTESIAN_POINT('Ctrl Pts',(-3.16286278519733,-0.618786061352153,
38.7272059279998));
#22598=CARTESIAN_POINT('Ctrl Pts',(-3.16699464761004,-0.597278874106064,
38.7258819480685));
#22599=CARTESIAN_POINT('Ctrl Pts',(-3.17324614501426,-0.562848047624855,
38.723755195981));
#22600=CARTESIAN_POINT('Ctrl Pts',(-3.17550680959566,-0.549950466707746,
38.7229569221296));
#22601=CARTESIAN_POINT('Ctrl Pts',(-3.17936886221839,-0.527098518780338,
38.7215395575294));
#22602=CARTESIAN_POINT('Ctrl Pts',(-3.18100226506128,-0.517149684859452,
38.7209214953921));
#22603=CARTESIAN_POINT('Ctrl Pts',(-3.18429701960772,-0.496475424153949,
38.7196349866772));
#22604=CARTESIAN_POINT('Ctrl Pts',(-3.18595092605086,-0.485748955792172,
38.718966311672));
#22605=CARTESIAN_POINT('Ctrl Pts',(-3.19008337726808,-0.458018436020884,
38.7172344485463));
#22606=CARTESIAN_POINT('Ctrl Pts',(-3.19248013724707,-0.441002717117454,
38.7161686790451));
#22607=CARTESIAN_POINT('Ctrl Pts',(-3.20212950782503,-0.368291638137228,
38.7116007895461));
#22608=CARTESIAN_POINT('Ctrl Pts',(-3.20806119123702,-0.312433782447478,
38.708057231879));
#22609=CARTESIAN_POINT('Ctrl Pts',(-3.21985750140243,-0.164663528791871,
38.6985861807442));
#22610=CARTESIAN_POINT('Ctrl Pts',(-3.22324705391988,-0.0726106288567802,
38.6925867825136));
#22611=CARTESIAN_POINT('Ctrl Pts',(-3.22123667371041,0.260413000722466,
38.6705540577715));
#22612=CARTESIAN_POINT('Ctrl Pts',(-3.19276414240804,0.500422874191539,
38.6539855881292));
#22613=CARTESIAN_POINT('Ctrl Pts',(-3.11648348568949,0.826072993055285,
38.6317213447037));
#22614=CARTESIAN_POINT('Ctrl Pts',(-3.0911949938636,0.916178464593166,38.6255953149802));
#22615=CARTESIAN_POINT('Ctrl Pts',(-3.05765950143477,1.01834737921826,38.6187836760114));
#22616=CARTESIAN_POINT('Ctrl Pts',(-3.05321304665781,1.03160221008797,38.6179026440848));
#22617=CARTESIAN_POINT('Ctrl Pts',(-3.04638266787942,1.05153242107241,38.6165823904263));
#22618=CARTESIAN_POINT('Ctrl Pts',(-3.04406281571226,1.05822935510263,38.6161395259339));
#22619=CARTESIAN_POINT('Ctrl Pts',(-3.03987575713399,1.07018882576067,38.6153500937918));
#22620=CARTESIAN_POINT('Ctrl Pts',(-3.03801695461214,1.07545419552328,38.6150030371192));
#22621=CARTESIAN_POINT('Ctrl Pts',(-3.03396502082593,1.08683763895693,38.6142538227467));
#22622=CARTESIAN_POINT('Ctrl Pts',(-3.03176707161883,1.0929538994206,38.6138519566616));
#22623=CARTESIAN_POINT('Ctrl Pts',(-3.02558158421137,1.11000409406797,38.6127334781502));
#22624=CARTESIAN_POINT('Ctrl Pts',(-3.02155325032854,1.12092326973296,38.6120192560698));
#22625=CARTESIAN_POINT('Ctrl Pts',(-2.99788974749306,1.1840108399259,38.6079033788696));
#22626=CARTESIAN_POINT('Ctrl Pts',(-2.9769615901331,1.23568813515905,38.6045742601978));
#22627=CARTESIAN_POINT('Ctrl Pts',(-2.85309831341355,1.52009835128221,38.586352211355));
#22628=CARTESIAN_POINT('Ctrl Pts',(-2.72421241054394,1.74056406550934,38.5725443297351));
#22629=CARTESIAN_POINT('Ctrl Pts',(-2.47181419243833,2.0744027604447,38.5489055120823));
#22630=CARTESIAN_POINT('Ctrl Pts',(-2.36308328025146,2.1974619822985,38.5394557028752));
#22631=CARTESIAN_POINT('Ctrl Pts',(-2.22975330802823,2.32697182181145,38.5282759105367));
#22632=CARTESIAN_POINT('Ctrl Pts',(-2.2138810619597,2.34207777013135,38.5269512683837));
#22633=CARTESIAN_POINT('Ctrl Pts',(-2.18827719496378,2.36595266754435,38.5248236519738));
#22634=CARTESIAN_POINT('Ctrl Pts',(-2.17864383419666,2.37482633950933,38.524025181835));
#22635=CARTESIAN_POINT('Ctrl Pts',(-2.16149936665313,2.39042667936403,38.5226075882277));
#22636=CARTESIAN_POINT('Ctrl Pts',(-2.15401023828681,2.39717732158954,38.5219894944578));
#22637=CARTESIAN_POINT('Ctrl Pts',(-2.138395039001,2.41112048299922,38.5207030390866));
#22638=CARTESIAN_POINT('Ctrl Pts',(-2.13026408108945,2.41830731433588,38.5200344496495));
#22639=CARTESIAN_POINT('Ctrl Pts',(-2.10916928992794,2.43676374150166,38.5183030643864));
#22640=CARTESIAN_POINT('Ctrl Pts',(-2.09615150339521,2.44797089073208,38.5172376899081));
#22641=CARTESIAN_POINT('Ctrl Pts',(-2.04023271260731,2.49533887939783,38.5126738089208));
#22642=CARTESIAN_POINT('Ctrl Pts',(-1.99648305983983,2.53047829429274,38.5091339553454));
#22643=CARTESIAN_POINT('Ctrl Pts',(-1.87867403214216,2.62014426252652,38.4996753229585));
#22644=CARTESIAN_POINT('Ctrl Pts',(-1.80316375613681,2.67267095264063,38.4936848739923));
#22645=CARTESIAN_POINT('Ctrl Pts',(-1.52761556632957,2.8473518822491,38.4721019313201));
#22646=CARTESIAN_POINT('Ctrl Pts',(-1.31664350570897,2.9508401911888,38.4560101564839));
#22647=CARTESIAN_POINT('Ctrl Pts',(-1.07787440617152,3.03721739410839,38.4390702099217));
#22648=CARTESIAN_POINT('Ctrl Pts',(-1.05935822808816,3.04372516868267,38.4377649089865));
#22649=CARTESIAN_POINT('Ctrl Pts',(-0.963686946120721,3.07637140395294,
38.4310671036862));
#22650=CARTESIAN_POINT('Ctrl Pts',(-0.885613101174097,3.09974925806941,
38.425755924003));
#22651=CARTESIAN_POINT('Ctrl Pts',(-0.793629191734922,3.12353219665299,
38.4197408189209));
#22652=CARTESIAN_POINT('Ctrl Pts',(-0.780506543574181,3.1268370965065,38.4188883785942));
#22653=CARTESIAN_POINT('Ctrl Pts',(-0.760573147020587,3.13172395437175,
38.4176025381763));
#22654=CARTESIAN_POINT('Ctrl Pts',(-0.753777619485011,3.1333665187637,38.4171657655021));
#22655=CARTESIAN_POINT('Ctrl Pts',(-0.741551397257901,3.13627967390906,
38.4163828579099));
#22656=CARTESIAN_POINT('Ctrl Pts',(-0.736122729708663,3.13755828567696,
38.416036268118));
#22657=CARTESIAN_POINT('Ctrl Pts',(-0.724289912588004,3.14031286251561,
38.4152830693479));
#22658=CARTESIAN_POINT('Ctrl Pts',(-0.717884579000465,3.14178332878175,
38.4148767790806));
#22659=CARTESIAN_POINT('Ctrl Pts',(-0.699797048209316,3.14587746244971,
38.4137334066453));
#22660=CARTESIAN_POINT('Ctrl Pts',(-0.68810451888155,3.148455668894,38.4129988902638));
#22661=CARTESIAN_POINT('Ctrl Pts',(-0.616210696039781,3.16388864193324,
38.4085093110128));
#22662=CARTESIAN_POINT('Ctrl Pts',(-0.555661266310293,3.17508246562517,
38.4048430562699));
#22663=CARTESIAN_POINT('Ctrl Pts',(-0.231564557482987,3.22544170965631,
38.3856500249424));
#22664=CARTESIAN_POINT('Ctrl Pts',(0.0357720105488799,3.23354991255757,
38.3712487592086));
#22665=CARTESIAN_POINT('Ctrl Pts',(0.335747515699205,3.20540226999132,38.3541485629435));
#22666=CARTESIAN_POINT('Ctrl Pts',(0.3703611802829,3.20158751495943,38.3521625935107));
#22667=CARTESIAN_POINT('Ctrl Pts',(0.517728638621303,3.18292441129463,38.3436376088817));
#22668=CARTESIAN_POINT('Ctrl Pts',(0.629705377457992,3.16267572173402,38.3369814075794));
#22669=CARTESIAN_POINT('Ctrl Pts',(0.760147728569706,3.13188536583983,38.3289090070795));
#22670=CARTESIAN_POINT('Ctrl Pts',(0.779880466194814,3.12703005156854,38.3276792463039));
#22671=CARTESIAN_POINT('Ctrl Pts',(0.811930615872333,3.11882175811995,38.3256672537962));
#22672=CARTESIAN_POINT('Ctrl Pts',(0.8242765408059,3.11558159270845,38.3248886756023));
#22673=CARTESIAN_POINT('Ctrl Pts',(0.846267045892457,3.10967036787665,38.3234954075626));
#22674=CARTESIAN_POINT('Ctrl Pts',(0.855919097407876,3.10702755136079,38.3228816435759));
#22675=CARTESIAN_POINT('Ctrl Pts',(0.876273680228241,3.10135224355523,38.3215825293356));
#22676=CARTESIAN_POINT('Ctrl Pts',(0.886973113623122,3.09830921504044,38.3208968418547));
#22677=CARTESIAN_POINT('Ctrl Pts',(0.91533454125471,3.09008398580277,38.3190716989328));
#22678=CARTESIAN_POINT('Ctrl Pts',(0.93296805959005,3.08480581866096,38.3179291149274));
#22679=CARTESIAN_POINT('Ctrl Pts',(1.01495437683612,3.05949793555752,38.3125794965939));
#22680=CARTESIAN_POINT('Ctrl Pts',(1.07870993518799,3.03760494134279,38.3083115877426));
#22681=CARTESIAN_POINT('Ctrl Pts',(1.39514060098899,2.91772761919292,38.2865662059791));
#22682=CARTESIAN_POINT('Ctrl Pts',(1.63540086326412,2.79015561371561,38.2680929982626));
#22683=CARTESIAN_POINT('Ctrl Pts',(1.97184742513313,2.55298693769739,38.2403534573455));
#22684=CARTESIAN_POINT('Ctrl Pts',(2.08145687877717,2.46444139251656,38.2309847786213));
#22685=CARTESIAN_POINT('Ctrl Pts',(2.19596849412832,2.3588270784302,38.2211071425949));
#22686=CARTESIAN_POINT('Ctrl Pts',(2.20692998150898,2.34857465080232,38.2201607054759));
#22687=CARTESIAN_POINT('Ctrl Pts',(2.22304158683202,2.33329283752219,38.2187687794706));
#22688=CARTESIAN_POINT('Ctrl Pts',(2.22824693498608,2.32832234914491,38.2183189473264));
#22689=CARTESIAN_POINT('Ctrl Pts',(2.23746815948907,2.31945792934599,38.2175219186344));
#22690=CARTESIAN_POINT('Ctrl Pts',(2.2414905861456,2.31557094571986,38.2171741941864));
#22691=CARTESIAN_POINT('Ctrl Pts',(2.25011066063178,2.30719761638016,38.216428927465));
#22692=CARTESIAN_POINT('Ctrl Pts',(2.25470500877019,2.30270800390525,38.2160316481237));
#22693=CARTESIAN_POINT('Ctrl Pts',(2.26679697293695,2.29082080974838,38.21498576637));
#22694=CARTESIAN_POINT('Ctrl Pts',(2.27427187445572,2.28340008476939,38.2143389530659));
#22695=CARTESIAN_POINT('Ctrl Pts',(2.31247691316823,2.24509822751942,38.2110307115671));
#22696=CARTESIAN_POINT('Ctrl Pts',(2.3426166156365,2.21363125917362,38.2084131276354));
#22697=CARTESIAN_POINT('Ctrl Pts',(2.4292636926111,2.11941594719959,38.2008298884893));
#22698=CARTESIAN_POINT('Ctrl Pts',(2.48395675346763,2.05504426523028,38.1959669696715));
#22699=CARTESIAN_POINT('Ctrl Pts',(2.60289988764278,1.903355644638,38.1850190688539));
#22700=CARTESIAN_POINT('Ctrl Pts',(2.66539994914537,1.81479888962503,38.178983303926));
#22701=CARTESIAN_POINT('Ctrl Pts',(2.84071569230094,1.53774190101823,38.1606620164246));
#22702=CARTESIAN_POINT('Ctrl Pts',(2.9388299190723,1.34073820988874,38.1483289833366));
#22703=CARTESIAN_POINT('Ctrl Pts',(3.0291607124404,1.10075680698274,38.1330463134295));
#22704=CARTESIAN_POINT('Ctrl Pts',(3.04156958776108,1.06598988876505,38.1308277508842));
#22705=CARTESIAN_POINT('Ctrl Pts',(3.0582051806485,1.01672331008451,38.1276743916881));
#22706=CARTESIAN_POINT('Ctrl Pts',(3.06293166416047,1.00239454547579,38.1267561460961));
#22707=CARTESIAN_POINT('Ctrl Pts',(3.0704282109749,0.979119938544014,38.1252625989505));
#22708=CARTESIAN_POINT('Ctrl Pts',(3.0732602415944,0.970194175053682,38.1246893490493));
#22709=CARTESIAN_POINT('Ctrl Pts',(3.07909211170209,0.951531989013385,38.1234897319037));
#22710=CARTESIAN_POINT('Ctrl Pts',(3.08208475926499,0.941793444106166,38.1228631356315));
#22711=CARTESIAN_POINT('Ctrl Pts',(3.08906898686195,0.918675833820232,38.1213742172039));
#22712=CARTESIAN_POINT('Ctrl Pts',(3.09301987527039,0.905284780912984,38.1205105721028));
#22713=CARTESIAN_POINT('Ctrl Pts',(3.10116125281201,0.877015036798432,38.1186847087445));
#22714=CARTESIAN_POINT('Ctrl Pts',(3.10533194928208,0.862131058501892,38.1177218675539));
#22715=CARTESIAN_POINT('Ctrl Pts',(3.11640311428866,0.821498500236896,38.1150889848471));
#22716=CARTESIAN_POINT('Ctrl Pts',(3.12309132359014,0.795693830806746,38.1134121383776));
#22717=CARTESIAN_POINT('Ctrl Pts',(3.19166642247518,0.516919861529357,38.0952424557336));
#22718=CARTESIAN_POINT('Ctrl Pts',(3.22297737174026,0.257477409621273,38.0777345230348));
#22719=CARTESIAN_POINT('Ctrl Pts',(3.22274875711747,-0.00283037061280869,
38.0601149330464));
#22720=CARTESIAN_POINT('Ctrl Pts',(-1.47642198135613,-2.86757701803244,
37.6538374877124));
#22721=CARTESIAN_POINT('Ctrl Pts',(-0.665155103199407,-3.27567489814633,
37.7100277565976));
#22722=CARTESIAN_POINT('Ctrl Pts',(1.50747120958243,-3.40811199926236,37.8325290049372));
#22723=CARTESIAN_POINT('Ctrl Pts',(3.10959334693804,-1.49896815034561,37.9681743254574));
#22724=CARTESIAN_POINT('Ctrl Pts',(3.22586433700409,-0.215544722264628,
38.0476293770925));
#22725=CARTESIAN_POINT('Ctrl Pts',(3.22389497588569,-0.002876326465697,
38.0607734492731));
#22726=CARTESIAN_POINT('',(3.22274953375635,0.00173354353987881,37.8165056021994));
#22727=CARTESIAN_POINT('Ctrl Pts',(-1.47525540431025,-2.86526422072265,
37.4085260041042));
#22728=CARTESIAN_POINT('Ctrl Pts',(-1.43625760423782,-2.88534324690704,
37.4114783217196));
#22729=CARTESIAN_POINT('Ctrl Pts',(-1.39683575020098,-2.90463337997842,
37.4144193805815));
#22730=CARTESIAN_POINT('Ctrl Pts',(-1.27393816816533,-2.96168666266681,
37.4234325092417));
#22731=CARTESIAN_POINT('Ctrl Pts',(-1.1892482247323,-2.9966979124969,37.429427020127));
#22732=CARTESIAN_POINT('Ctrl Pts',(-1.09009691860782,-3.03282046492186,
37.4361111154649));
#22733=CARTESIAN_POINT('Ctrl Pts',(-1.0769890306239,-3.03749994383052,37.4369881523242));
#22734=CARTESIAN_POINT('Ctrl Pts',(-1.05717493303045,-3.04442913262363,
37.4383035141713));
#22735=CARTESIAN_POINT('Ctrl Pts',(-1.05049115905415,-3.04674185148841,
37.4387454441221));
#22736=CARTESIAN_POINT('Ctrl Pts',(-1.03851967456026,-3.05084014569193,
37.4395337580483));
#22737=CARTESIAN_POINT('Ctrl Pts',(-1.03323490810244,-3.05263399955876,
37.4398806263606));
#22738=CARTESIAN_POINT('Ctrl Pts',(-1.02177956153736,-3.05648923004023,
37.4406300496742));
#22739=CARTESIAN_POINT('Ctrl Pts',(-1.01560741011654,-3.0585456472008,37.4410323099559));
#22740=CARTESIAN_POINT('Ctrl Pts',(-0.998341982499454,-3.06424005945056,
37.4421533973977));
#22741=CARTESIAN_POINT('Ctrl Pts',(-0.987234969882515,-3.0678365308348,
37.4428698150333));
#22742=CARTESIAN_POINT('Ctrl Pts',(-0.92237377082824,-3.08844997402597,
37.4470269220475));
#22743=CARTESIAN_POINT('Ctrl Pts',(-0.868196327896372,-3.10411543744507,
37.4503933551825));
#22744=CARTESIAN_POINT('Ctrl Pts',(-0.567968942834488,-3.18244995353801,
37.4686115598272));
#22745=CARTESIAN_POINT('Ctrl Pts',(-0.315569757793848,-3.21730000377383,
37.4823896948693));
#22746=CARTESIAN_POINT('Ctrl Pts',(0.102172048858668,-3.22529598914287,
37.505990032542));
#22747=CARTESIAN_POINT('Ctrl Pts',(0.265998739668756,-3.21593028080837,
37.5154334030571));
#22748=CARTESIAN_POINT('Ctrl Pts',(0.450099879470417,-3.19123917122849,
37.5266056965123));
#22749=CARTESIAN_POINT('Ctrl Pts',(0.47177886739132,-3.18810633660193,37.5279298974547));
#22750=CARTESIAN_POINT('Ctrl Pts',(0.506362463765492,-3.1827481905488,37.530056797019));
#22751=CARTESIAN_POINT('Ctrl Pts',(0.519288604395263,-3.18066476173729,
37.5308549945278));
#22752=CARTESIAN_POINT('Ctrl Pts',(0.542142228265927,-3.17683820086012,
37.5322720981139));
#22753=CARTESIAN_POINT('Ctrl Pts',(0.552074959888118,-3.17512714471595,
37.5328899751805));
#22754=CARTESIAN_POINT('Ctrl Pts',(0.572681199104011,-3.17147780788289,
37.534175972722));
#22755=CARTESIAN_POINT('Ctrl Pts',(0.58335325957357,-3.16953217551716,37.5348443208466));
#22756=CARTESIAN_POINT('Ctrl Pts',(0.610891962848549,-3.16436777485636,
37.5365750642616));
#22757=CARTESIAN_POINT('Ctrl Pts',(0.627742901766128,-3.16106805300211,
37.5376400362361));
#22758=CARTESIAN_POINT('Ctrl Pts',(0.699516743483176,-3.14641689040722,
37.5422019819395));
#22759=CARTESIAN_POINT('Ctrl Pts',(0.754161905297265,-3.1337680363353,37.5457402667464));
#22760=CARTESIAN_POINT('Ctrl Pts',(0.897409856562916,-3.09664642239335,
37.555194229315));
#22761=CARTESIAN_POINT('Ctrl Pts',(0.98533890770676,-3.06979937999765,37.5611815026519));
#22762=CARTESIAN_POINT('Ctrl Pts',(1.2095339777098,-2.99072159863251,37.5769081150617));
#22763=CARTESIAN_POINT('Ctrl Pts',(1.34361342306006,-2.93293127891763,37.5867751799219));
#22764=CARTESIAN_POINT('Ctrl Pts',(1.64055446299926,-2.78029852200403,37.6093749174947));
#22765=CARTESIAN_POINT('Ctrl Pts',(1.79997494065692,-2.67984805879226,37.6220741106077));
#22766=CARTESIAN_POINT('Ctrl Pts',(1.9613994561847,-2.55719460177184,37.6349237909817));
#22767=CARTESIAN_POINT('Ctrl Pts',(1.97300052435852,-2.54825450221348,37.6358470784723));
#22768=CARTESIAN_POINT('Ctrl Pts',(1.99015393674327,-2.53484824568232,37.6372114851217));
#22769=CARTESIAN_POINT('Ctrl Pts',(1.99575287536791,-2.53044240862144,37.637656708983));
#22770=CARTESIAN_POINT('Ctrl Pts',(2.00571489348871,-2.5225496074878,37.6384485903369));
#22771=CARTESIAN_POINT('Ctrl Pts',(2.01008355105668,-2.51906984333524,37.6387957505675));
#22772=CARTESIAN_POINT('Ctrl Pts',(2.01446052691476,-2.51556481699289,37.6391434612459));
#22773=CARTESIAN_POINT('Ctrl Pts',(2.01447780796669,-2.51555097825504,37.6391448340657));
#22774=CARTESIAN_POINT('Ctrl Pts',(2.01451209387071,-2.51552352138144,37.6391475577606));
#22775=CARTESIAN_POINT('Ctrl Pts',(2.01452909869127,-2.5155099032802,37.6391489086332));
#22776=CARTESIAN_POINT('Ctrl Pts',(2.0145628373658,-2.51548288351646,37.6391515888495));
#22777=CARTESIAN_POINT('Ctrl Pts',(2.01457957132563,-2.51546948177812,37.6391529182017));
#22778=CARTESIAN_POINT('Ctrl Pts',(2.01461277389525,-2.51544289026868,37.6391555558235));
#22779=CARTESIAN_POINT('Ctrl Pts',(2.01462924241462,-2.51542970057863,37.639156864086));
#22780=CARTESIAN_POINT('Ctrl Pts',(2.0146619193043,-2.51540352902598,37.6391594599418));
#22781=CARTESIAN_POINT('Ctrl Pts',(2.01467812761216,-2.51539054722172,37.6391607475302));
#22782=CARTESIAN_POINT('Ctrl Pts',(2.01471028907978,-2.51536478746003,37.6391633024351));
#22783=CARTESIAN_POINT('Ctrl Pts',(2.01472624225204,-2.51535200950061,37.6391645697527));
#22784=CARTESIAN_POINT('Ctrl Pts',(2.01972807099056,-2.51134563322859,37.6395619138407));
#22785=CARTESIAN_POINT('Ctrl Pts',(2.02470211271556,-2.50733717850673,37.6399569153863));
#22786=CARTESIAN_POINT('Ctrl Pts',(2.03827249452963,-2.49633443583687,37.6410343068212));
#22787=CARTESIAN_POINT('Ctrl Pts',(2.04684482313504,-2.48931047799182,37.6417145931564));
#22788=CARTESIAN_POINT('Ctrl Pts',(2.06606395237776,-2.47339638665036,37.6432395665484));
#22789=CARTESIAN_POINT('Ctrl Pts',(2.07669000471623,-2.4644814019076,37.6440825502383));
#22790=CARTESIAN_POINT('Ctrl Pts',(2.10951810837679,-2.43657637541224,37.6466875629647));
#22791=CARTESIAN_POINT('Ctrl Pts',(2.13152033616147,-2.41735232524608,37.6484345170127));
#22792=CARTESIAN_POINT('Ctrl Pts',(2.21662868366218,-2.34092479432583,37.6552100180404));
#22793=CARTESIAN_POINT('Ctrl Pts',(2.277722411028,-2.28152455949615,37.6601136487935));
#22794=CARTESIAN_POINT('Ctrl Pts',(2.47910493352838,-2.06956152673026,37.6767133184336));
#22795=CARTESIAN_POINT('Ctrl Pts',(2.60699792545665,-1.90594121404209,37.6880679711775));
#22796=CARTESIAN_POINT('Ctrl Pts',(2.79364918059233,-1.61285988383586,37.7078258502478));
#22797=CARTESIAN_POINT('Ctrl Pts',(2.86118440054439,-1.48976823541654,37.7159683100511));
#22798=CARTESIAN_POINT('Ctrl Pts',(2.92950456987935,-1.3433449777783,37.7256914787533));
#22799=CARTESIAN_POINT('Ctrl Pts',(2.93833337958235,-1.32392207894861,37.7269817553788));
#22800=CARTESIAN_POINT('Ctrl Pts',(2.95220046439086,-1.29259315699834,37.7290644168006));
#22801=CARTESIAN_POINT('Ctrl Pts',(2.9573611778658,-1.28074178017141,37.7298525949595));
#22802=CARTESIAN_POINT('Ctrl Pts',(2.96640875182672,-1.25961809982176,37.7312581549325));
#22803=CARTESIAN_POINT('Ctrl Pts',(2.97032380494049,-1.25035800092514,37.7318745637));
#22804=CARTESIAN_POINT('Ctrl Pts',(2.97840216178564,-1.23099855951164,37.7331638276924));
#22805=CARTESIAN_POINT('Ctrl Pts',(2.98255756835005,-1.22089607977979,37.7338369421164));
#22806=CARTESIAN_POINT('Ctrl Pts',(2.99324152136314,-1.19454154661972,37.7355938605544));
#22807=CARTESIAN_POINT('Ctrl Pts',(2.9996890194264,-1.17825722107829,37.7366803906561));
#22808=CARTESIAN_POINT('Ctrl Pts',(3.02738045597171,-1.10661678915694,37.7414651034141));
#22809=CARTESIAN_POINT('Ctrl Pts',(3.04722600175411,-1.05073597301318,37.745209778755));
#22810=CARTESIAN_POINT('Ctrl Pts',(3.09618601212435,-0.899794217254751,
37.7553646995311));
#22811=CARTESIAN_POINT('Ctrl Pts',(3.12246079401988,-0.803886135467158,
37.7618604483947));
#22812=CARTESIAN_POINT('Ctrl Pts',(3.19655906508416,-0.474311713053508,
37.7842838470966));
#22813=CARTESIAN_POINT('Ctrl Pts',(3.22287775861272,-0.236643276283802,
37.8006859445876));
#22814=CARTESIAN_POINT('Ctrl Pts',(3.22274953375635,0.00173354353987881,
37.8165056021994));
#22815=CARTESIAN_POINT('Ctrl Pts',(3.222749531205,0.00173828016955539,37.8165059165414));
#22816=CARTESIAN_POINT('Ctrl Pts',(3.22270305071438,0.0879125241068303,
37.8222247873387));
#22817=CARTESIAN_POINT('Ctrl Pts',(3.21920019789002,0.174060452734954,37.8278510718186));
#22818=CARTESIAN_POINT('Ctrl Pts',(3.2114797988416,0.269454144514142,37.8339081349421));
#22819=CARTESIAN_POINT('Ctrl Pts',(3.21067053001022,0.278931510071132,37.8345079924864));
#22820=CARTESIAN_POINT('Ctrl Pts',(3.2092464328258,0.294781062059853,37.8355078136478));
#22821=CARTESIAN_POINT('Ctrl Pts',(3.20865456251314,0.301155178058178,37.835908996707));
#22822=CARTESIAN_POINT('Ctrl Pts',(3.20754096814088,0.312771891365883,37.8366384362922));
#22823=CARTESIAN_POINT('Ctrl Pts',(3.2070253751692,0.318015034703768,37.836967029785));
#22824=CARTESIAN_POINT('Ctrl Pts',(3.20593683907471,0.328812599313765,37.8376423829336));
#22825=CARTESIAN_POINT('Ctrl Pts',(3.20536232519363,0.334366724584944,37.8379890372753));
#22826=CARTESIAN_POINT('Ctrl Pts',(3.20402360875131,0.346988193085497,37.8387751375784));
#22827=CARTESIAN_POINT('Ctrl Pts',(3.20325045895787,0.354054502934622,37.8392140737816));
#22828=CARTESIAN_POINT('Ctrl Pts',(3.20118373404302,0.372382545982474,37.8403496410081));
#22829=CARTESIAN_POINT('Ctrl Pts',(3.19985409722441,0.383640228532662,37.8410442892656));
#22830=CARTESIAN_POINT('Ctrl Pts',(3.19108503739539,0.454666263385874,37.8454102006503));
#22831=CARTESIAN_POINT('Ctrl Pts',(3.1820302095878,0.514227520546008,37.8489966822654));
#22832=CARTESIAN_POINT('Ctrl Pts',(3.16366679900411,0.615771813209107,37.8550362213012));
#22833=CARTESIAN_POINT('Ctrl Pts',(3.1551785212053,0.657883962557299,37.8575185671406));
#22834=CARTESIAN_POINT('Ctrl Pts',(3.09705571057058,0.919161018413947,37.8728485623131));
#22835=CARTESIAN_POINT('Ctrl Pts',(3.02545318345635,1.13280770928991,37.8851126266627));
#22836=CARTESIAN_POINT('Ctrl Pts',(2.89150874849534,1.42650354757404,37.9034389615986));
#22837=CARTESIAN_POINT('Ctrl Pts',(2.84676610907895,1.51382154709284,37.9090837800931));
#22838=CARTESIAN_POINT('Ctrl Pts',(2.76897445235689,1.64995383043231,37.9183162286303));
#22839=CARTESIAN_POINT('Ctrl Pts',(2.73844702740723,1.70013951790317,37.9218187002717));
#22840=CARTESIAN_POINT('Ctrl Pts',(2.69709104329107,1.76412079276401,37.9264275422393));
#22841=CARTESIAN_POINT('Ctrl Pts',(2.68749641232533,1.7787032586588,37.927487903642));
#22842=CARTESIAN_POINT('Ctrl Pts',(2.67171291233598,1.80227265496957,37.9292182942922));
#22843=CARTESIAN_POINT('Ctrl Pts',(2.66559595145052,1.81130749122718,37.9298856027177));
#22844=CARTESIAN_POINT('Ctrl Pts',(2.65375232712182,1.82861075903095,37.9311714103812));
#22845=CARTESIAN_POINT('Ctrl Pts',(2.64803259611736,1.83688379817252,37.9317896403862));
#22846=CARTESIAN_POINT('Ctrl Pts',(2.63485785912359,1.85575036666307,37.9332075188928));
#22847=CARTESIAN_POINT('Ctrl Pts',(2.62737755804495,1.86632594172695,37.9340081330577));
#22848=CARTESIAN_POINT('Ctrl Pts',(2.60735435208714,1.89427559330572,37.9361397271336));
#22849=CARTESIAN_POINT('Ctrl Pts',(2.59470173952829,1.91156992752261,37.9374749398502));
#22850=CARTESIAN_POINT('Ctrl Pts',(2.49592050226965,2.04380213864549,37.9478116764587));
#22851=CARTESIAN_POINT('Ctrl Pts',(2.402379485937,2.15297679446978,37.9571075650017));
#22852=CARTESIAN_POINT('Ctrl Pts',(2.15626158547292,2.40415153159436,37.9804243513077));
#22853=CARTESIAN_POINT('Ctrl Pts',(1.99659451213777,2.53830831002931,37.9946613115335));
#22854=CARTESIAN_POINT('Ctrl Pts',(1.75751803682042,2.70258726230109,38.0141158726067));
#22855=CARTESIAN_POINT('Ctrl Pts',(1.68815084006837,2.74645156053097,38.0195611130074));
#22856=CARTESIAN_POINT('Ctrl Pts',(1.59252827816446,2.80192496797036,38.0267347183051));
#22857=CARTESIAN_POINT('Ctrl Pts',(1.56768624761195,2.81589946415481,38.0285691710128));
#22858=CARTESIAN_POINT('Ctrl Pts',(1.53069724318931,2.8360657951724,38.0312541993667));
#22859=CARTESIAN_POINT('Ctrl Pts',(1.51869179277238,2.84251270853795,38.0321185477782));
#22860=CARTESIAN_POINT('Ctrl Pts',(1.49690928938378,2.85403248933598,38.0336734742623));
#22861=CARTESIAN_POINT('Ctrl Pts',(1.48714650299652,2.85913171395537,38.0343655820304));
#22862=CARTESIAN_POINT('Ctrl Pts',(1.47173453145196,2.86708127940143,38.0354504067361));
#22863=CARTESIAN_POINT('Ctrl Pts',(1.46610287509791,2.86996514874785,38.0358451866311));
#22864=CARTESIAN_POINT('Ctrl Pts',(1.46044796055885,2.87283993937586,38.0362399436139));
#22865=CARTESIAN_POINT('Ctrl Pts',(1.46043321592104,2.87284743496903,38.0362409728929));
#22866=CARTESIAN_POINT('Ctrl Pts',(1.46040364232788,2.87286246873257,38.0362430373144));
#22867=CARTESIAN_POINT('Ctrl Pts',(1.46038881341484,2.8728700068798,38.0362440724538));
#22868=CARTESIAN_POINT('Ctrl Pts',(1.46035907063203,2.87288512607146,38.0362461486401));
#22869=CARTESIAN_POINT('Ctrl Pts',(1.46034415683728,2.87289270707611,38.0362471896817));
#22870=CARTESIAN_POINT('Ctrl Pts',(1.45534669962921,2.87543297376482,38.0365960280181));
#22871=CARTESIAN_POINT('Ctrl Pts',(1.45035764638453,2.87795265786701,38.0369429881896));
#22872=CARTESIAN_POINT('Ctrl Pts',(1.43895354559918,2.88367502743833,38.0377331616025));
#22873=CARTESIAN_POINT('Ctrl Pts',(1.43253436100289,2.88686928646823,38.0381758437417));
#22874=CARTESIAN_POINT('Ctrl Pts',(1.41276385848193,2.89662513128069,38.0395330002227));
#22875=CARTESIAN_POINT('Ctrl Pts',(1.39937750172517,2.90311582586225,38.0404431584222));
#22876=CARTESIAN_POINT('Ctrl Pts',(1.22848058267346,2.9845225447519,38.0519576953124));
#22877=CARTESIAN_POINT('Ctrl Pts',(1.06516083522188,3.04663577192103,38.0618390428793));
#22878=CARTESIAN_POINT('Ctrl Pts',(0.744803845263201,3.1395370959834,38.0805367676056));
#22879=CARTESIAN_POINT('Ctrl Pts',(0.588945809178976,3.17247024686073,38.0893474671676));
#22880=CARTESIAN_POINT('Ctrl Pts',(0.340216192523598,3.20605943601172,38.1036365166495));
#22881=CARTESIAN_POINT('Ctrl Pts',(0.24865913799094,3.21445654336918,38.1089413318794));
#22882=CARTESIAN_POINT('Ctrl Pts',(0.100854190929152,3.2216597544652,38.1176673211599));
#22883=CARTESIAN_POINT('Ctrl Pts',(0.0447762865463718,3.22292687623243,
38.1210150249678));
#22884=CARTESIAN_POINT('Ctrl Pts',(-0.0284747961101848,3.22266994879571,
38.1254477024342));
#22885=CARTESIAN_POINT('Ctrl Pts',(-0.0456448777774604,3.22247248867469,
38.1264909926292));
#22886=CARTESIAN_POINT('Ctrl Pts',(-0.0736583032493643,3.22192639537209,
38.1282004306651));
#22887=CARTESIAN_POINT('Ctrl Pts',(-0.0845030560364107,3.22166020427402,
38.1288639815716));
#22888=CARTESIAN_POINT('Ctrl Pts',(-0.105420791035026,3.22104107495384,
38.1301473820261));
#22889=CARTESIAN_POINT('Ctrl Pts',(-0.115493880682363,3.22069562510396,
38.1307669885861));
#22890=CARTESIAN_POINT('Ctrl Pts',(-0.138648031389127,3.21979280534953,
38.1321949203655));
#22891=CARTESIAN_POINT('Ctrl Pts',(-0.151727580797547,3.21920296332524,
38.1330042578807));
#22892=CARTESIAN_POINT('Ctrl Pts',(-0.18667799869667,3.21741334873613,38.1351743386246));
#22893=CARTESIAN_POINT('Ctrl Pts',(-0.208540539936081,3.21607029412703,
38.1365395609543));
#22894=CARTESIAN_POINT('Ctrl Pts',(-0.393840039733015,3.2027896641646,38.1481785828982));
#22895=CARTESIAN_POINT('Ctrl Pts',(-0.556135396528536,3.17862711579753,
38.158839691741));
#22896=CARTESIAN_POINT('Ctrl Pts',(-0.963423532403372,3.08583802170708,
38.1867004993818));
#22897=CARTESIAN_POINT('Ctrl Pts',(-1.20343252256089,3.00038773177432,38.2042259311353));
#22898=CARTESIAN_POINT('Ctrl Pts',(-1.48147084860564,2.86261145545658,38.2245269036309));
#22899=CARTESIAN_POINT('Ctrl Pts',(-1.53135739624207,2.83623794245424,38.2281651429803));
#22900=CARTESIAN_POINT('Ctrl Pts',(-1.59070494386854,2.80283993168146,38.23246559334));
#22901=CARTESIAN_POINT('Ctrl Pts',(-1.60084970609599,2.79705812049337,38.2331996995365));
#22902=CARTESIAN_POINT('Ctrl Pts',(-1.61659788811844,2.78796900257939,38.2343374472128));
#22903=CARTESIAN_POINT('Ctrl Pts',(-1.62222297267421,2.78469971808759,38.234743470836));
#22904=CARTESIAN_POINT('Ctrl Pts',(-1.63265481793771,2.77859442066814,38.2354957100871));
#22905=CARTESIAN_POINT('Ctrl Pts',(-1.6374640662122,2.77576298370083,38.2358422041996));
#22906=CARTESIAN_POINT('Ctrl Pts',(-1.64835086985035,2.76931525549814,38.2366259119493));
#22907=CARTESIAN_POINT('Ctrl Pts',(-1.65442387733516,2.76569145257135,38.2370626284957));
#22908=CARTESIAN_POINT('Ctrl Pts',(-1.67241077076626,2.75487811040467,38.2383548667934));
#22909=CARTESIAN_POINT('Ctrl Pts',(-1.68429025628301,2.74763125949393,38.2392067355982));
#22910=CARTESIAN_POINT('Ctrl Pts',(-1.77405206577623,2.6920728820386,38.2456342994269));
#22911=CARTESIAN_POINT('Ctrl Pts',(-1.84989646459654,2.64053092553442,38.2510129042002));
#22912=CARTESIAN_POINT('Ctrl Pts',(-2.11863128812539,2.44063412914987,38.2702723580079));
#22913=CARTESIAN_POINT('Ctrl Pts',(-2.29675611581672,2.27381134942314,38.2834955770402));
#22914=CARTESIAN_POINT('Ctrl Pts',(-2.51395734354943,2.01855791224649,38.3025768798924));
#22915=CARTESIAN_POINT('Ctrl Pts',(-2.57047107878271,1.94608172400177,38.3078797114441));
#22916=CARTESIAN_POINT('Ctrl Pts',(-2.65636616807812,1.82564513694718,38.3166027355812));
#22917=CARTESIAN_POINT('Ctrl Pts',(-2.68772469930393,1.77915619050023,38.3199495233266));
#22918=CARTESIAN_POINT('Ctrl Pts',(-2.72708003359799,1.71739536630857,38.3243811566818));
#22919=CARTESIAN_POINT('Ctrl Pts',(-2.7361907508879,1.70284247976019,38.3254243437838));
#22920=CARTESIAN_POINT('Ctrl Pts',(-2.7508671015084,1.6789774937446,38.3271336554537));
#22921=CARTESIAN_POINT('Ctrl Pts',(-2.75650284633126,1.66970874354773,38.3277971838302));
#22922=CARTESIAN_POINT('Ctrl Pts',(-2.76728459198546,1.65177333175417,38.3290805706059));
#22923=CARTESIAN_POINT('Ctrl Pts',(-2.77243694752018,1.64311062344441,38.3297001861775));
#22924=CARTESIAN_POINT('Ctrl Pts',(-2.78418905852207,1.62313902526471,38.3311281815928));
#22925=CARTESIAN_POINT('Ctrl Pts',(-2.79076066565264,1.61181385644982,38.3319375740255));
#22926=CARTESIAN_POINT('Ctrl Pts',(-2.80814204631419,1.58143470015158,38.3341078974175));
#22927=CARTESIAN_POINT('Ctrl Pts',(-2.81882671262365,1.56231027297562,38.3354733090496));
#22928=CARTESIAN_POINT('Ctrl Pts',(-2.90785048558914,1.39908054498373,38.3471219503244));
#22929=CARTESIAN_POINT('Ctrl Pts',(-2.97526571064352,1.24931983145554,38.3577932298352));
#22930=CARTESIAN_POINT('Ctrl Pts',(-3.11736683285141,0.856016445185154,
38.3856860239903));
#22931=CARTESIAN_POINT('Ctrl Pts',(-3.17515349537329,0.607565359259412,
38.4032339399794));
#22932=CARTESIAN_POINT('Ctrl Pts',(-3.2093141222477,0.29925852843585,38.4235230123581));
#22933=CARTESIAN_POINT('Ctrl Pts',(-3.2140294884054,0.243450512011036,38.4271333905509));
#22934=CARTESIAN_POINT('Ctrl Pts',(-3.21796642475436,0.175913030632564,
38.4314054360352));
#22935=CARTESIAN_POINT('Ctrl Pts',(-3.2185813674084,0.164278106729677,38.4321379173505));
#22936=CARTESIAN_POINT('Ctrl Pts',(-3.21944109407276,0.14614670904612,38.4332736998765));
#22937=CARTESIAN_POINT('Ctrl Pts',(-3.21972933480573,0.13965253715186,38.4336793702184));
#22938=CARTESIAN_POINT('Ctrl Pts',(-3.22022854344607,0.127580733825581,
38.4344312904788));
#22939=CARTESIAN_POINT('Ctrl Pts',(-3.22044466915152,0.122003480728437,
38.4347778167768));
#22940=CARTESIAN_POINT('Ctrl Pts',(-3.22090206691413,0.109350619653088,
38.4355620247485));
#22941=CARTESIAN_POINT('Ctrl Pts',(-3.22113451361212,0.102274777662503,
38.4359992066737));
#22942=CARTESIAN_POINT('Ctrl Pts',(-3.22175574471678,0.0812533720824494,
38.4372941009502));
#22943=CARTESIAN_POINT('Ctrl Pts',(-3.22207730168362,0.0673057752632883,
38.4381481380415));
#22944=CARTESIAN_POINT('Ctrl Pts',(-3.2238434874023,-0.0393583179198146,
38.4446432329982));
#22945=CARTESIAN_POINT('Ctrl Pts',(-3.22137664547639,-0.132105592091975,
38.450082489086));
#22946=CARTESIAN_POINT('Ctrl Pts',(-3.19805036666433,-0.465958016293262,
38.4693168858473));
#22947=CARTESIAN_POINT('Ctrl Pts',(-3.15406885139023,-0.704631435494986,
38.4824714164184));
#22948=CARTESIAN_POINT('Ctrl Pts',(-3.05706370892876,-1.02417925709542,
38.5014826397379));
#22949=CARTESIAN_POINT('Ctrl Pts',(-3.02658375078057,-1.11102229362385,
38.5067927171475));
#22950=CARTESIAN_POINT('Ctrl Pts',(-2.97159564421363,-1.24855401512394,
38.5155265714249));
#22951=CARTESIAN_POINT('Ctrl Pts',(-2.94940177372226,-1.30011399551361,
38.5188767044753));
#22952=CARTESIAN_POINT('Ctrl Pts',(-2.91867338573031,-1.36665951756177,
38.5233121509282));
#22953=CARTESIAN_POINT('Ctrl Pts',(-2.91134839518326,-1.38219502010771,
38.524355714684));
#22954=CARTESIAN_POINT('Ctrl Pts',(-2.89919456199872,-1.40744667972448,
38.5260654882481));
#22955=CARTESIAN_POINT('Ctrl Pts',(-2.89444015800656,-1.4171984447344,38.5267290991531));
#22956=CARTESIAN_POINT('Ctrl Pts',(-2.88517414570637,-1.43596284469021,
38.5280125364984));
#22957=CARTESIAN_POINT('Ctrl Pts',(-2.88066931434218,-1.44497869884218,
38.5286321195248));
#22958=CARTESIAN_POINT('Ctrl Pts',(-2.87021637655335,-1.46565578401377,
38.5300598836095));
#22959=CARTESIAN_POINT('Ctrl Pts',(-2.86423939276216,-1.47730214183485,
38.5308690761878));
#22960=CARTESIAN_POINT('Ctrl Pts',(-2.84807586046103,-1.50833049362682,
38.5330385159032));
#22961=CARTESIAN_POINT('Ctrl Pts',(-2.83776260141139,-1.52764536616261,
38.5344032379863));
#22962=CARTESIAN_POINT('Ctrl Pts',(-2.74878830991491,-1.69026769387256,
38.5460168899577));
#22963=CARTESIAN_POINT('Ctrl Pts',(-2.65953734574309,-1.82748148231766,
38.5566511793456));
#22964=CARTESIAN_POINT('Ctrl Pts',(-2.40655797962761,-2.15839222672096,
38.5844296518019));
#22965=CARTESIAN_POINT('Ctrl Pts',(-2.22969529378452,-2.34064781176811,
38.6018979557191));
#22966=CARTESIAN_POINT('Ctrl Pts',(-1.98872409105201,-2.53661202819307,
38.6222302776015));
#22967=CARTESIAN_POINT('Ctrl Pts',(-1.9431451261639,-2.57169439898932,38.6259403739221));
#22968=CARTESIAN_POINT('Ctrl Pts',(-1.88715595583454,-2.61245053861243,
38.6303139793726));
#22969=CARTESIAN_POINT('Ctrl Pts',(-1.87762552175141,-2.61930865466757,
38.6310522071538));
#22970=CARTESIAN_POINT('Ctrl Pts',(-1.86274457894569,-2.62989404893614,
38.6321949382655));
#22971=CARTESIAN_POINT('Ctrl Pts',(-1.85741999614261,-2.63365734953099,
38.632601856881));
#22972=CARTESIAN_POINT('Ctrl Pts',(-1.8475178844385,-2.64061098230092,38.6333549080475));
#22973=CARTESIAN_POINT('Ctrl Pts',(-1.84294353429229,-2.64380555701761,
38.6337013244089));
#22974=CARTESIAN_POINT('Ctrl Pts',(-1.83256804051393,-2.65101144490501,
38.6344837827721));
#22975=CARTESIAN_POINT('Ctrl Pts',(-1.82676202617466,-2.65501559432157,
38.6349193343374));
#22976=CARTESIAN_POINT('Ctrl Pts',(-1.8095358930443,-2.66681243362961,38.6362049378037));
#22977=CARTESIAN_POINT('Ctrl Pts',(-1.79807855029821,-2.67455084962485,
38.6370513921887));
#22978=CARTESIAN_POINT('Ctrl Pts',(-1.7124328785458,-2.73159776516563,38.6433177517081));
#22979=CARTESIAN_POINT('Ctrl Pts',(-1.63627114840698,-2.77788994748917,
38.6485515707677));
#22980=CARTESIAN_POINT('Ctrl Pts',(-1.53081351430991,-2.83614391159488,
38.6554881361776));
#22981=CARTESIAN_POINT('Ctrl Pts',(-1.5031349093025,-2.85090973729773,38.6572808675935));
#22982=CARTESIAN_POINT('Ctrl Pts',(-1.47525532932069,-2.86526425933297,
38.6590632205222));
#22983=CARTESIAN_POINT('Origin',(0.,0.,4.68922655072688));
#22984=CARTESIAN_POINT('',(-1.47525550050006,-2.86526417119684,40.1544081509837));
#22985=CARTESIAN_POINT('',(-1.47525529542902,-2.86526427678297,39.904468116039));
#22986=CARTESIAN_POINT('',(-1.47525540501186,-2.86526422036142,4.68922655072688));
#22987=CARTESIAN_POINT('Ctrl Pts',(-1.47525550050006,-2.86526417119684,
40.1544081509837));
#22988=CARTESIAN_POINT('Ctrl Pts',(-1.5257082871409,-2.8392872467109,40.1512214838131));
#22989=CARTESIAN_POINT('Ctrl Pts',(-1.57548102869782,-2.81197460503496,
40.1480187586786));
#22990=CARTESIAN_POINT('Ctrl Pts',(-1.70398379898398,-2.73697318973332,
40.1395483182983));
#22991=CARTESIAN_POINT('Ctrl Pts',(-1.78141930899777,-2.6872153505836,40.1342378046197));
#22992=CARTESIAN_POINT('Ctrl Pts',(-1.90249889118442,-2.60187749789188,
40.1255031209275));
#22993=CARTESIAN_POINT('Ctrl Pts',(-1.94752644469264,-2.56834746770252,
40.1221525928023));
#22994=CARTESIAN_POINT('Ctrl Pts',(-2.00516054531332,-2.52304259246607,
40.1177164499752));
#22995=CARTESIAN_POINT('Ctrl Pts',(-2.01858226143142,-2.51231733105785,
40.1166725905314));
#22996=CARTESIAN_POINT('Ctrl Pts',(-2.04034132069919,-2.49464278845382,
40.1149622859871));
#22997=CARTESIAN_POINT('Ctrl Pts',(-2.04873056051132,-2.48775771183767,
40.1142984409028));
#22998=CARTESIAN_POINT('Ctrl Pts',(-2.06484634333585,-2.47439463355507,
40.1130145170621));
#22999=CARTESIAN_POINT('Ctrl Pts',(-2.07257758695582,-2.46792247984304,
40.1123946817282));
#23000=CARTESIAN_POINT('Ctrl Pts',(-2.09028095968121,-2.452960373389,40.1109662868802));
#23001=CARTESIAN_POINT('Ctrl Pts',(-2.10023191145538,-2.44444574367854,
40.1101567147658));
#23002=CARTESIAN_POINT('Ctrl Pts',(-2.12668913652012,-2.42152654799782,
40.1079861441118));
#23003=CARTESIAN_POINT('Ctrl Pts',(-2.14310066686595,-2.40701412531151,
40.1066206654441));
#23004=CARTESIAN_POINT('Ctrl Pts',(-2.28092614532539,-2.2826105235455,40.0949883346007));
#23005=CARTESIAN_POINT('Ctrl Pts',(-2.39393054758166,-2.1637968376173,40.084334731861));
#23006=CARTESIAN_POINT('Ctrl Pts',(-2.65772228599949,-1.84037116950742,
40.0564985965985));
#23007=CARTESIAN_POINT('Ctrl Pts',(-2.79426555286322,-1.62558571381885,
40.03899084047));
#23008=CARTESIAN_POINT('Ctrl Pts',(-2.92884012435285,-1.34582337006906,
40.018675713813));
#23009=CARTESIAN_POINT('Ctrl Pts',(-2.95211062396424,-1.29398176979983,
40.0150113002094));
#23010=CARTESIAN_POINT('Ctrl Pts',(-2.97850814812233,-1.23074925183527,
40.0106840442302));
#23011=CARTESIAN_POINT('Ctrl Pts',(-2.98295767820349,-1.21992541136176,
40.0099482798543));
#23012=CARTESIAN_POINT('Ctrl Pts',(-2.98979164271471,-1.20304027883689,
40.0088084576044));
#23013=CARTESIAN_POINT('Ctrl Pts',(-2.99221677429015,-1.19699572129119,
40.0084020044186));
#23014=CARTESIAN_POINT('Ctrl Pts',(-2.99668629148706,-1.18575713745136,
40.0076492799604));
#23015=CARTESIAN_POINT('Ctrl Pts',(-2.99873548786116,-1.18056520072981,
40.0073027280715));
#23016=CARTESIAN_POINT('Ctrl Pts',(-3.00334855925941,-1.16878780518274,
40.006519274946));
#23017=CARTESIAN_POINT('Ctrl Pts',(-3.00590426267253,-1.16219923758535,
40.0060828687203));
#23018=CARTESIAN_POINT('Ctrl Pts',(-3.01341777011743,-1.14263894015396,
40.0047926628828));
#23019=CARTESIAN_POINT('Ctrl Pts',(-3.01831350196856,-1.1296433174915,40.0039424989481));
#23020=CARTESIAN_POINT('Ctrl Pts',(-3.0545723447766,-1.03147617453332,39.9975704414923));
#23021=CARTESIAN_POINT('Ctrl Pts',(-3.08241199747418,-0.945036964367656,
39.9922418278056));
#23022=CARTESIAN_POINT('Ctrl Pts',(-3.17159661621014,-0.621948371578699,
39.9729602834399));
#23023=CARTESIAN_POINT('Ctrl Pts',(-3.2096208052385,-0.379727239062099,
39.9596794192817));
#23024=CARTESIAN_POINT('Ctrl Pts',(-3.2237571068219,-0.0438641655779862,
39.9405401526686));
#23025=CARTESIAN_POINT('Ctrl Pts',(-3.22369918435547,0.0479123905017251,
39.9352445049471));
#23026=CARTESIAN_POINT('Ctrl Pts',(-3.21730122645842,0.195520289011085,
39.9265320649528));
#23027=CARTESIAN_POINT('Ctrl Pts',(-3.21341697581568,0.251408294879304,
39.9231884468364));
#23028=CARTESIAN_POINT('Ctrl Pts',(-3.20644239769175,0.32425203327463,39.9187602840505));
#23029=CARTESIAN_POINT('Ctrl Pts',(-3.20466981922349,0.341326182438772,
39.9177173160471));
#23030=CARTESIAN_POINT('Ctrl Pts',(-3.2015545501712,0.369166240464658,39.9160081803709));
#23031=CARTESIAN_POINT('Ctrl Pts',(-3.20029373615862,0.379941111980566,
39.9153446071768));
#23032=CARTESIAN_POINT('Ctrl Pts',(-3.19775627028726,0.400716913116977,
39.9140610049007));
#23033=CARTESIAN_POINT('Ctrl Pts',(-3.19648704179784,0.410718634287481,
39.9134412180959));
#23034=CARTESIAN_POINT('Ctrl Pts',(-3.19346072759143,0.433702389973712,
39.9120126428223));
#23035=CARTESIAN_POINT('Ctrl Pts',(-3.19167138261563,0.44667992901306,39.9112028399393));
#23036=CARTESIAN_POINT('Ctrl Pts',(-3.18667602231112,0.481346201813041,
39.9090310010592));
#23037=CARTESIAN_POINT('Ctrl Pts',(-3.18332776837149,0.503013437111399,
39.9076644751009));
#23038=CARTESIAN_POINT('Ctrl Pts',(-3.1529390337906,0.687193131615201,39.8959691767041));
#23039=CARTESIAN_POINT('Ctrl Pts',(-3.11369923127039,0.847420280484252,
39.8852487209386));
#23040=CARTESIAN_POINT('Ctrl Pts',(-2.982657886704,1.24715090349905,39.8571851329669));
#23041=CARTESIAN_POINT('Ctrl Pts',(-2.87423617645597,1.47999848744319,39.8395110927366));
#23042=CARTESIAN_POINT('Ctrl Pts',(-2.71109840758028,1.74325926402472,39.8192791525069));
#23043=CARTESIAN_POINT('Ctrl Pts',(-2.68164099980509,1.78824209509877,39.8158162712529));
#23044=CARTESIAN_POINT('Ctrl Pts',(-2.64452351388311,1.8419406886083,39.811694889188));
#23045=CARTESIAN_POINT('Ctrl Pts',(-2.6379262467113,1.85137658033043,39.810971164671));
#23046=CARTESIAN_POINT('Ctrl Pts',(-2.62754202477367,1.86606064944886,39.8098459257176));
#23047=CARTESIAN_POINT('Ctrl Pts',(-2.62378966730064,1.87133300694688,39.8094421117172));
#23048=CARTESIAN_POINT('Ctrl Pts',(-2.61676823700227,1.88113603144475,39.8086917309303));
#23049=CARTESIAN_POINT('Ctrl Pts',(-2.61350329829536,1.88566945285615,39.8083448994666));
#23050=CARTESIAN_POINT('Ctrl Pts',(-2.60604731567502,1.89596564395544,39.8075575760942));
#23051=CARTESIAN_POINT('Ctrl Pts',(-2.60184894692927,1.90172300671287,39.8071175994328));
#23052=CARTESIAN_POINT('Ctrl Pts',(-2.59089152781911,1.91664507075308,39.8059778363865));
#23053=CARTESIAN_POINT('Ctrl Pts',(-2.58410286833128,1.92578804934161,39.8052800560322));
#23054=CARTESIAN_POINT('Ctrl Pts',(-2.54064840413865,1.98366907269412,39.8008649353722));
#23055=CARTESIAN_POINT('Ctrl Pts',(-2.50265108634127,2.03139753663881,39.7972345456825));
#23056=CARTESIAN_POINT('Ctrl Pts',(-2.44044027409346,2.10514318475714,39.7915905494667));
#23057=CARTESIAN_POINT('Ctrl Pts',(-2.41711427567274,2.13188538445169,39.7895363013204));
#23058=CARTESIAN_POINT('Ctrl Pts',(-2.23235480650211,2.33677208746604,39.7736894504789));
#23059=CARTESIAN_POINT('Ctrl Pts',(-2.05188364839378,2.49673737195673,39.7606126207799));
#23060=CARTESIAN_POINT('Ctrl Pts',(-1.77996205678656,2.68818524884868,39.7416817160656));
#23061=CARTESIAN_POINT('Ctrl Pts',(-1.70239841574455,2.7379632119031,39.7363646873085));
#23062=CARTESIAN_POINT('Ctrl Pts',(-1.57426976687456,2.81264096923382,39.7276201671238));
#23063=CARTESIAN_POINT('Ctrl Pts',(-1.52499706432151,2.8396580596163,39.7242665377114));
#23064=CARTESIAN_POINT('Ctrl Pts',(-1.45976460611466,2.87323863308815,39.7198268408919));
#23065=CARTESIAN_POINT('Ctrl Pts',(-1.44442125890776,2.88098249855008,39.7187826140009));
#23066=CARTESIAN_POINT('Ctrl Pts',(-1.41928793491564,2.89341617104172,39.7170718468481));
#23067=CARTESIAN_POINT('Ctrl Pts',(-1.4095347794069,2.89817996027282,39.7164079091796));
#23068=CARTESIAN_POINT('Ctrl Pts',(-1.39067592923892,2.90727358209375,39.7151239040334));
#23069=CARTESIAN_POINT('Ctrl Pts',(-1.38157360341922,2.91161013804268,39.7145040805141));
#23070=CARTESIAN_POINT('Ctrl Pts',(-1.36060372019867,2.92148019611838,39.7130758525399));
#23071=CARTESIAN_POINT('Ctrl Pts',(-1.34872254904603,2.92698419833303,39.7122664364141));
#23072=CARTESIAN_POINT('Ctrl Pts',(-1.31688253718308,2.94149919157231,39.7100965912793));
#23073=CARTESIAN_POINT('Ctrl Pts',(-1.29686511248134,2.95037928960949,39.7087316871857));
#23074=CARTESIAN_POINT('Ctrl Pts',(-1.12678705061772,3.02376378366411,39.6971265634845));
#23075=CARTESIAN_POINT('Ctrl Pts',(-0.972136342063126,3.07696812766912,
39.6865017053639));
#23076=CARTESIAN_POINT('Ctrl Pts',(-0.569019987400004,3.18221836682201,
39.6587180081901));
#23077=CARTESIAN_POINT('Ctrl Pts',(-0.317221819917639,3.21708917067282,
39.6412330911143));
#23078=CARTESIAN_POINT('Ctrl Pts',(-0.00658281150906346,3.22325392202767,
39.6208953911145));
#23079=CARTESIAN_POINT('Ctrl Pts',(0.0508030176557234,3.2228604061706,39.6171938793897));
#23080=CARTESIAN_POINT('Ctrl Pts',(0.119882245504012,3.22054088160411,39.6128287660732));
#23081=CARTESIAN_POINT('Ctrl Pts',(0.131610745624033,3.2200829095702,39.6120907984698));
#23082=CARTESIAN_POINT('Ctrl Pts',(0.149851292117261,3.21927082999772,39.610948270807));
#23083=CARTESIAN_POINT('Ctrl Pts',(0.15636506478163,3.21896102103265,39.6105412983858));
#23084=CARTESIAN_POINT('Ctrl Pts',(0.16845275427524,3.21834932697459,39.6097880407386));
#23085=CARTESIAN_POINT('Ctrl Pts',(0.174026775514854,3.21805273465272,39.6094414721545));
#23086=CARTESIAN_POINT('Ctrl Pts',(0.186647547058653,3.21734829889903,39.6086585176762));
#23087=CARTESIAN_POINT('Ctrl Pts',(0.193693727429667,3.21693178750267,39.6082226235358));
#23088=CARTESIAN_POINT('Ctrl Pts',(0.214556191184979,3.21562977872989,39.6069355119538));
#23089=CARTESIAN_POINT('Ctrl Pts',(0.228368408307645,3.21467838501386,39.6060879031744));
#23090=CARTESIAN_POINT('Ctrl Pts',(0.331437645587854,3.2069112607229,39.5997939293242));
#23091=CARTESIAN_POINT('Ctrl Pts',(0.42039097614108,3.19646763357667,39.5945354862197));
#23092=CARTESIAN_POINT('Ctrl Pts',(0.75171772543088,3.14349398231313,39.5752210712554));
#23093=CARTESIAN_POINT('Ctrl Pts',(0.989396096321654,3.07696985649079,39.5618576085669));
#23094=CARTESIAN_POINT('Ctrl Pts',(1.30196420350957,2.94947227069157,39.5426359611814));
#23095=CARTESIAN_POINT('Ctrl Pts',(1.38520845091741,2.91130436409413,39.5373512666229));
#23096=CARTESIAN_POINT('Ctrl Pts',(1.51651347907473,2.84419279245851,39.5286551452488));
#23097=CARTESIAN_POINT('Ctrl Pts',(1.56564228290785,2.81744732754238,39.5253165195216));
#23098=CARTESIAN_POINT('Ctrl Pts',(1.62889912782115,2.7808451209106,39.5208939676828));
#23099=CARTESIAN_POINT('Ctrl Pts',(1.64368096504025,2.77213362278265,39.519851476176));
#23100=CARTESIAN_POINT('Ctrl Pts',(1.6676934405881,2.7577225786824,39.5181428666633));
#23101=CARTESIAN_POINT('Ctrl Pts',(1.67696623195043,2.75209365485684,39.5174793390619));
#23102=CARTESIAN_POINT('Ctrl Pts',(1.69480401143186,2.74114184513632,39.5161956452952));
#23103=CARTESIAN_POINT('Ctrl Pts',(1.70337279269542,2.73582535585494,39.5155757204777));
#23104=CARTESIAN_POINT('Ctrl Pts',(1.72302158940155,2.72350619016021,39.5141465684993));
#23105=CARTESIAN_POINT('Ctrl Pts',(1.73408406062812,2.71647599435393,39.5133363250114));
#23106=CARTESIAN_POINT('Ctrl Pts',(1.76355271055686,2.69749531897932,39.5111627261614));
#23107=CARTESIAN_POINT('Ctrl Pts',(1.78187997285332,2.68542415321924,39.5097948706838));
#23108=CARTESIAN_POINT('Ctrl Pts',(1.93754087978799,2.58060375725869,39.4980370896905));
#23109=CARTESIAN_POINT('Ctrl Pts',(2.06763348275666,2.47759097241901,39.4872506874491));
#23110=CARTESIAN_POINT('Ctrl Pts',(2.37903539444383,2.18934086152986,39.4589349897228));
#23111=CARTESIAN_POINT('Ctrl Pts',(2.54700423324933,1.99142877288373,39.4410670920848));
#23112=CARTESIAN_POINT('Ctrl Pts',(2.71730081947909,1.73347579528025,39.420914434034));
#23113=CARTESIAN_POINT('Ctrl Pts',(2.74410215972377,1.69072945418358,39.4176698193342));
#23114=CARTESIAN_POINT('Ctrl Pts',(2.7756638746554,1.63766149748852,39.4137727225801));
#23115=CARTESIAN_POINT('Ctrl Pts',(2.78138623733969,1.62792374916509,39.4130629124998));
#23116=CARTESIAN_POINT('Ctrl Pts',(2.79028275332644,1.61260068922477,39.4119544949185));
#23117=CARTESIAN_POINT('Ctrl Pts',(2.79349153540256,1.6070357400336,39.4115536970625));
#23118=CARTESIAN_POINT('Ctrl Pts',(2.79946324941816,1.59660714180388,39.4108059356572));
#23119=CARTESIAN_POINT('Ctrl Pts',(2.80223012713352,1.59174594872404,39.4104587256807));
#23120=CARTESIAN_POINT('Ctrl Pts',(2.80852812601331,1.58061352732041,39.409666652134));
#23121=CARTESIAN_POINT('Ctrl Pts',(2.81205089982569,1.57433766915333,39.4092223285375));
#23122=CARTESIAN_POINT('Ctrl Pts',(2.82285439261683,1.55493917864139,39.4078555611918));
#23123=CARTESIAN_POINT('Ctrl Pts',(2.8300646219203,1.54177723006927,39.4069375215035));
#23124=CARTESIAN_POINT('Ctrl Pts',(2.90383910878204,1.40484377166515,39.3974776304722));
#23125=CARTESIAN_POINT('Ctrl Pts',(2.96234042603946,1.27687786512601,39.3894027369826));
#23126=CARTESIAN_POINT('Ctrl Pts',(3.1085142463978,0.892481908540035,39.3661852721921));
#23127=CARTESIAN_POINT('Ctrl Pts',(3.17246256163294,0.628382129195524,39.3514208794854));
#23128=CARTESIAN_POINT('Ctrl Pts',(3.21022702807425,0.291854640170197,39.3315753933734));
#23129=CARTESIAN_POINT('Ctrl Pts',(3.21566741099104,0.224095523279758,39.3275352790876));
#23130=CARTESIAN_POINT('Ctrl Pts',(3.21985153338909,0.137879565845321,39.3223177686998));
#23131=CARTESIAN_POINT('Ctrl Pts',(3.22058478502712,0.119533646090907,39.3212031576098));
#23132=CARTESIAN_POINT('Ctrl Pts',(3.22151014477212,0.0900747425718642,
39.3194059659622));
#23133=CARTESIAN_POINT('Ctrl Pts',(3.22180160437277,0.0789651144007929,
39.3187265140089));
#23134=CARTESIAN_POINT('Ctrl Pts',(3.22224633524775,0.0578472412051899,
39.3174316687083));
#23135=CARTESIAN_POINT('Ctrl Pts',(3.22241045532736,0.0478393365818509,
39.3168166241478));
#23136=CARTESIAN_POINT('Ctrl Pts',(3.22267799293404,0.0250498448599227,
39.3154127982733));
#23137=CARTESIAN_POINT('Ctrl Pts',(3.22275199573299,0.0122681419001293,
39.3146231015749));
#23138=CARTESIAN_POINT('Ctrl Pts',(3.22274577406068,-0.0267780763807966,
39.3122033488369));
#23139=CARTESIAN_POINT('Ctrl Pts',(3.22242051587675,-0.0530409511759957,
39.3105656360131));
#23140=CARTESIAN_POINT('Ctrl Pts',(3.21657546869301,-0.29052267298961,39.2956612460516));
#23141=CARTESIAN_POINT('Ctrl Pts',(3.19061820458058,-0.500686094542264,
39.2817366890936));
#23142=CARTESIAN_POINT('Ctrl Pts',(3.09075946592093,-0.944944400017209,
39.2510492829271));
#23143=CARTESIAN_POINT('Ctrl Pts',(3.01033022951578,-1.17628252723634,39.2342736439257));
#23144=CARTESIAN_POINT('Ctrl Pts',(2.89512845967804,-1.41591705781204,39.2172917697573));
#23145=CARTESIAN_POINT('Ctrl Pts',(2.88551367160884,-1.43540963624992,39.2159139564565));
#23146=CARTESIAN_POINT('Ctrl Pts',(2.87181285948336,-1.46249194612545,39.2140061827161));
#23147=CARTESIAN_POINT('Ctrl Pts',(2.86789273040673,-1.47016430486403,39.2134664513934));
#23148=CARTESIAN_POINT('Ctrl Pts',(2.86153335074908,-1.48248845911567,39.2126007785497));
#23149=CARTESIAN_POINT('Ctrl Pts',(2.85911344694395,-1.48715010920516,39.2122736360001));
#23150=CARTESIAN_POINT('Ctrl Pts',(2.85401673085687,-1.49690988973128,39.2115893848141));
#23151=CARTESIAN_POINT('Ctrl Pts',(2.85133763931079,-1.50200678603902,39.2112324302642));
#23152=CARTESIAN_POINT('Ctrl Pts',(2.84478889249885,-1.51438492775443,39.2103664167005));
#23153=CARTESIAN_POINT('Ctrl Pts',(2.84090489133678,-1.52165861946619,39.2098582634325));
#23154=CARTESIAN_POINT('Ctrl Pts',(2.82703185631834,-1.54740082260892,39.2080621990342));
#23155=CARTESIAN_POINT('Ctrl Pts',(2.81689004788105,-1.56578700154801,39.2067836464197));
#23156=CARTESIAN_POINT('Ctrl Pts',(2.75422559740134,-1.67681223100307,39.1990810755065));
#23157=CARTESIAN_POINT('Ctrl Pts',(2.69731210723424,-1.76690972779765,39.1929061646783));
#23158=CARTESIAN_POINT('Ctrl Pts',(2.5162037334278,-2.0244070249798,39.1749889155812));
#23159=CARTESIAN_POINT('Ctrl Pts',(2.38013532283281,-2.18276568316848,39.1635801291983));
#23160=CARTESIAN_POINT('Ctrl Pts',(2.1980573943836,-2.35724114196146,39.14926506881));
#23161=CARTESIAN_POINT('Ctrl Pts',(2.16576695546997,-2.38694269429084,39.1467594420274));
#23162=CARTESIAN_POINT('Ctrl Pts',(2.10017667605733,-2.44484737164205,39.1417207489274));
#23163=CARTESIAN_POINT('Ctrl Pts',(2.06689045827015,-2.47305162762471,39.1391884508847));
#23164=CARTESIAN_POINT('Ctrl Pts',(1.98128089139269,-2.54265490726078,39.1327225860384));
#23165=CARTESIAN_POINT('Ctrl Pts',(1.92822767164798,-2.5831192478746,39.1287580645187));
#23166=CARTESIAN_POINT('Ctrl Pts',(1.85846877584393,-2.63297814814501,39.1235783252825));
#23167=CARTESIAN_POINT('Ctrl Pts',(1.84288025072208,-2.64391234287018,39.1224229381918));
#23168=CARTESIAN_POINT('Ctrl Pts',(1.8179171454286,-2.66109407940087,39.1205756050772));
#23169=CARTESIAN_POINT('Ctrl Pts',(1.80860496339993,-2.66743182262345,39.1198871095989));
#23170=CARTESIAN_POINT('Ctrl Pts',(1.7918059536015,-2.67873658804928,39.1186461149906));
#23171=CARTESIAN_POINT('Ctrl Pts',(1.78433118602807,-2.68372139006235,39.1180942973701));
#23172=CARTESIAN_POINT('Ctrl Pts',(1.76677546701283,-2.6953232500139,39.1167990657712));
#23173=CARTESIAN_POINT('Ctrl Pts',(1.75667807853348,-2.70191507915415,39.1160547127544));
#23174=CARTESIAN_POINT('Ctrl Pts',(1.72745845266876,-2.72075735544246,39.1139023447241));
#23175=CARTESIAN_POINT('Ctrl Pts',(1.70824371547161,-2.73286235636227,39.1124889421898));
#23176=CARTESIAN_POINT('Ctrl Pts',(1.56347904162417,-2.8219387156103,39.1018531150306));
#23177=CARTESIAN_POINT('Ctrl Pts',(1.43293094927243,-2.89041569172864,39.0923210311563));
#23178=CARTESIAN_POINT('Ctrl Pts',(1.12299206918269,-3.02682003572455,39.0698561276923));
#23179=CARTESIAN_POINT('Ctrl Pts',(0.941295114479844,-3.08815576330052,
39.0567926850927));
#23180=CARTESIAN_POINT('Ctrl Pts',(0.626296591991462,-3.16408990104728,
39.0349901274769));
#23181=CARTESIAN_POINT('Ctrl Pts',(0.495532729666177,-3.18718810240982,
39.0261834329234));
#23182=CARTESIAN_POINT('Ctrl Pts',(0.348856801022213,-3.20384765012721,
39.0168239504983));
#23183=CARTESIAN_POINT('Ctrl Pts',(0.333998138707797,-3.20543071933491,
39.015881734465));
#23184=CARTESIAN_POINT('Ctrl Pts',(0.311979624632646,-3.20762184356043,
39.0144948003946));
#23185=CARTESIAN_POINT('Ctrl Pts',(0.30482813779362,-3.20830936573366,39.0140457832456));
#23186=CARTESIAN_POINT('Ctrl Pts',(0.292105850759773,-3.20948952471186,
39.0132496467793));
#23187=CARTESIAN_POINT('Ctrl Pts',(0.286536018534134,-3.2099915808396,39.0129020041156));
#23188=CARTESIAN_POINT('Ctrl Pts',(0.27455706398531,-3.21103991789833,39.0121562976743));
#23189=CARTESIAN_POINT('Ctrl Pts',(0.268147622524599,-3.21158150915796,
39.0117585000821));
#23190=CARTESIAN_POINT('Ctrl Pts',(0.250441275974636,-3.21302430115474,
39.0106627725796));
#23191=CARTESIAN_POINT('Ctrl Pts',(0.239141043331531,-3.21388511973132,
39.0099670776138));
#23192=CARTESIAN_POINT('Ctrl Pts',(0.17696229066587,-3.21829195016714,39.0061577092385));
#23193=CARTESIAN_POINT('Ctrl Pts',(0.126006496722375,-3.22068964190635,
39.0031045191778));
#23194=CARTESIAN_POINT('Ctrl Pts',(-0.1830946739326,-3.22788616433542,38.9848837179768));
#23195=CARTESIAN_POINT('Ctrl Pts',(-0.441014466588179,-3.20285955449788,
38.9708829805337));
#23196=CARTESIAN_POINT('Ctrl Pts',(-0.85485490292943,-3.1117099640274,38.9469569118957));
#23197=CARTESIAN_POINT('Ctrl Pts',(-1.01350044503538,-3.06371049011604,
38.9374236231667));
#23198=CARTESIAN_POINT('Ctrl Pts',(-1.18819681511353,-2.99579494117757,
38.9261504041177));
#23199=CARTESIAN_POINT('Ctrl Pts',(-1.20856532806469,-2.98763599060569,
38.9248239579017));
#23200=CARTESIAN_POINT('Ctrl Pts',(-1.24096468549849,-2.9742723458415,38.9226939920739));
#23201=CARTESIAN_POINT('Ctrl Pts',(-1.25305006745087,-2.96920104714872,
38.9218949925177));
#23202=CARTESIAN_POINT('Ctrl Pts',(-1.27437855958805,-2.96009772403249,
38.9204767872859));
#23203=CARTESIAN_POINT('Ctrl Pts',(-1.28363436311561,-2.95609574728522,
38.9198586142834));
#23204=CARTESIAN_POINT('Ctrl Pts',(-1.30280799442383,-2.94769852125175,
38.918572321186));
#23205=CARTESIAN_POINT('Ctrl Pts',(-1.31272270426616,-2.94329650895409,
38.9179039748818));
#23206=CARTESIAN_POINT('Ctrl Pts',(-1.3382631435736,-2.93180213933663,38.9161739220505));
#23207=CARTESIAN_POINT('Ctrl Pts',(-1.35385463617362,-2.92463495695087,
38.9151096443797));
#23208=CARTESIAN_POINT('Ctrl Pts',(-1.40499449194601,-2.90063014056312,
38.9115915079834));
#23209=CARTESIAN_POINT('Ctrl Pts',(-1.44028948151397,-2.883267330633,38.9091195882205));
#23210=CARTESIAN_POINT('Ctrl Pts',(-1.47525540693158,-2.86526421937299,
38.9066255640146));
#23211=CARTESIAN_POINT('Ctrl Pts',(-1.47525532932068,-2.86526425933297,
38.6590632205222));
#23212=CARTESIAN_POINT('Ctrl Pts',(-1.28407448727895,-2.96369865510202,
38.671285489794));
#23213=CARTESIAN_POINT('Ctrl Pts',(-1.08344525766489,-3.04279164141386,
38.6830572974952));
#23214=CARTESIAN_POINT('Ctrl Pts',(-0.788298988501228,-3.126191380641,38.7005217387652));
#23215=CARTESIAN_POINT('Ctrl Pts',(-0.699243561028461,-3.14730748079575,
38.7058035438473));
#23216=CARTESIAN_POINT('Ctrl Pts',(-0.554520133269385,-3.17517719228224,
38.7144951307614));
#23217=CARTESIAN_POINT('Ctrl Pts',(-0.499362042980586,-3.18431778565124,
38.7178321985447));
#23218=CARTESIAN_POINT('Ctrl Pts',(-0.427008882053403,-3.19438180882905,
38.7222527501882));
#23219=CARTESIAN_POINT('Ctrl Pts',(-0.4100029068956,-3.1966090353024,38.7232948396561));
#23220=CARTESIAN_POINT('Ctrl Pts',(-0.382217487871135,-3.20002264666423,
38.7250028045136));
#23221=CARTESIAN_POINT('Ctrl Pts',(-0.371448260896553,-3.20129057289873,
38.725666091599));
#23222=CARTESIAN_POINT('Ctrl Pts',(-0.35065562984874,-3.20363228400043,
38.7269493293259));
#23223=CARTESIAN_POINT('Ctrl Pts',(-0.340633170662929,-3.20471343823334,
38.7275690388482));
#23224=CARTESIAN_POINT('Ctrl Pts',(-0.317571989813094,-3.20709171731181,
38.7289977066194));
#23225=CARTESIAN_POINT('Ctrl Pts',(-0.304530166870745,-3.20835637379617,
38.7298076805755));
#23226=CARTESIAN_POINT('Ctrl Pts',(-0.269632609653829,-3.21152566765951,
38.7319805786219));
#23227=CARTESIAN_POINT('Ctrl Pts',(-0.247764831074532,-3.2132866987346,
38.7333480001095));
#23228=CARTESIAN_POINT('Ctrl Pts',(-0.060656220350022,-3.22643339498369,
38.7450998303797));
#23229=CARTESIAN_POINT('Ctrl Pts',(0.105191485909992,-3.22528622545785,
38.7558802854321));
#23230=CARTESIAN_POINT('Ctrl Pts',(0.527376311259654,-3.18976522331647,
38.7841513322817));
#23231=CARTESIAN_POINT('Ctrl Pts',(0.781014796840861,-3.1373141480355,38.8019781425205));
#23232=CARTESIAN_POINT('Ctrl Pts',(1.07405394425557,-3.03893561923401,38.8221387662267));
#23233=CARTESIAN_POINT('Ctrl Pts',(1.12204082752715,-3.02154706242529,38.8254219409099));
#23234=CARTESIAN_POINT('Ctrl Pts',(1.1801568336041,-2.99891243998137,38.8293586228693));
#23235=CARTESIAN_POINT('Ctrl Pts',(1.19069455895295,-2.99474413779865,38.8300708189757));
#23236=CARTESIAN_POINT('Ctrl Pts',(1.20717751417929,-2.98812338515305,38.8311820456652));
#23237=CARTESIAN_POINT('Ctrl Pts',(1.2131376407651,-2.98570862307673,38.8315832854799));
#23238=CARTESIAN_POINT('Ctrl Pts',(1.22426546879922,-2.98116133007865,38.8323312928323));
#23239=CARTESIAN_POINT('Ctrl Pts',(1.22943479198025,-2.97903321682104,38.8326783101273));
#23240=CARTESIAN_POINT('Ctrl Pts',(1.24123136243931,-2.97414085520648,38.8334691867301));
#23241=CARTESIAN_POINT('Ctrl Pts',(1.24785491385004,-2.97136790688149,38.8339125112813));
#23242=CARTESIAN_POINT('Ctrl Pts',(1.26822193345918,-2.96276114505854,38.83527359686));
#23243=CARTESIAN_POINT('Ctrl Pts',(1.28193440445722,-2.95685384788623,38.8361870054277));
#23244=CARTESIAN_POINT('Ctrl Pts',(1.41626744121304,-2.89787336426817,38.8451106006821));
#23245=CARTESIAN_POINT('Ctrl Pts',(1.53358211754802,-2.83753733299432,38.8527106759889));
#23246=CARTESIAN_POINT('Ctrl Pts',(1.82009682533644,-2.66720294482605,38.8715769792473));
#23247=CARTESIAN_POINT('Ctrl Pts',(1.98326834980852,-2.54820975285874,38.8826373588631));
#23248=CARTESIAN_POINT('Ctrl Pts',(2.20320026995289,-2.35382483260806,38.8993472110471));
#23249=CARTESIAN_POINT('Ctrl Pts',(2.26949388351596,-2.28997343888693,38.9046576200447));
#23250=CARTESIAN_POINT('Ctrl Pts',(2.37168587292633,-2.18274465202265,38.913391970288));
#23251=CARTESIAN_POINT('Ctrl Pts',(2.4093396660718,-2.14110950022714,38.9167422569918));
#23252=CARTESIAN_POINT('Ctrl Pts',(2.45706978185443,-2.08547852234036,38.9211778796392));
#23253=CARTESIAN_POINT('Ctrl Pts',(2.46814952794719,-2.07235384767475,38.9222214618484));
#23254=CARTESIAN_POINT('Ctrl Pts',(2.48605560647135,-2.05079564751309,38.9239312588243));
#23255=CARTESIAN_POINT('Ctrl Pts',(2.49294529191739,-2.04241500025859,38.9245948745641));
#23256=CARTESIAN_POINT('Ctrl Pts',(2.50615350081707,-2.02618206799042,38.9258783164783));
#23257=CARTESIAN_POINT('Ctrl Pts',(2.51247777182223,-2.01833460672897,38.9264978992126));
#23258=CARTESIAN_POINT('Ctrl Pts',(2.52693132591901,-2.00022673627236,38.9279256557813));
#23259=CARTESIAN_POINT('Ctrl Pts',(2.53503507088338,-1.98994625647866,38.9287348410906));
#23260=CARTESIAN_POINT('Ctrl Pts',(2.55652532792222,-1.96233921977238,38.9309042461241));
#23261=CARTESIAN_POINT('Ctrl Pts',(2.56979809190432,-1.94492536987769,38.9322689405519));
#23262=CARTESIAN_POINT('Ctrl Pts',(2.68064589397213,-1.79637748776523,38.9438811116159));
#23263=CARTESIAN_POINT('Ctrl Pts',(2.7682766615979,-1.65815084661719,38.9545138332772));
#23264=CARTESIAN_POINT('Ctrl Pts',(2.96391275139813,-1.29049491292741,38.9822876383255));
#23265=CARTESIAN_POINT('Ctrl Pts',(3.0560559650172,-1.05388462986568,38.99975275878));
#23266=CARTESIAN_POINT('Ctrl Pts',(3.1340222851665,-0.753216771649467,39.0200869078658));
#23267=CARTESIAN_POINT('Ctrl Pts',(3.14697694837441,-0.69711422990077,39.0238010814912));
#23268=CARTESIAN_POINT('Ctrl Pts',(3.16075742472357,-0.62918042395756,39.0281788341636));
#23269=CARTESIAN_POINT('Ctrl Pts',(3.16302943231293,-0.617657125093158,
39.0289172934967));
#23270=CARTESIAN_POINT('Ctrl Pts',(3.16646486897041,-0.599716865689503,
39.0300603048312));
#23271=CARTESIAN_POINT('Ctrl Pts',(3.16767187543463,-0.593308500516473,
39.0304672739813));
#23272=CARTESIAN_POINT('Ctrl Pts',(3.1698755038158,-0.581410339263496,39.0312203711134));
#23273=CARTESIAN_POINT('Ctrl Pts',(3.17087731134209,-0.575921669543651,
39.031566783207));
#23274=CARTESIAN_POINT('Ctrl Pts',(3.17311304417515,-0.563489927102145,
39.0323491718734));
#23275=CARTESIAN_POINT('Ctrl Pts',(3.17433843522563,-0.556545406900894,
39.032784658381));
#23276=CARTESIAN_POINT('Ctrl Pts',(3.17789792682124,-0.535978855656356,
39.0340698933367));
#23277=CARTESIAN_POINT('Ctrl Pts',(3.18016724296081,-0.5223455653897,39.0349160473253));
#23278=CARTESIAN_POINT('Ctrl Pts',(3.19638794546752,-0.420870913814157,
39.0411737663143));
#23279=CARTESIAN_POINT('Ctrl Pts',(3.20678665715305,-0.332491599773301,
39.0463998251197));
#23280=CARTESIAN_POINT('Ctrl Pts',(3.21959808597111,-0.163615866077885,
39.0561515490697));
#23281=CARTESIAN_POINT('Ctrl Pts',(3.22267806929456,-0.083241512514831,
39.0606928146395));
#23282=CARTESIAN_POINT('Ctrl Pts',(3.22300035142336,0.283371477487148,39.0812650273812));
#23283=CARTESIAN_POINT('Ctrl Pts',(3.18512972088702,0.56830024843683,39.0969964397528));
#23284=CARTESIAN_POINT('Ctrl Pts',(3.10136656492807,0.876791876939508,39.1160906873797));
#23285=CARTESIAN_POINT('Ctrl Pts',(3.09209046345141,0.908963697782091,39.1181059828272));
#23286=CARTESIAN_POINT('Ctrl Pts',(3.0785040457592,0.953467757204457,39.1209296153227));
#23287=CARTESIAN_POINT('Ctrl Pts',(3.07461726803527,0.965927829109165,39.1217240969029));
#23288=CARTESIAN_POINT('Ctrl Pts',(3.06778297368048,0.987377682112405,39.1230987240027));
#23289=CARTESIAN_POINT('Ctrl Pts',(3.06487134467569,0.996378792579462,39.1236776826933));
#23290=CARTESIAN_POINT('Ctrl Pts',(3.05876455609028,1.01497747475644,39.1248784105621));
#23291=CARTESIAN_POINT('Ctrl Pts',(3.05556376100611,1.02457307331343,39.1255003607382));
#23292=CARTESIAN_POINT('Ctrl Pts',(3.04796937799707,1.04698799932642,39.1269590492139));
#23293=CARTESIAN_POINT('Ctrl Pts',(3.04354002876989,1.05979492553884,39.1277969672757));
#23294=CARTESIAN_POINT('Ctrl Pts',(3.02892318728499,1.1012102934382,39.1305214350045));
#23295=CARTESIAN_POINT('Ctrl Pts',(3.01841230847862,1.12970209300049,39.1324187212863));
#23296=CARTESIAN_POINT('Ctrl Pts',(2.96261906407752,1.2746005160825,39.1421885313019));
#23297=CARTESIAN_POINT('Ctrl Pts',(2.91100480269604,1.38843892057456,39.1502725301293));
#23298=CARTESIAN_POINT('Ctrl Pts',(2.73746367588499,1.71872862827424,39.1749469343045));
#23299=CARTESIAN_POINT('Ctrl Pts',(2.59701815017566,1.92437427322692,39.1920356184189));
#23300=CARTESIAN_POINT('Ctrl Pts',(2.37679540635408,2.17822909856052,39.2143594642086));
#23301=CARTESIAN_POINT('Ctrl Pts',(2.31651925375649,2.24222656889907,39.2201023517836));
#23302=CARTESIAN_POINT('Ctrl Pts',(2.24384581848401,2.31332302686861,39.2265409233234));
#23303=CARTESIAN_POINT('Ctrl Pts',(2.2339328241013,2.32289725066601,39.2274092544808));
#23304=CARTESIAN_POINT('Ctrl Pts',(2.21886104938312,2.33726823751822,39.2287141439041));
#23305=CARTESIAN_POINT('Ctrl Pts',(2.21374760868439,2.34211201650658,39.2291542242887));
#23306=CARTESIAN_POINT('Ctrl Pts',(2.20455559765037,2.35076228100756,39.2299405482151));
#23307=CARTESIAN_POINT('Ctrl Pts',(2.20048300260674,2.35457495988372,39.230287265748));
#23308=CARTESIAN_POINT('Ctrl Pts',(2.19162387500514,2.36282562994989,39.2310378589657));
#23309=CARTESIAN_POINT('Ctrl Pts',(2.18683376856828,2.36725964724496,39.2314414318532));
#23310=CARTESIAN_POINT('Ctrl Pts',(2.17336571301225,2.37965074318618,39.2325698967051));
#23311=CARTESIAN_POINT('Ctrl Pts',(2.16465747733956,2.38757496171443,39.233292327543));
#23312=CARTESIAN_POINT('Ctrl Pts',(2.11275200052783,2.43428988165557,39.2375571819236));
#23313=CARTESIAN_POINT('Ctrl Pts',(2.06855335562532,2.47195797546705,39.2410207800469));
#23314=CARTESIAN_POINT('Ctrl Pts',(1.82669438903894,2.66704829677977,39.259245557701));
#23315=CARTESIAN_POINT('Ctrl Pts',(1.61204044770465,2.80201906718346,39.2729602638246));
#23316=CARTESIAN_POINT('Ctrl Pts',(1.23635327855258,2.98063822673124,39.2964607938358));
#23317=CARTESIAN_POINT('Ctrl Pts',(1.0838085218015,3.03942797261869,39.3058707943695));
#23318=CARTESIAN_POINT('Ctrl Pts',(0.906513600552543,3.09270591965345,39.317005765055));
#23319=CARTESIAN_POINT('Ctrl Pts',(0.885484730473467,3.09879227592305,39.3183292362209));
#23320=CARTESIAN_POINT('Ctrl Pts',(0.851786065699515,3.10817460799464,39.3204551846339));
#23321=CARTESIAN_POINT('Ctrl Pts',(0.839155134502183,3.11160851454795,39.3212531671907));
#23322=CARTESIAN_POINT('Ctrl Pts',(0.816762353239068,3.11755006327165,39.3226700216246));
#23323=CARTESIAN_POINT('Ctrl Pts',(0.807008945445506,3.12008905273223,39.3232878656914));
#23324=CARTESIAN_POINT('Ctrl Pts',(0.78673154836555,3.12526618801908,39.3245739266984));
#23325=CARTESIAN_POINT('Ctrl Pts',(0.776205839233688,3.12789701967621,39.3252423719447));
#23326=CARTESIAN_POINT('Ctrl Pts',(0.748980992174118,3.13455580899825,39.32697365105));
#23327=CARTESIAN_POINT('Ctrl Pts',(0.732262739341119,3.13850345045512,39.3280390646258));
#23328=CARTESIAN_POINT('Ctrl Pts',(0.660767690658835,3.15478306322465,39.3326054712275));
#23329=CARTESIAN_POINT('Ctrl Pts',(0.605707975589027,3.16581542820628,39.3361478758941));
#23330=CARTESIAN_POINT('Ctrl Pts',(0.459694296651282,3.19112389498064,39.3456156479761));
#23331=CARTESIAN_POINT('Ctrl Pts',(0.368373377273709,3.2029500595136,39.3516128713068));
#23332=CARTESIAN_POINT('Ctrl Pts',(0.0361003955840009,3.23158191611163,
39.3736765843402));
#23333=CARTESIAN_POINT('Ctrl Pts',(-0.206019566525885,3.22520791140348,
39.3902812914309));
#23334=CARTESIAN_POINT('Ctrl Pts',(-0.537365088622875,3.17899771848399,
39.4125479615176));
#23335=CARTESIAN_POINT('Ctrl Pts',(-0.628995432904767,3.16214420919996,
39.4186455967354));
#23336=CARTESIAN_POINT('Ctrl Pts',(-0.733386359925439,3.13822513357812,
39.4254294925948));
#23337=CARTESIAN_POINT('Ctrl Pts',(-0.746977027195903,3.13501800304144,
39.4263094522589));
#23338=CARTESIAN_POINT('Ctrl Pts',(-0.767428929536656,3.13005120710026,
39.4276283282962));
#23339=CARTESIAN_POINT('Ctrl Pts',(-0.774305703008538,3.12835714098051,
39.428070877633));
#23340=CARTESIAN_POINT('Ctrl Pts',(-0.786592154576694,3.12528742681839,
39.4288598623279));
#23341=CARTESIAN_POINT('Ctrl Pts',(-0.792003876800657,3.12392038608281,
39.4292067854653));
#23342=CARTESIAN_POINT('Ctrl Pts',(-0.803708711335837,3.12093128762173,
39.4299558355472));
#23343=CARTESIAN_POINT('Ctrl Pts',(-0.810000458436784,3.119304257976,39.4303576704154));
#23344=CARTESIAN_POINT('Ctrl Pts',(-0.82754980126605,3.11470936497899,39.4314763551853));
#23345=CARTESIAN_POINT('Ctrl Pts',(-0.838796434810256,3.11169947977874,
39.4321908123323));
#23346=CARTESIAN_POINT('Ctrl Pts',(-0.903897274126563,3.09389823740208,
39.4363134609622));
#23347=CARTESIAN_POINT('Ctrl Pts',(-0.95737965684929,3.07776894068284,39.43964882841));
#23348=CARTESIAN_POINT('Ctrl Pts',(-1.2518885347879,2.98052955051237,39.4578658146912));
#23349=CARTESIAN_POINT('Ctrl Pts',(-1.48309546221237,2.87249658179732,39.4716649417582));
#23350=CARTESIAN_POINT('Ctrl Pts',(-1.8386133958519,2.6518923002712,39.4952971602274));
#23351=CARTESIAN_POINT('Ctrl Pts',(-1.97118680334568,2.55488631984889,39.5047503130499));
#23352=CARTESIAN_POINT('Ctrl Pts',(-2.11243334642095,2.43397265135256,39.5159335508639));
#23353=CARTESIAN_POINT('Ctrl Pts',(-2.12892990574813,2.41955676327569,39.5172579715009));
#23354=CARTESIAN_POINT('Ctrl Pts',(-2.15504938944001,2.39625773823557,39.5193851613114));
#23355=CARTESIAN_POINT('Ctrl Pts',(-2.1647675498707,2.38748203471025,39.5201834275149));
#23356=CARTESIAN_POINT('Ctrl Pts',(-2.18187119911505,2.3718467964462,39.5216006156333));
#23357=CARTESIAN_POINT('Ctrl Pts',(-2.18927853627438,2.36501134083585,39.5222185081888));
#23358=CARTESIAN_POINT('Ctrl Pts',(-2.20459104976112,2.35074744238787,39.5235045006977));
#23359=CARTESIAN_POINT('Ctrl Pts',(-2.21249101923929,2.34331361959059,39.5241728281175));
#23360=CARTESIAN_POINT('Ctrl Pts',(-2.23279739041388,2.32401122113596,39.525903437912));
#23361=CARTESIAN_POINT('Ctrl Pts',(-2.24514662512567,2.31208325021044,39.5269682961416));
#23362=CARTESIAN_POINT('Ctrl Pts',(-2.29741377919766,2.260785459167,39.531529034092));
#23363=CARTESIAN_POINT('Ctrl Pts',(-2.33639397209793,2.22047822220215,39.535066197085));
#23364=CARTESIAN_POINT('Ctrl Pts',(-2.43641663291798,2.1114994904577,39.5445163802376));
#23365=CARTESIAN_POINT('Ctrl Pts',(-2.49560495771744,2.04120295070135,39.5505009238395));
#23366=CARTESIAN_POINT('Ctrl Pts',(-2.70039315703021,1.77573954144471,39.5726797617604));
#23367=CARTESIAN_POINT('Ctrl Pts',(-2.82674938959659,1.56679511673867,39.589424555875));
#23368=CARTESIAN_POINT('Ctrl Pts',(-2.96659722480782,1.26245684601902,39.6117037022118));
#23369=CARTESIAN_POINT('Ctrl Pts',(-3.00126028822044,1.17768265432542,39.6176945061403));
#23370=CARTESIAN_POINT('Ctrl Pts',(-3.03698126438962,1.07845068675902,39.6243746911029));
#23371=CARTESIAN_POINT('Ctrl Pts',(-3.04160826559865,1.06533105610021,39.6252513143447));
#23372=CARTESIAN_POINT('Ctrl Pts',(-3.04845888693301,1.04549795695694,39.6265661801149));
#23373=CARTESIAN_POINT('Ctrl Pts',(-3.05074553083901,1.03880665749362,39.6270080236295));
#23374=CARTESIAN_POINT('Ctrl Pts',(-3.05479744172909,1.02682096667632,39.6277962428935));
#23375=CARTESIAN_POINT('Ctrl Pts',(-3.05657099059342,1.02152948495501,39.628143102517));
#23376=CARTESIAN_POINT('Ctrl Pts',(-3.06038254249641,1.01005870677849,39.6288925726029));
#23377=CARTESIAN_POINT('Ctrl Pts',(-3.06241557425149,1.003877856069,39.629294887994));
#23378=CARTESIAN_POINT('Ctrl Pts',(-3.06804543520717,0.986585611056661,
39.6304163038666));
#23379=CARTESIAN_POINT('Ctrl Pts',(-3.07160064736433,0.975460626208227,
39.631132992443));
#23380=CARTESIAN_POINT('Ctrl Pts',(-3.0919892720848,0.910443617439896,39.6352950129623));
#23381=CARTESIAN_POINT('Ctrl Pts',(-3.10746576956372,0.856132367811441,
39.6386658815996));
#23382=CARTESIAN_POINT('Ctrl Pts',(-3.18462999296485,0.555586948438195,
39.6568839990104));
#23383=CARTESIAN_POINT('Ctrl Pts',(-3.21849228996203,0.303116389506117,
39.6706588904062));
#23384=CARTESIAN_POINT('Ctrl Pts',(-3.22487832653238,-0.114571260589173,
39.6942546760087));
#23385=CARTESIAN_POINT('Ctrl Pts',(-3.21488456870987,-0.278340731235344,
39.7036969409756));
#23386=CARTESIAN_POINT('Ctrl Pts',(-3.18949094369585,-0.462325471573138,
39.7148679913995));
#23387=CARTESIAN_POINT('Ctrl Pts',(-3.18627515336803,-0.483991665559696,
39.7161921534439));
#23388=CARTESIAN_POINT('Ctrl Pts',(-3.18078468245329,-0.518553550875952,
39.7183189952192));
#23389=CARTESIAN_POINT('Ctrl Pts',(-3.17865179173586,-0.531471316450938,
39.7191171740483));
#23390=CARTESIAN_POINT('Ctrl Pts',(-3.17473778144699,-0.554309629524622,
39.7205342471714));
#23391=CARTESIAN_POINT('Ctrl Pts',(-3.17298871556446,-0.564235547945788,
39.7211521124968));
#23392=CARTESIAN_POINT('Ctrl Pts',(-3.16926052130431,-0.584827313269401,
39.7224380882202));
#23393=CARTESIAN_POINT('Ctrl Pts',(-3.1672740466979,-0.595491684871205,
39.7231064262771));
#23394=CARTESIAN_POINT('Ctrl Pts',(-3.16200424339392,-0.623010083338556,
39.7248371490724));
#23395=CARTESIAN_POINT('Ctrl Pts',(-3.15864002288915,-0.6398480964976,39.7259021105103));
#23396=CARTESIAN_POINT('Ctrl Pts',(-3.14371400603114,-0.711565311408102,
39.7304640565655));
#23397=CARTESIAN_POINT('Ctrl Pts',(-3.13085585754201,-0.76616180125175,
39.7340023534215));
#23398=CARTESIAN_POINT('Ctrl Pts',(-3.09318546081508,-0.9092674950203,39.7434563852011));
#23399=CARTESIAN_POINT('Ctrl Pts',(-3.06600146818817,-0.997093852123104,
39.7494437189835));
#23400=CARTESIAN_POINT('Ctrl Pts',(-2.9533884000279,-1.31250740328511,39.7715991691548));
#23401=CARTESIAN_POINT('Ctrl Pts',(-2.84605622288976,-1.53138097428601,
39.7883152533023));
#23402=CARTESIAN_POINT('Ctrl Pts',(-2.6656712648271,-1.81349164490135,39.8105916885811));
#23403=CARTESIAN_POINT('Ctrl Pts',(-2.61289646902171,-1.88873785391463,
39.8166042216249));
#23404=CARTESIAN_POINT('Ctrl Pts',(-2.54849956332873,-1.97267872563566,
39.8233055030797));
#23405=CARTESIAN_POINT('Ctrl Pts',(-2.53995393823379,-1.98366967688043,
39.8241828027881));
#23406=CARTESIAN_POINT('Ctrl Pts',(-2.52695942185555,-2.00016091207473,
39.8254984758337));
#23407=CARTESIAN_POINT('Ctrl Pts',(-2.52256333649863,-2.00570232325646,
39.825940456732));
#23408=CARTESIAN_POINT('Ctrl Pts',(-2.51466612406436,-2.01558998636422,
39.8267288199463));
#23409=CARTESIAN_POINT('Ctrl Pts',(-2.51117193107576,-2.01994164341351,
39.8270756869182));
#23410=CARTESIAN_POINT('Ctrl Pts',(-2.50358053567092,-2.02934580015975,
39.8278250595716));
#23411=CARTESIAN_POINT('Ctrl Pts',(-2.49947934768524,-2.03439496349108,
39.8282272707966));
#23412=CARTESIAN_POINT('Ctrl Pts',(-2.48797711888578,-2.04846860672115,
39.8293481021728));
#23413=CARTESIAN_POINT('Ctrl Pts',(-2.48054221281182,-2.0574654594896,39.8300643144918));
#23414=CARTESIAN_POINT('Ctrl Pts',(-2.4369403243924,-2.10964745583943,39.834217938609));
#23415=CARTESIAN_POINT('Ctrl Pts',(-2.39969252699148,-2.15192174664676,
39.8375812376748));
#23416=CARTESIAN_POINT('Ctrl Pts',(-2.18855363647068,-2.37924862519077,
39.8557986074645));
#23417=CARTESIAN_POINT('Ctrl Pts',(-1.99435678089185,-2.54424040897939,
39.869578214336));
#23418=CARTESIAN_POINT('Ctrl Pts',(-1.68364917784115,-2.75056444302925,
39.8906452045811));
#23419=CARTESIAN_POINT('Ctrl Pts',(-1.58098051405214,-2.81082891809792,
39.8974610527913));
#23420=CARTESIAN_POINT('Ctrl Pts',(-1.47525529542902,-2.86526427678297,
39.904468116039));
#23421=CARTESIAN_POINT('Origin',(0.,0.,4.68922655072688));
#23422=CARTESIAN_POINT('',(-1.47525540501187,-2.86526422036141,41.4036966894132));
#23423=CARTESIAN_POINT('',(-1.47525540498233,-2.86526422037662,41.155741540048));
#23424=CARTESIAN_POINT('',(-1.47525540501186,-2.86526422036142,4.68922655072688));
#23425=CARTESIAN_POINT('',(3.22274859133547,0.00301322837664063,40.5607734493322));
#23426=CARTESIAN_POINT('Ctrl Pts',(3.22274859133547,0.00301322837664063,
40.5607734493322));
#23427=CARTESIAN_POINT('Ctrl Pts',(3.22262419112213,0.136063419793571,40.5689887246145));
#23428=CARTESIAN_POINT('Ctrl Pts',(3.21425677216936,0.26874543348901,40.5772039998969));
#23429=CARTESIAN_POINT('Ctrl Pts',(3.19780408718992,0.400208173893808,40.5854192751792));
#23430=CARTESIAN_POINT('Ctrl Pts',(3.18308417976128,0.51782541214356,40.5927693272715));
#23431=CARTESIAN_POINT('Ctrl Pts',(3.16189309846113,0.634467395283658,40.6001193793638));
#23432=CARTESIAN_POINT('Ctrl Pts',(3.13437478364467,0.749541378545861,40.607469431456));
#23433=CARTESIAN_POINT('Ctrl Pts',(3.11126200858287,0.846192612763652,40.6136427782556));
#23434=CARTESIAN_POINT('Ctrl Pts',(3.08363389295753,0.941943832720015,40.6198161250552));
#23435=CARTESIAN_POINT('Ctrl Pts',(3.05157570653629,1.03634129020201,40.6259894718547));
#23436=CARTESIAN_POINT('Ctrl Pts',(3.01956099498361,1.13061073304826,40.6321544468319));
#23437=CARTESIAN_POINT('Ctrl Pts',(2.98312829213254,1.22352965490198,40.6383194218092));
#23438=CARTESIAN_POINT('Ctrl Pts',(2.94241358377365,1.31465579697666,40.6444843967864));
#23439=CARTESIAN_POINT('Ctrl Pts',(2.90174207079912,1.40568526075273,40.6506428311675));
#23440=CARTESIAN_POINT('Ctrl Pts',(2.85679776024314,1.49492533189045,40.6568012655486));
#23441=CARTESIAN_POINT('Ctrl Pts',(2.80776570451632,1.58195110892909,40.6629596999297));
#23442=CARTESIAN_POINT('Ctrl Pts',(2.75876964160129,1.66891300322067,40.6691136136077));
#23443=CARTESIAN_POINT('Ctrl Pts',(2.70569201198593,1.75366345796182,40.6752675272856));
#23444=CARTESIAN_POINT('Ctrl Pts',(2.64876461986577,1.83580052049436,40.6814214409636));
#23445=CARTESIAN_POINT('Ctrl Pts',(2.59185893121694,1.91790626841163,40.6875730084724));
#23446=CARTESIAN_POINT('Ctrl Pts',(2.53110664350499,1.99740024740105,40.6937245759812));
#23447=CARTESIAN_POINT('Ctrl Pts',(2.46678337926716,2.07390870634927,40.69987614349));
#23448=CARTESIAN_POINT('Ctrl Pts',(2.40246744708781,2.15040844427716,40.7060270097961));
#23449=CARTESIAN_POINT('Ctrl Pts',(2.33458162708301,2.2239230063942,40.7121778761021));
#23450=CARTESIAN_POINT('Ctrl Pts',(2.26344175423213,2.29411180802039,40.7183287424081));
#23451=CARTESIAN_POINT('Ctrl Pts',(2.19229097773184,2.36431136752475,40.724480551461));
#23452=CARTESIAN_POINT('Ctrl Pts',(2.11788546687482,2.43118384907181,40.7306323605138));
#23453=CARTESIAN_POINT('Ctrl Pts',(2.04057708960769,2.49442632760885,40.7367841695667));
#23454=CARTESIAN_POINT('Ctrl Pts',(1.96318636876915,2.55773616768849,40.7429425311039));
#23455=CARTESIAN_POINT('Ctrl Pts',(1.88288694393398,2.61740800834537,40.749100892641));
#23456=CARTESIAN_POINT('Ctrl Pts',(1.80006277528914,2.67318004771814,40.7552592541782));
#23457=CARTESIAN_POINT('Ctrl Pts',(1.71719262056847,2.72898305313952,40.7614210349936));
#23458=CARTESIAN_POINT('Ctrl Pts',(1.63179530139903,2.78088171955104,40.767582815809));
#23459=CARTESIAN_POINT('Ctrl Pts',(1.54428088665247,2.82865941845601,40.7737445966245));
#23460=CARTESIAN_POINT('Ctrl Pts',(1.45662043951921,2.87651684241452,40.7799166593981));
#23461=CARTESIAN_POINT('Ctrl Pts',(1.3668362307995,2.92023937284788,40.7860887221718));
#23462=CARTESIAN_POINT('Ctrl Pts',(1.27536000463379,2.95965782162069,40.7922607849455));
#23463=CARTESIAN_POINT('Ctrl Pts',(1.20549579749648,2.98976333411861,40.7969746465701));
#23464=CARTESIAN_POINT('Ctrl Pts',(1.13464508386649,3.01735925009222,40.8016885081947));
#23465=CARTESIAN_POINT('Ctrl Pts',(1.06300562506833,3.04238994929531,40.8064023698193));
#23466=CARTESIAN_POINT('Ctrl Pts',(0.969183155822521,3.07517135280645,40.8125758689596));
#23467=CARTESIAN_POINT('Ctrl Pts',(0.873678323558671,3.103666182483,40.8187493680999));
#23468=CARTESIAN_POINT('Ctrl Pts',(0.776919112435889,3.12770111347485,40.8249228672402));
#23469=CARTESIAN_POINT('Ctrl Pts',(0.680290719135704,3.1517035493967,40.83108801985));
#23470=CARTESIAN_POINT('Ctrl Pts',(0.582411735498871,3.17125796782599,40.8372531724597));
#23471=CARTESIAN_POINT('Ctrl Pts',(0.483727864759985,3.18623993373926,40.8434183250694));
#23472=CARTESIAN_POINT('Ctrl Pts',(0.385148292245413,3.20120606532793,40.8495769617767));
#23473=CARTESIAN_POINT('Ctrl Pts',(0.285765950771235,3.21160928734603,40.855735598484));
#23474=CARTESIAN_POINT('Ctrl Pts',(0.186038433928137,3.21737583499372,40.8618942351914));
#23475=CARTESIAN_POINT('Ctrl Pts',(0.0863835406774207,3.22313818332493,
40.868048387055));
#23476=CARTESIAN_POINT('Ctrl Pts',(-0.0136155960424126,3.22427054543994,
40.8742025389187));
#23477=CARTESIAN_POINT('Ctrl Pts',(-0.113495445003531,3.2207508979217,40.8803566907824));
#23478=CARTESIAN_POINT('Ctrl Pts',(-0.213337571237968,3.21723257970765,
40.8865085183395));
#23479=CARTESIAN_POINT('Ctrl Pts',(-0.313060065815396,3.20906575827465,
40.8926603458966));
#23480=CARTESIAN_POINT('Ctrl Pts',(-0.412199467256615,3.19628051986889,
40.8988121734537));
#23481=CARTESIAN_POINT('Ctrl Pts',(-0.511327913499578,3.18349669426994,
40.9049633212156));
#23482=CARTESIAN_POINT('Ctrl Pts',(-0.609872964109097,3.16609552188737,
40.9111144689774));
#23483=CARTESIAN_POINT('Ctrl Pts',(-0.707377352625077,3.14415884514335,
40.9172656167393));
#23484=CARTESIAN_POINT('Ctrl Pts',(-0.804897017418076,3.12221873152068,
40.9234177282182));
#23485=CARTESIAN_POINT('Ctrl Pts',(-0.901375272646106,3.09574179739957,
40.9295698396971));
#23486=CARTESIAN_POINT('Ctrl Pts',(-0.99636708492585,3.06486055059221,40.935721951176));
#23487=CARTESIAN_POINT('Ctrl Pts',(-1.09146053909923,3.03394626063799,40.9418806454566));
#23488=CARTESIAN_POINT('Ctrl Pts',(-1.18506396053084,2.99861838176978,40.9480393397371));
#23489=CARTESIAN_POINT('Ctrl Pts',(-1.27674958943304,2.95905864226828,40.9541980340177));
#23490=CARTESIAN_POINT('Ctrl Pts',(-1.36848637968764,2.91947682809927,40.9603601649015));
#23491=CARTESIAN_POINT('Ctrl Pts',(-1.45830285597916,2.87565864088038,40.9665222957853));
#23492=CARTESIAN_POINT('Ctrl Pts',(-1.54579517455693,2.82783218045493,40.972684426669));
#23493=CARTESIAN_POINT('Ctrl Pts',(-1.63343382772084,2.779925728261,40.9788568639762));
#23494=CARTESIAN_POINT('Ctrl Pts',(-1.71874018738417,2.72799783754466,40.9850293012833));
#23495=CARTESIAN_POINT('Ctrl Pts',(-1.8013386261253,2.67232047414396,40.9912017385904));
#23496=CARTESIAN_POINT('Ctrl Pts',(-1.86438291609249,2.62982403115618,40.9959129284546));
#23497=CARTESIAN_POINT('Ctrl Pts',(-1.92585023631551,2.58514416715511,41.0006241183187));
#23498=CARTESIAN_POINT('Ctrl Pts',(-1.98558722752699,2.53841701152149,41.0053353081829));
#23499=CARTESIAN_POINT('Ctrl Pts',(-2.06373736416863,2.47728682194238,41.0114986606411));
#23500=CARTESIAN_POINT('Ctrl Pts',(-2.13920186822442,2.41243469483613,41.0176620130993));
#23501=CARTESIAN_POINT('Ctrl Pts',(-2.21160414709847,2.34412556383758,41.0238253655576));
#23502=CARTESIAN_POINT('Ctrl Pts',(-2.28390791960727,2.27590937030333,41.0299803325139));
#23503=CARTESIAN_POINT('Ctrl Pts',(-2.35315743316449,2.20424581702229,41.0361352994702));
#23504=CARTESIAN_POINT('Ctrl Pts',(-2.41900756135291,2.12944123671386,41.0422902664265));
#23505=CARTESIAN_POINT('Ctrl Pts',(-2.48478770214377,2.05471616085053,41.048438691708));
#23506=CARTESIAN_POINT('Ctrl Pts',(-2.54717535364372,1.97685701969955,41.0545871169896));
#23507=CARTESIAN_POINT('Ctrl Pts',(-2.60586152789159,1.89620759938213,41.0607355422712));
#23508=CARTESIAN_POINT('Ctrl Pts',(-2.66450491757013,1.81561697571927,41.0668794851047));
#23509=CARTESIAN_POINT('Ctrl Pts',(-2.71945193898403,1.73224046813409,41.0730234279382));
#23510=CARTESIAN_POINT('Ctrl Pts',(-2.77043388081351,1.64645488080926,41.0791673707717));
#23511=CARTESIAN_POINT('Ctrl Pts',(-2.82139657140941,1.56070168688334,41.0853089935979));
#23512=CARTESIAN_POINT('Ctrl Pts',(-2.86839693478945,1.47254159477363,41.0914506164241));
#23513=CARTESIAN_POINT('Ctrl Pts',(-2.91121011325736,1.38237955676726,41.0975922392503));
#23514=CARTESIAN_POINT('Ctrl Pts',(-2.95401866372039,1.29222726506722,41.1037331981813));
#23515=CARTESIAN_POINT('Ctrl Pts',(-2.9926407421395,1.20007385130773,41.1098741571124));
#23516=CARTESIAN_POINT('Ctrl Pts',(-3.02689837238441,1.10634705484158,41.1160151160435));
#23517=CARTESIAN_POINT('Ctrl Pts',(-3.06116153227586,1.01260512959821,41.1221570662087));
#23518=CARTESIAN_POINT('Ctrl Pts',(-3.09105869515395,0.917289726540066,
41.1282990163739));
#23519=CARTESIAN_POINT('Ctrl Pts',(-3.11646112231233,0.820845683192496,
41.1344409665391));
#23520=CARTESIAN_POINT('Ctrl Pts',(-3.14189120989953,0.724296622966874,
41.1405896046075));
#23521=CARTESIAN_POINT('Ctrl Pts',(-3.16281667734122,0.626616890588295,
41.146738242676));
#23522=CARTESIAN_POINT('Ctrl Pts',(-3.17915953521806,0.528263392761672,
41.1528868807444));
#23523=CARTESIAN_POINT('Ctrl Pts',(-3.19551163962405,0.429854248089751,
41.1590389976145));
#23524=CARTESIAN_POINT('Ctrl Pts',(-3.20727592026887,0.330771011595257,
41.1651911144846));
#23525=CARTESIAN_POINT('Ctrl Pts',(-3.21442633426897,0.231475493428943,
41.1713432313547));
#23526=CARTESIAN_POINT('Ctrl Pts',(-3.22158892941005,0.132010819643656,
41.1775058287093));
#23527=CARTESIAN_POINT('Ctrl Pts',(-3.22412194700544,0.0323335776409921,
41.1836684260639));
#23528=CARTESIAN_POINT('Ctrl Pts',(-3.22205150365813,-0.0670944876602563,
41.1898310234185));
#23529=CARTESIAN_POINT('Ctrl Pts',(-3.22043468254313,-0.144738435567149,
41.1946434311278));
#23530=CARTESIAN_POINT('Ctrl Pts',(-3.21601166693476,-0.222230416598312,
41.199455838837));
#23531=CARTESIAN_POINT('Ctrl Pts',(-3.20881670658963,-0.299354148144459,
41.2042682465462));
#23532=CARTESIAN_POINT('Ctrl Pts',(-3.19957127567767,-0.398457144891972,
41.2104521281608));
#23533=CARTESIAN_POINT('Ctrl Pts',(-3.18571439893586,-0.497303199742479,
41.2166360097754));
#23534=CARTESIAN_POINT('Ctrl Pts',(-3.16726709666734,-0.595429845463283,
41.22281989139));
#23535=CARTESIAN_POINT('Ctrl Pts',(-3.14884484621629,-0.693423233172627,
41.2289953751657));
#23536=CARTESIAN_POINT('Ctrl Pts',(-3.12584464111695,-0.790698732252656,
41.2351708589413));
#23537=CARTESIAN_POINT('Ctrl Pts',(-3.09833932604596,-0.886798163719958,
41.241346342717));
#23538=CARTESIAN_POINT('Ctrl Pts',(-3.07086331758082,-0.982795202316867,
41.2475152465836));
#23539=CARTESIAN_POINT('Ctrl Pts',(-3.03889186148929,-1.07761825109776,
41.2536841504503));
#23540=CARTESIAN_POINT('Ctrl Pts',(-3.00254881755478,-1.17081943983708,
41.259853054317));
#23541=CARTESIAN_POINT('Ctrl Pts',(-2.96623300370973,-1.26395079742213,
41.2660173361217));
#23542=CARTESIAN_POINT('Ctrl Pts',(-2.92555227186591,-1.35546230948821,
41.2721816179263));
#23543=CARTESIAN_POINT('Ctrl Pts',(-2.88067999071116,-1.44492226559645,
41.2783458997309));
#23544=CARTESIAN_POINT('Ctrl Pts',(-2.83582526615847,-1.53434721985476,
41.2845077697161));
#23545=CARTESIAN_POINT('Ctrl Pts',(-2.78678244504761,-1.62172182701643,
41.2906696397012));
#23546=CARTESIAN_POINT('Ctrl Pts',(-2.73377225069178,-1.70663611934343,
41.2968315096864));
#23547=CARTESIAN_POINT('Ctrl Pts',(-2.6807687561129,-1.79153967964379,41.3029926008939));
#23548=CARTESIAN_POINT('Ctrl Pts',(-2.62379911439302,-1.87398317641695,
41.3091536921013));
#23549=CARTESIAN_POINT('Ctrl Pts',(-2.5631285449393,-1.95358379001704,41.3153147833088));
#23550=CARTESIAN_POINT('Ctrl Pts',(-2.50244957388124,-2.03319542663648,
41.3214767276985));
#23551=CARTESIAN_POINT('Ctrl Pts',(-2.43806891945372,-2.10996305405005,
41.3276386720882));
#23552=CARTESIAN_POINT('Ctrl Pts',(-2.3702928086302,-2.18353602302686,41.333800616478));
#23553=CARTESIAN_POINT('Ctrl Pts',(-2.30244683475877,-2.25718483040446,
41.3399689125484));
#23554=CARTESIAN_POINT('Ctrl Pts',(-2.23119870873185,-2.32763208442139,
41.3461372086188));
#23555=CARTESIAN_POINT('Ctrl Pts',(-2.15689225476011,-2.39456329293168,
41.3523055046892));
#23556=CARTESIAN_POINT('Ctrl Pts',(-2.08254577089664,-2.46153055818924,
41.3584771237041));
#23557=CARTESIAN_POINT('Ctrl Pts',(-2.00513801200696,-2.52497773072402,
41.3646487427191));
#23558=CARTESIAN_POINT('Ctrl Pts',(-1.92504508718016,-2.58463130345965,
41.370820361734));
#23559=CARTESIAN_POINT('Ctrl Pts',(-1.8448220891684,-2.64438175529187,41.3770020036335));
#23560=CARTESIAN_POINT('Ctrl Pts',(-1.76190557312126,-2.70032605835056,
41.3831836455331));
#23561=CARTESIAN_POINT('Ctrl Pts',(-1.67669985950868,-2.75223457278328,
41.3893652874326));
#23562=CARTESIAN_POINT('Ctrl Pts',(-1.61313004331406,-2.79096219539821,
41.3939772532583));
#23563=CARTESIAN_POINT('Ctrl Pts',(-1.54828657774929,-2.8274443124284,41.398589219084));
#23564=CARTESIAN_POINT('Ctrl Pts',(-1.48234495845957,-2.86160287018124,
41.4032011849096));
#23565=CARTESIAN_POINT('Ctrl Pts',(-1.47998339359638,-2.86282618939352,
41.4033663530775));
#23566=CARTESIAN_POINT('Ctrl Pts',(-1.47762020665672,-2.8640466410598,41.4035315212454));
#23567=CARTESIAN_POINT('Ctrl Pts',(-1.47525540501187,-2.86526422036141,
41.4036966894132));
#23568=CARTESIAN_POINT('Ctrl Pts',(3.22274859312508,0.00301131371402447,
40.5608077201065));
#23569=CARTESIAN_POINT('Ctrl Pts',(3.2229238947785,-0.184598882557479,40.5503261789538));
#23570=CARTESIAN_POINT('Ctrl Pts',(3.20671723420002,-0.371855052433079,
40.5398166588107));
#23571=CARTESIAN_POINT('Ctrl Pts',(3.16427968097729,-0.613862529188434,
40.5254059762392));
#23572=CARTESIAN_POINT('Ctrl Pts',(3.15269954516447,-0.670804038967186,
40.5219562899646));
#23573=CARTESIAN_POINT('Ctrl Pts',(3.13594431233552,-0.743122694444961,
40.5174858727603));
#23574=CARTESIAN_POINT('Ctrl Pts',(3.13218332582174,-0.758818600182063,
40.5165102250996));
#23575=CARTESIAN_POINT('Ctrl Pts',(3.12563446067714,-0.785270804289436,
40.5148565483237));
#23576=CARTESIAN_POINT('Ctrl Pts',(3.12290854167766,-0.796042243429977,
40.5141805149489));
#23577=CARTESIAN_POINT('Ctrl Pts',(3.11740830733502,-0.817313246518816,
40.5128401633219));
#23578=CARTESIAN_POINT('Ctrl Pts',(3.114636513304,-0.827813314099862,40.512175934349));
#23579=CARTESIAN_POINT('Ctrl Pts',(3.10919338784129,-0.848018491750633,
40.51089268907));
#23580=CARTESIAN_POINT('Ctrl Pts',(3.1065295497782,-0.857725502727836,40.5102739235535));
#23581=CARTESIAN_POINT('Ctrl Pts',(3.10031003975935,-0.879980288415187,
40.508850029205));
#23582=CARTESIAN_POINT('Ctrl Pts',(3.09672360645326,-0.892519214259733,
40.5080439027508));
#23583=CARTESIAN_POINT('Ctrl Pts',(3.08695511710534,-0.925904117693024,
40.5058870977307));
#23584=CARTESIAN_POINT('Ctrl Pts',(3.08063811984657,-0.946709600284812,
40.5045320180866));
#23585=CARTESIAN_POINT('Ctrl Pts',(3.02709939589663,-1.11683119106082,40.4933598813228));
#23586=CARTESIAN_POINT('Ctrl Pts',(2.9692690942477,-1.26256516297879,40.4831901049873));
#23587=CARTESIAN_POINT('Ctrl Pts',(2.8788886727882,-1.4493845179116,40.4693751701246));
#23588=CARTESIAN_POINT('Ctrl Pts',(2.85560670142801,-1.49473260860151,40.4659589530262));
#23589=CARTESIAN_POINT('Ctrl Pts',(2.82894744290142,-1.54376078382435,40.4622016806355));
#23590=CARTESIAN_POINT('Ctrl Pts',(2.82662558960878,-1.54800800010078,40.4618756644591));
#23591=CARTESIAN_POINT('Ctrl Pts',(2.77067316662324,-1.64981254609223,40.4540485249987));
#23592=CARTESIAN_POINT('Ctrl Pts',(2.71203355215114,-1.74452998818334,40.4464840362029));
#23593=CARTESIAN_POINT('Ctrl Pts',(2.57377279054074,-1.94398231964742,40.4301162172918));
#23594=CARTESIAN_POINT('Ctrl Pts',(2.49239564248336,-2.04727740802169,40.4213489548755));
#23595=CARTESIAN_POINT('Ctrl Pts',(2.38857458465351,-2.16366189942263,40.4113634291883));
#23596=CARTESIAN_POINT('Ctrl Pts',(2.37200747121731,-2.18181163351335,40.4098030536497));
#23597=CARTESIAN_POINT('Ctrl Pts',(2.35062176127878,-2.20470872284533,40.4078324829267));
#23598=CARTESIAN_POINT('Ctrl Pts',(2.34599414962127,-2.20963224747159,40.4074086314184));
#23599=CARTESIAN_POINT('Ctrl Pts',(2.3369450838761,-2.21919948386372,40.4065848420951));
#23600=CARTESIAN_POINT('Ctrl Pts',(2.33252519119706,-2.22384462325253,40.406184790299));
#23601=CARTESIAN_POINT('Ctrl Pts',(2.32422418162256,-2.23251669513297,40.4054378305655));
#23602=CARTESIAN_POINT('Ctrl Pts',(2.32034649208245,-2.23654666789858,40.4050906798753));
#23603=CARTESIAN_POINT('Ctrl Pts',(2.31144910298076,-2.24574542598431,40.4042981699123));
#23604=CARTESIAN_POINT('Ctrl Pts',(2.30642255426454,-2.25090747867538,40.4038533540029));
#23605=CARTESIAN_POINT('Ctrl Pts',(2.29084613036601,-2.26679684598253,40.402483733832));
#23606=CARTESIAN_POINT('Ctrl Pts',(2.28023823420157,-2.27746735423769,40.4015633590956));
#23607=CARTESIAN_POINT('Ctrl Pts',(2.16157901497012,-2.39516676427382,40.3913990751255));
#23608=CARTESIAN_POINT('Ctrl Pts',(2.04614058331038,-2.4945077582227,40.3827028048404));
#23609=CARTESIAN_POINT('Ctrl Pts',(1.76139459026686,-2.70642641181927,40.3627219482727));
#23610=CARTESIAN_POINT('Ctrl Pts',(1.58762445738144,-2.81188593057071,40.3515638285195));
#23611=CARTESIAN_POINT('Ctrl Pts',(1.3348199865055,-2.93436040257996,40.3354579954833));
#23612=CARTESIAN_POINT('Ctrl Pts',(1.26333425012722,-2.96583894780112,40.3309210088079));
#23613=CARTESIAN_POINT('Ctrl Pts',(1.1446522514414,-3.01303051967691,40.3233636247056));
#23614=CARTESIAN_POINT('Ctrl Pts',(1.09810952530253,-3.03030307985393,40.3203940283747));
#23615=CARTESIAN_POINT('Ctrl Pts',(1.03621933884947,-3.0516582034835,40.3164297265227));
#23616=CARTESIAN_POINT('Ctrl Pts',(1.02121274523473,-3.056712748057,40.315467326557));
#23617=CARTESIAN_POINT('Ctrl Pts',(0.995847650001017,-3.06504862482765,
40.3138383924981));
#23618=CARTESIAN_POINT('Ctrl Pts',(0.985508596637388,-3.06838856990994,
40.3131738042492));
#23619=CARTESIAN_POINT('Ctrl Pts',(0.965541957742636,-3.0747273002856,40.3118890843201));
#23620=CARTESIAN_POINT('Ctrl Pts',(0.955916786186559,-3.07773331162445,
40.3112691996256));
#23621=CARTESIAN_POINT('Ctrl Pts',(0.933771423142863,-3.08453556587378,
40.3098416058582));
#23622=CARTESIAN_POINT('Ctrl Pts',(0.921241969045974,-3.08830081989703,
40.3090328900427));
#23623=CARTESIAN_POINT('Ctrl Pts',(0.88772424444445,-3.09815118407498,40.3068666329172));
#23624=CARTESIAN_POINT('Ctrl Pts',(0.866696709727775,-3.10409920410611,
40.3055046432148));
#23625=CARTESIAN_POINT('Ctrl Pts',(0.690332581046362,-3.15205528645061,
40.2940545449546));
#23626=CARTESIAN_POINT('Ctrl Pts',(0.532134429685544,-3.18258238173379,
40.2835937515043));
#23627=CARTESIAN_POINT('Ctrl Pts',(0.121474423938302,-3.2303476369322,40.2560428507455));
#23628=CARTESIAN_POINT('Ctrl Pts',(-0.131935317308873,-3.22993636240842,
40.2386162665552));
#23629=CARTESIAN_POINT('Ctrl Pts',(-0.442326483535104,-3.19281568102752,
40.2181240203984));
#23630=CARTESIAN_POINT('Ctrl Pts',(-0.501754566968227,-3.18401760979885,
40.2142446132021));
#23631=CARTESIAN_POINT('Ctrl Pts',(-0.572621039016476,-3.1714924296507,
40.2096985134214));
#23632=CARTESIAN_POINT('Ctrl Pts',(-0.584324483269368,-3.16935703168332,
40.2089503718798));
#23633=CARTESIAN_POINT('Ctrl Pts',(-0.602486847658238,-3.16593912054356,
40.2077937293167));
#23634=CARTESIAN_POINT('Ctrl Pts',(-0.608953969538599,-3.16470156277189,
40.2073827460243));
#23635=CARTESIAN_POINT('Ctrl Pts',(-0.620893496299887,-3.16237884387466,
40.2066256509544));
#23636=CARTESIAN_POINT('Ctrl Pts',(-0.626366835800287,-3.16129930152288,
40.2062792327385));
#23637=CARTESIAN_POINT('Ctrl Pts',(-0.638684432494127,-3.15883657585578,
40.2055010772227));
#23638=CARTESIAN_POINT('Ctrl Pts',(-0.645526993645605,-3.15744536293488,
40.2050698045064));
#23639=CARTESIAN_POINT('Ctrl Pts',(-0.663055734370697,-3.15382209858,40.2039674463562));
#23640=CARTESIAN_POINT('Ctrl Pts',(-0.673735293444924,-3.15155794784685,
40.203298154434));
#23641=CARTESIAN_POINT('Ctrl Pts',(-0.736832483135688,-3.13784545457574,
40.1993565220328));
#23642=CARTESIAN_POINT('Ctrl Pts',(-0.788972514573263,-3.12514309308663,
40.1961512341744));
#23643=CARTESIAN_POINT('Ctrl Pts',(-0.86821343675468,-3.10372854417498,
40.1913258912345));
#23644=CARTESIAN_POINT('Ctrl Pts',(-0.895553884671158,-3.09595038304072,
40.1896694958894));
#23645=CARTESIAN_POINT('Ctrl Pts',(-1.01915676344838,-3.05901181679438,
40.1822051765307));
#23646=CARTESIAN_POINT('Ctrl Pts',(-1.11412936226403,-3.02571508266372,
40.1765352057574));
#23647=CARTESIAN_POINT('Ctrl Pts',(-1.29853395032025,-2.95120144988354,
40.1653921006252));
#23648=CARTESIAN_POINT('Ctrl Pts',(-1.38791377808792,-2.91023432009513,
40.1599247739091));
#23649=CARTESIAN_POINT('Ctrl Pts',(-1.47525550050006,-2.86526417119684,
40.1544081509837));
#23650=CARTESIAN_POINT('',(3.22274996944047,-0.000443814660293801,40.3112149259812));
#23651=CARTESIAN_POINT('Ctrl Pts',(-1.47525529542902,-2.86526427678297,
39.904468116039));
#23652=CARTESIAN_POINT('Ctrl Pts',(-1.4354344117846,-2.88576708692202,39.907107291951));
#23653=CARTESIAN_POINT('Ctrl Pts',(-1.39517988412917,-2.90544297473476,
39.9097730047258));
#23654=CARTESIAN_POINT('Ctrl Pts',(-1.33459234943844,-2.9335069438397,39.9137889337923));
#23655=CARTESIAN_POINT('Ctrl Pts',(-1.31457429940772,-2.94253192056124,
39.9151163693994));
#23656=CARTESIAN_POINT('Ctrl Pts',(-1.28246107940106,-2.956616813754,39.9172474830041));
#23657=CARTESIAN_POINT('Ctrl Pts',(-1.27042432850135,-2.96180880901089,
39.9180466313052));
#23658=CARTESIAN_POINT('Ctrl Pts',(-1.24907510149167,-2.970863610293,39.9194648354831));
#23659=CARTESIAN_POINT('Ctrl Pts',(-1.23977549368212,-2.97475644746363,
39.9200828570189));
#23660=CARTESIAN_POINT('Ctrl Pts',(-1.22043800308202,-2.98274473823459,
39.9213685701654));
#23661=CARTESIAN_POINT('Ctrl Pts',(-1.2103974272437,-2.98683329905711,39.9220364865195));
#23662=CARTESIAN_POINT('Ctrl Pts',(-1.1844299082303,-2.99725493218915,39.9237648559926));
#23663=CARTESIAN_POINT('Ctrl Pts',(-1.16847288555892,-3.00351168359012,
39.9248278723957));
#23664=CARTESIAN_POINT('Ctrl Pts',(-1.10035602627271,-3.02959533807511,
39.9293701413526));
#23665=CARTESIAN_POINT('Ctrl Pts',(-1.04773846536925,-3.04819205055329,
39.9328902629578));
#23666=CARTESIAN_POINT('Ctrl Pts',(-0.907866804382616,-3.09357770389227,
39.942283470876));
#23667=CARTESIAN_POINT('Ctrl Pts',(-0.819916423488113,-3.11804100876193,
39.9482270134279));
#23668=CARTESIAN_POINT('Ctrl Pts',(-0.489238441873115,-3.19506019930173,
39.9706807439011));
#23669=CARTESIAN_POINT('Ctrl Pts',(-0.241751965264356,-3.2232443358107,
39.9877734806567));
#23670=CARTESIAN_POINT('Ctrl Pts',(0.0943292490012712,-3.22256623450963,
40.0100979881635));
#23671=CARTESIAN_POINT('Ctrl Pts',(0.18212114491343,-3.21879885323879,40.0158380748646));
#23672=CARTESIAN_POINT('Ctrl Pts',(0.283388872142236,-3.21029565534206,
40.0222739267102));
#23673=CARTESIAN_POINT('Ctrl Pts',(0.2971131830738,-3.20905456793451,40.0231421733362));
#23674=CARTESIAN_POINT('Ctrl Pts',(0.317839679711471,-3.20704616524514,
40.0244469671753));
#23675=CARTESIAN_POINT('Ctrl Pts',(0.324847796302325,-3.20634388041727,
40.0248870356005));
#23676=CARTESIAN_POINT('Ctrl Pts',(0.33740301201393,-3.20504413317905,40.0256733651343));
#23677=CARTESIAN_POINT('Ctrl Pts',(0.342950889905818,-3.20445523869221,
40.0260201000121));
#23678=CARTESIAN_POINT('Ctrl Pts',(0.354987248919614,-3.20314598992632,
40.0267707701308));
#23679=CARTESIAN_POINT('Ctrl Pts',(0.361475059145022,-3.2024203289196,40.027174402342));
#23680=CARTESIAN_POINT('Ctrl Pts',(0.379659965633833,-3.20033038200326,
40.0283030861608));
#23681=CARTESIAN_POINT('Ctrl Pts',(0.391351996466248,-3.19892167273746,
40.0290256756629));
#23682=CARTESIAN_POINT('Ctrl Pts',(0.460668858059748,-3.19018432957703,
40.0332925773403));
#23683=CARTESIAN_POINT('Ctrl Pts',(0.518098742550746,-3.18136236880429,
40.0367579873582));
#23684=CARTESIAN_POINT('Ctrl Pts',(0.8238959272466,-3.12588644084873,40.054985652752));
#23685=CARTESIAN_POINT('Ctrl Pts',(1.06638357635951,-3.05169180061492,40.0687017116454));
#23686=CARTESIAN_POINT('Ctrl Pts',(1.44700665821806,-2.88424778755483,40.0921939520004));
#23687=CARTESIAN_POINT('Ctrl Pts',(1.59106414428608,-2.8073507326046,40.1015935547739));
#23688=CARTESIAN_POINT('Ctrl Pts',(1.74882749913779,-2.70708148875967,40.1128365923115));
#23689=CARTESIAN_POINT('Ctrl Pts',(1.76883783116284,-2.69404908799061,40.1142808564639));
#23690=CARTESIAN_POINT('Ctrl Pts',(1.79915210180886,-2.67382256825838,40.1164976866093));
#23691=CARTESIAN_POINT('Ctrl Pts',(1.80956213660343,-2.66678838281437,40.1172642282786));
#23692=CARTESIAN_POINT('Ctrl Pts',(1.8279854189055,-2.65418200720913,40.1186303575));
#23693=CARTESIAN_POINT('Ctrl Pts',(1.83601502811607,-2.64863391814042,40.119229022317));
#23694=CARTESIAN_POINT('Ctrl Pts',(1.84419128288443,-2.64292945774922,40.1198419819224));
#23695=CARTESIAN_POINT('Ctrl Pts',(1.84436331220659,-2.6428094102842,40.1198548801868));
#23696=CARTESIAN_POINT('Ctrl Pts',(1.84469492315573,-2.64257795360169,40.119879746363));
#23697=CARTESIAN_POINT('Ctrl Pts',(1.84485451146287,-2.64246654319754,40.1198917145635));
#23698=CARTESIAN_POINT('Ctrl Pts',(1.84516256000937,-2.64225144950816,40.1199148189596));
#23699=CARTESIAN_POINT('Ctrl Pts',(1.84531101617009,-2.6421477719631,40.1199259546724));
#23700=CARTESIAN_POINT('Ctrl Pts',(1.84559791493642,-2.64194737407912,40.119947477178));
#23701=CARTESIAN_POINT('Ctrl Pts',(1.84573635868543,-2.64185065536412,40.1199578639086));
#23702=CARTESIAN_POINT('Ctrl Pts',(1.84600420383836,-2.64166350371011,40.1199779608828));
#23703=CARTESIAN_POINT('Ctrl Pts',(1.84613360619568,-2.64157307214807,40.1199876710731));
#23704=CARTESIAN_POINT('Ctrl Pts',(1.84638421423636,-2.64139790977976,40.1200064780607));
#23705=CARTESIAN_POINT('Ctrl Pts',(1.84650542074391,-2.64131318013095,40.1200155748138));
#23706=CARTESIAN_POINT('Ctrl Pts',(1.84674037741264,-2.64114890913022,40.1200332101801));
#23707=CARTESIAN_POINT('Ctrl Pts',(1.8468541282786,-2.64106936876452,40.1200417487558));
#23708=CARTESIAN_POINT('Ctrl Pts',(1.84707482495552,-2.64091502524191,40.1200583163914));
#23709=CARTESIAN_POINT('Ctrl Pts',(1.84718177136025,-2.64084022293802,40.1200663454183));
#23710=CARTESIAN_POINT('Ctrl Pts',(1.84738943469184,-2.64069495667296,40.120081936941));
#23711=CARTESIAN_POINT('Ctrl Pts',(1.84749015211488,-2.64062449345748,40.1200894994073));
#23712=CARTESIAN_POINT('Ctrl Pts',(1.84768586820412,-2.64048755126454,40.1201041959611));
#23713=CARTESIAN_POINT('Ctrl Pts',(1.84778086732807,-2.64042107291253,40.1201113300251));
#23714=CARTESIAN_POINT('Ctrl Pts',(1.84796560191936,-2.64029178475038,40.1201252037812));
#23715=CARTESIAN_POINT('Ctrl Pts',(1.84805533776569,-2.64022897549687,40.1201319434515));
#23716=CARTESIAN_POINT('Ctrl Pts',(1.84822995269071,-2.64010674314742,40.1201450588323));
#23717=CARTESIAN_POINT('Ctrl Pts',(1.84831483212035,-2.64004732052278,40.1201514345254));
#23718=CARTESIAN_POINT('Ctrl Pts',(1.84848009940399,-2.63993160787134,40.1201638492545));
#23719=CARTESIAN_POINT('Ctrl Pts',(1.84856048753421,-2.63987531827889,40.1201698882729));
#23720=CARTESIAN_POINT('Ctrl Pts',(1.84871710084741,-2.63976564342265,40.1201816542276));
#23721=CARTESIAN_POINT('Ctrl Pts',(1.84879332631048,-2.63971225851419,40.1201873811512));
#23722=CARTESIAN_POINT('Ctrl Pts',(1.84894191112628,-2.63960818675532,40.120198545119));
#23723=CARTESIAN_POINT('Ctrl Pts',(1.84901427069464,-2.63955750023988,40.1202039821497));
#23724=CARTESIAN_POINT('Ctrl Pts',(1.84915539244532,-2.63945863845969,40.1202145864359));
#23725=CARTESIAN_POINT('Ctrl Pts',(1.84922415483558,-2.63941046347887,40.1202197536808));
#23726=CARTESIAN_POINT('Ctrl Pts',(1.84935832619262,-2.63931645511126,40.1202298366511));
#23727=CARTESIAN_POINT('Ctrl Pts',(1.84942373536371,-2.63927062196213,40.1202347523686));
#23728=CARTESIAN_POINT('Ctrl Pts',(1.84955142247948,-2.63918114268188,40.1202443489145));
#23729=CARTESIAN_POINT('Ctrl Pts',(1.84961370055251,-2.63913749679928,40.1202490297319));
#23730=CARTESIAN_POINT('Ctrl Pts',(1.84973532810732,-2.63905225103722,40.1202581716465));
#23731=CARTESIAN_POINT('Ctrl Pts',(1.84979467772745,-2.63901065136238,40.1202626327357));
#23732=CARTESIAN_POINT('Ctrl Pts',(1.8499508514083,-2.63890117735688,40.1202743722087));
#23733=CARTESIAN_POINT('Ctrl Pts',(1.85004767312273,-2.63883329970936,40.1202816507196));
#23734=CARTESIAN_POINT('Ctrl Pts',(1.85987454831579,-2.63194328254921,40.1210204291846));
#23735=CARTESIAN_POINT('Ctrl Pts',(1.86956669129953,-2.6250674579411,40.1217539912025));
#23736=CARTESIAN_POINT('Ctrl Pts',(1.88961513268072,-2.61067729289508,40.1232817217677));
#23737=CARTESIAN_POINT('Ctrl Pts',(1.89996513577431,-2.60315457714655,40.1240762073053));
#23738=CARTESIAN_POINT('Ctrl Pts',(1.92652292712574,-2.58360875843707,40.1261299611862));
#23739=CARTESIAN_POINT('Ctrl Pts',(1.94266288720805,-2.5714948341689,40.1273927576013));
#23740=CARTESIAN_POINT('Ctrl Pts',(2.05084929511193,-2.48869517951676,40.1359580608007));
#23741=CARTESIAN_POINT('Ctrl Pts',(2.13912313870307,-2.41324126002501,40.1434487349545));
#23742=CARTESIAN_POINT('Ctrl Pts',(2.3442565878826,-2.21778516637936,40.1621230029332));
#23743=CARTESIAN_POINT('Ctrl Pts',(2.45620502737752,-2.09312174580871,40.1734576634612));
#23744=CARTESIAN_POINT('Ctrl Pts',(2.62171048559569,-1.877161427229,40.1918679186159));
#23745=CARTESIAN_POINT('Ctrl Pts',(2.68136706640819,-1.79091419996341,40.1989376278261));
#23746=CARTESIAN_POINT('Ctrl Pts',(2.77646025055787,-1.63800175924701,40.2108366087151));
#23747=CARTESIAN_POINT('Ctrl Pts',(2.8139561781881,-1.57271546174028,40.2157314151553));
#23748=CARTESIAN_POINT('Ctrl Pts',(2.8547842455235,-1.49548340334282,40.2212603561159));
#23749=CARTESIAN_POINT('Ctrl Pts',(2.86037387661069,-1.48476428935119,40.222022011679));
#23750=CARTESIAN_POINT('Ctrl Pts',(2.86922201243464,-1.46756098992165,40.2232349863979));
#23751=CARTESIAN_POINT('Ctrl Pts',(2.87251909826765,-1.46109693323464,40.2236886411033));
#23752=CARTESIAN_POINT('Ctrl Pts',(2.87832755210492,-1.44961359117345,40.2244907368085));
#23753=CARTESIAN_POINT('Ctrl Pts',(2.88084767429952,-1.44459881637653,40.2248397236261));
#23754=CARTESIAN_POINT('Ctrl Pts',(2.88617297060559,-1.43393268709669,40.2255792429951));
#23755=CARTESIAN_POINT('Ctrl Pts',(2.88897464815871,-1.42827968244749,40.2259695567574));
#23756=CARTESIAN_POINT('Ctrl Pts',(2.8965202531976,-1.41294171382675,40.227024264696));
#23757=CARTESIAN_POINT('Ctrl Pts',(2.90123224814389,-1.40324100349815,40.2276866907242));
#23758=CARTESIAN_POINT('Ctrl Pts',(2.92476807779917,-1.35416181830449,40.2310156858405));
#23759=CARTESIAN_POINT('Ctrl Pts',(2.94284028211441,-1.31442536880162,40.2336383264671));
#23760=CARTESIAN_POINT('Ctrl Pts',(2.99340659042261,-1.19696666549488,40.2412148326157));
#23761=CARTESIAN_POINT('Ctrl Pts',(3.02366914678196,-1.11831978125285,40.2460666869733));
#23762=CARTESIAN_POINT('Ctrl Pts',(3.15302723056023,-0.738329026262928,
40.2688664922471));
#23763=CARTESIAN_POINT('Ctrl Pts',(3.21035471649592,-0.424663076438896,
40.2859978879917));
#23764=CARTESIAN_POINT('Ctrl Pts',(3.2221453506905,-0.071937250536365,40.3069233384524));
#23765=CARTESIAN_POINT('Ctrl Pts',(3.22274504656494,-0.0361911623234127,
40.3090599752032));
#23766=CARTESIAN_POINT('Ctrl Pts',(3.22274996944047,-0.000443814660293801,
40.3112149259812));
#23767=CARTESIAN_POINT('Ctrl Pts',(-1.47525540498233,-2.86526422037662,
41.155741540048));
#23768=CARTESIAN_POINT('Ctrl Pts',(-1.6289715779912,-2.78611947224071,41.1441838822727));
#23769=CARTESIAN_POINT('Ctrl Pts',(-1.77608938213473,-2.69472340804177,
41.1329065881922));
#23770=CARTESIAN_POINT('Ctrl Pts',(-1.93294765727014,-2.57882119718988,
41.1206854600813));
#23771=CARTESIAN_POINT('Ctrl Pts',(-1.95057667855932,-2.56551282847913,
41.1193085513726));
#23772=CARTESIAN_POINT('Ctrl Pts',(-1.97848089032937,-2.54399368052792,
41.1171232728468));
#23773=CARTESIAN_POINT('Ctrl Pts',(-1.98884480585058,-2.53589960890422,
41.1163103308354));
#23774=CARTESIAN_POINT('Ctrl Pts',(-2.00707472009297,-2.52148180279603,
41.1148779535633));
#23775=CARTESIAN_POINT('Ctrl Pts',(-2.01496104506488,-2.51518416908886,
41.1142574885869));
#23776=CARTESIAN_POINT('Ctrl Pts',(-2.03125022220081,-2.50205064480447,
41.1129741619813));
#23777=CARTESIAN_POINT('Ctrl Pts',(-2.0396484637143,-2.49520921835311,41.1123115342925));
#23778=CARTESIAN_POINT('Ctrl Pts',(-2.06120111631275,-2.47747034382921,
41.1106083649862));
#23779=CARTESIAN_POINT('Ctrl Pts',(-2.07430377794486,-2.46651032852507,
41.109570379794));
#23780=CARTESIAN_POINT('Ctrl Pts',(-2.12939504831909,-2.41967850006918,
41.105194343007));
#23781=CARTESIAN_POINT('Ctrl Pts',(-2.17054663580616,-2.38283343274123,
41.1018966080188));
#23782=CARTESIAN_POINT('Ctrl Pts',(-2.27615696560908,-2.28326776552103,
41.0933336033125));
#23783=CARTESIAN_POINT('Ctrl Pts',(-2.33897420853146,-2.21887442229304,
41.0881382289355));
#23784=CARTESIAN_POINT('Ctrl Pts',(-2.56824119044034,-1.96328293183994,
41.0685722358207));
#23785=CARTESIAN_POINT('Ctrl Pts',(-2.71460484173427,-1.75534803790454,
41.0548320395916));
#23786=CARTESIAN_POINT('Ctrl Pts',(-2.8757065343103,-1.4573001929816,41.0352890107141));
#23787=CARTESIAN_POINT('Ctrl Pts',(-2.91331146018282,-1.38058881519907,
41.0302634888056));
#23788=CARTESIAN_POINT('Ctrl Pts',(-2.95335411860204,-1.28996292813186,
41.0242290024043));
#23789=CARTESIAN_POINT('Ctrl Pts',(-2.95880596390388,-1.27740837571555,
41.0233909103942));
#23790=CARTESIAN_POINT('Ctrl Pts',(-2.96693369862355,-1.25836056346688,
41.0221155898173));
#23791=CARTESIAN_POINT('Ctrl Pts',(-2.96966868800489,-1.25189247181759,
41.0216818742675));
#23792=CARTESIAN_POINT('Ctrl Pts',(-2.97453691650705,-1.2402736696007,41.0209015201471));
#23793=CARTESIAN_POINT('Ctrl Pts',(-2.97667795048034,-1.23512631806238,
41.0205553623453));
#23794=CARTESIAN_POINT('Ctrl Pts',(-2.98130019973509,-1.22393194386215,
41.0198015546003));
#23795=CARTESIAN_POINT('Ctrl Pts',(-2.98377634346722,-1.21788300526373,
41.0193936139739));
#23796=CARTESIAN_POINT('Ctrl Pts',(-2.99068274843617,-1.20086395241495,
41.0182442038285));
#23797=CARTESIAN_POINT('Ctrl Pts',(-2.99507097235738,-1.18987705007791,
41.0175002699164));
#23798=CARTESIAN_POINT('Ctrl Pts',(-3.02104641257968,-1.12378754707162,
41.0130148969916));
#23799=CARTESIAN_POINT('Ctrl Pts',(-3.04117147169789,-1.06812682082553,
41.0091942321191));
#23800=CARTESIAN_POINT('Ctrl Pts',(-3.13877048713662,-0.773024012652112,
40.9888273279141));
#23801=CARTESIAN_POINT('Ctrl Pts',(-3.18953323793687,-0.525670336888177,
40.971460806899));
#23802=CARTESIAN_POINT('Ctrl Pts',(-3.22491441168477,-0.112434273603035,
40.9438025902794));
#23803=CARTESIAN_POINT('Ctrl Pts',(-3.22647460986668,0.0508973108841155,
40.9331915046951));
#23804=CARTESIAN_POINT('Ctrl Pts',(-3.21420885422605,0.235494099923247,
40.921601093887));
#23805=CARTESIAN_POINT('Ctrl Pts',(-3.2125364166089,0.257304954853257,40.920237705593));
#23806=CARTESIAN_POINT('Ctrl Pts',(-3.20950946619191,0.292125950915957,
40.9180703983877));
#23807=CARTESIAN_POINT('Ctrl Pts',(-3.20829761615469,0.305147503778617,
40.9172620084051));
#23808=CARTESIAN_POINT('Ctrl Pts',(-3.20601252250869,0.328180808526523,
40.915835673054));
#23809=CARTESIAN_POINT('Ctrl Pts',(-3.20497156509783,0.338195517648916,
40.9152167170135));
#23810=CARTESIAN_POINT('Ctrl Pts',(-3.20271269702035,0.35897966734687,40.9139345949595));
#23811=CARTESIAN_POINT('Ctrl Pts',(-3.20148735818182,0.369748186159671,
40.9132716720292));
#23812=CARTESIAN_POINT('Ctrl Pts',(-3.19818197095117,0.397547492113584,
40.9115637164637));
#23813=CARTESIAN_POINT('Ctrl Pts',(-3.19602018438141,0.414568361742573,
40.9105212797827));
#23814=CARTESIAN_POINT('Ctrl Pts',(-3.18621639073025,0.487118571474866,
40.9060912570909));
#23815=CARTESIAN_POINT('Ctrl Pts',(-3.17726204624829,0.542462769683345,
40.9027453591955));
#23816=CARTESIAN_POINT('Ctrl Pts',(-3.14983773516817,0.687805389879164,
40.8940240733117));
#23817=CARTESIAN_POINT('Ctrl Pts',(-3.1289557240749,0.777297895401345,40.8887221737297));
#23818=CARTESIAN_POINT('Ctrl Pts',(-3.03866194530129,1.10104807574918,40.8695889237014));
#23819=CARTESIAN_POINT('Ctrl Pts',(-2.94652009072388,1.32807344349637,40.8563193420581));
#23820=CARTESIAN_POINT('Ctrl Pts',(-2.78606595135321,1.62241754024192,40.8370379407796));
#23821=CARTESIAN_POINT('Ctrl Pts',(-2.73913942788136,1.700445250369,40.8316961137062));
#23822=CARTESIAN_POINT('Ctrl Pts',(-2.68132677909077,1.78795889917913,40.8253098197635));
#23823=CARTESIAN_POINT('Ctrl Pts',(-2.67359945158529,1.79949333919269,40.8244598891309));
#23824=CARTESIAN_POINT('Ctrl Pts',(-2.66183028410736,1.81681781036051,40.8231702975767));
#23825=CARTESIAN_POINT('Ctrl Pts',(-2.65784343029871,1.82264525215646,40.8227342756508));
#23826=CARTESIAN_POINT('Ctrl Pts',(-2.65067318450503,1.83305219166411,40.8219514943385));
#23827=CARTESIAN_POINT('Ctrl Pts',(-2.64749702730815,1.83763656853331,40.8216052292907));
#23828=CARTESIAN_POINT('Ctrl Pts',(-2.6405881222401,1.84755359884192,40.8208530340072));
#23829=CARTESIAN_POINT('Ctrl Pts',(-2.63685116277833,1.85288312515524,40.8204468226827));
#23830=CARTESIAN_POINT('Ctrl Pts',(-2.62635864002297,1.8677511821824,40.8193081510671));
#23831=CARTESIAN_POINT('Ctrl Pts',(-2.61956737364725,1.87726421944601,40.8185733030149));
#23832=CARTESIAN_POINT('Ctrl Pts',(-2.57958681669459,1.93262859920604,40.8142607198082));
#23833=CARTESIAN_POINT('Ctrl Pts',(-2.54524812887532,1.97763305004437,40.810610633954));
#23834=CARTESIAN_POINT('Ctrl Pts',(-2.35055066220807,2.21933032591839,40.7903038460388));
#23835=CARTESIAN_POINT('Ctrl Pts',(-2.16857512377057,2.39745746428005,40.7727871770924));
#23836=CARTESIAN_POINT('Ctrl Pts',(-1.83790536018683,2.65236344919967,40.7449406447598));
#23837=CARTESIAN_POINT('Ctrl Pts',(-1.70078027280591,2.74231455234003,40.7342852963149));
#23838=CARTESIAN_POINT('Ctrl Pts',(-1.53817387918843,2.83206999741515,40.7226484448609));
#23839=CARTESIAN_POINT('Ctrl Pts',(-1.51884903318719,2.842480783709,40.7212802573875));
#23840=CARTESIAN_POINT('Ctrl Pts',(-1.4878151546486,2.8587926604125,40.7191062013691));
#23841=CARTESIAN_POINT('Ctrl Pts',(-1.47617412966667,2.86482099906657,40.7182958319227));
#23842=CARTESIAN_POINT('Ctrl Pts',(-1.45551310430304,2.87536099805379,40.71686649845));
#23843=CARTESIAN_POINT('Ctrl Pts',(-1.44650816084706,2.87990163203849,40.7162465180284));
#23844=CARTESIAN_POINT('Ctrl Pts',(-1.42777319535233,2.88923847000818,40.7149627483162));
#23845=CARTESIAN_POINT('Ctrl Pts',(-1.41803996138554,2.89402797263671,40.7142992001003));
#23846=CARTESIAN_POINT('Ctrl Pts',(-1.39285094914866,2.90626532485832,40.712590618553));
#23847=CARTESIAN_POINT('Ctrl Pts',(-1.37735941684391,2.91363912651329,40.7115481738426));
#23848=CARTESIAN_POINT('Ctrl Pts',(-1.31113530347301,2.94451487272887,40.7071264797406));
#23849=CARTESIAN_POINT('Ctrl Pts',(-1.25985275211492,2.96681904290607,40.7037886209601));
#23850=CARTESIAN_POINT('Ctrl Pts',(-1.12318041107601,3.02207816115107,40.6950946121609));
#23851=CARTESIAN_POINT('Ctrl Pts',(-1.03692109068343,3.05275076061364,40.689811170639));
#23852=CARTESIAN_POINT('Ctrl Pts',(-0.714752190887211,3.15207465386251,
40.670613102102));
#23853=CARTESIAN_POINT('Ctrl Pts',(-0.472553630327219,3.19736209181319,
40.6572690935814));
#23854=CARTESIAN_POINT('Ctrl Pts',(-0.138080133596984,3.22104043569993,
40.6379683018134));
#23855=CARTESIAN_POINT('Ctrl Pts',(-0.0483650945236136,3.22363540986981,
40.6326990910141));
#23856=CARTESIAN_POINT('Ctrl Pts',(0.0551846605660254,3.22230727058895,
40.6263931471895));
#23857=CARTESIAN_POINT('Ctrl Pts',(0.0690358363103136,3.22204027445034,
40.6255450017194));
#23858=CARTESIAN_POINT('Ctrl Pts',(0.0899438266587515,3.22150237259412,
40.6242571638466));
#23859=CARTESIAN_POINT('Ctrl Pts',(0.097002387667862,3.22129755892398,40.6238210828002));
#23860=CARTESIAN_POINT('Ctrl Pts',(0.109639740196263,3.22088929556887,40.6230379129507));
#23861=CARTESIAN_POINT('Ctrl Pts',(0.115218727679125,3.22069454792429,40.6226913166813));
#23862=CARTESIAN_POINT('Ctrl Pts',(0.127311456721132,3.22024096148563,40.6219381830628));
#23863=CARTESIAN_POINT('Ctrl Pts',(0.13382483501755,3.21997685842438,40.6215313635449));
#23864=CARTESIAN_POINT('Ctrl Pts',(0.152057546553323,3.21918214617044,40.6203893824988));
#23865=CARTESIAN_POINT('Ctrl Pts',(0.163774706545357,3.21860731112061,40.619651811571));
#23866=CARTESIAN_POINT('Ctrl Pts',(0.232715930597485,3.21484767990292,40.6152914587745));
#23867=CARTESIAN_POINT('Ctrl Pts',(0.2898461134694,3.21020101832495,40.6115944905963));
#23868=CARTESIAN_POINT('Ctrl Pts',(0.598644070961123,3.1767754761183,40.5912641572256));
#23869=CARTESIAN_POINT('Ctrl Pts',(0.846375375800036,3.11992482108336,40.5737814987779));
#23870=CARTESIAN_POINT('Ctrl Pts',(1.23869557149647,2.97966904090722,40.5459965942905));
#23871=CARTESIAN_POINT('Ctrl Pts',(1.3881086345207,2.91306767666634,40.5353688691061));
#23872=CARTESIAN_POINT('Ctrl Pts',(1.55284964782652,2.82406539641601,40.5236373674335));
#23873=CARTESIAN_POINT('Ctrl Pts',(1.57372543889928,2.81248567720223,40.5221501073252));
#23874=CARTESIAN_POINT('Ctrl Pts',(1.60538755351386,2.79445990480158,40.5198929319164));
#23875=CARTESIAN_POINT('Ctrl Pts',(1.61626769312528,2.78818114688704,40.5191170238612));
#23876=CARTESIAN_POINT('Ctrl Pts',(1.63549981824309,2.77693218414056,40.5177449258675));
#23877=CARTESIAN_POINT('Ctrl Pts',(1.64386650227094,2.77198754268475,40.5171478177317));
#23878=CARTESIAN_POINT('Ctrl Pts',(1.66158194992431,2.76140944383695,40.515883037531));
#23879=CARTESIAN_POINT('Ctrl Pts',(1.67092473725706,2.7557661765612,40.5152157335385));
#23880=CARTESIAN_POINT('Ctrl Pts',(1.6900071716636,2.74410720717462,40.5138521065015));
#23881=CARTESIAN_POINT('Ctrl Pts',(1.69974380443528,2.73808685203732,40.5131559659387));
#23882=CARTESIAN_POINT('Ctrl Pts',(1.72381559626856,2.72302489695387,40.5114338600625));
#23883=CARTESIAN_POINT('Ctrl Pts',(1.73811200718185,2.71392178712342,40.5104101648386));
#23884=CARTESIAN_POINT('Ctrl Pts',(1.9288783125375,2.59032732965147,40.4967351122949));
#23885=CARTESIAN_POINT('Ctrl Pts',(2.0938075593618,2.45893363841088,40.4847836469251));
#23886=CARTESIAN_POINT('Ctrl Pts',(2.42373322905084,2.13865464140379,40.4590301853454));
#23887=CARTESIAN_POINT('Ctrl Pts',(2.58189321732426,1.94476591908205,40.4453794647995));
#23888=CARTESIAN_POINT('Ctrl Pts',(2.72753903046045,1.71671203891744,40.4290420576392));
#23889=CARTESIAN_POINT('Ctrl Pts',(2.73880217392482,1.69868536933102,40.4277485893435));
#23890=CARTESIAN_POINT('Ctrl Pts',(2.75433566026193,1.67326789575566,40.4259199916886));
#23891=CARTESIAN_POINT('Ctrl Pts',(2.75875649509246,1.66596908052015,40.4253943457105));
#23892=CARTESIAN_POINT('Ctrl Pts',(2.76584271299706,1.65416415703902,40.4245431480926));
#23893=CARTESIAN_POINT('Ctrl Pts',(2.76852622999115,1.64966890144346,40.424218776408));
#23894=CARTESIAN_POINT('Ctrl Pts',(2.77414418653196,1.64020574504123,40.4235353805807));
#23895=CARTESIAN_POINT('Ctrl Pts',(2.77707624410192,1.63523649250323,40.4231762000395));
#23896=CARTESIAN_POINT('Ctrl Pts',(2.78420116619758,1.62308674109628,40.4222972819549));
#23897=CARTESIAN_POINT('Ctrl Pts',(2.78837959741042,1.61589786808539,40.4217766189935));
#23898=CARTESIAN_POINT('Ctrl Pts',(2.80324190456623,1.59009838977428,40.4199060809042));
#23899=CARTESIAN_POINT('Ctrl Pts',(2.81376737717131,1.57139783429284,40.4185465640782));
#23900=CARTESIAN_POINT('Ctrl Pts',(2.87764461137888,1.45520777051212,40.4100836427643));
#23901=CARTESIAN_POINT('Ctrl Pts',(2.92610575809438,1.35512663248414,40.4027272278837));
#23902=CARTESIAN_POINT('Ctrl Pts',(3.09368764517555,0.957921600581406,40.37379496271));
#23903=CARTESIAN_POINT('Ctrl Pts',(3.1735059966434,0.646114547682966,40.351870055001));
#23904=CARTESIAN_POINT('Ctrl Pts',(3.21046813876591,0.284426754869854,40.3287939816476));
#23905=CARTESIAN_POINT('Ctrl Pts',(3.21401014084984,0.241129345005754,40.3260641302216));
#23906=CARTESIAN_POINT('Ctrl Pts',(3.2176651823808,0.181681614284291,40.322358818661));
#23907=CARTESIAN_POINT('Ctrl Pts',(3.21853373206233,0.165584013924313,40.3213597545801));
#23908=CARTESIAN_POINT('Ctrl Pts',(3.21972472178267,0.139934277854415,40.3197745050124));
#23909=CARTESIAN_POINT('Ctrl Pts',(3.22012551373191,0.130386215296407,40.3191858647466));
#23910=CARTESIAN_POINT('Ctrl Pts',(3.22084429607181,0.111229517769128,40.3180077380531));
#23911=CARTESIAN_POINT('Ctrl Pts',(3.22116177312373,0.101620960980645,40.3174182737083));
#23912=CARTESIAN_POINT('Ctrl Pts',(3.22171475437482,0.0822603084688677,
40.3162334156258));
#23913=CARTESIAN_POINT('Ctrl Pts',(3.22194898627566,0.0725082756372689,
40.3156380678866));
#23914=CARTESIAN_POINT('Ctrl Pts',(3.22235110246199,0.0518618064420085,
40.3143806714447));
#23915=CARTESIAN_POINT('Ctrl Pts',(3.22250802367108,0.040967260254133,40.3137189716861));
#23916=CARTESIAN_POINT('Ctrl Pts',(3.22270461541348,0.0198998894239589,
40.3124427752497));
#23917=CARTESIAN_POINT('Ctrl Pts',(3.22275137521086,0.00972729443329853,
40.3118280689229));
#23918=CARTESIAN_POINT('Ctrl Pts',(3.22274996921859,-0.000445422926308301,
40.3112148290304));
#23919=CARTESIAN_POINT('Origin',(0.,0.,32.));
#23920=CARTESIAN_POINT('',(3.93418083709056,-0.00237382471849651,7.40416393604293));
#23921=CARTESIAN_POINT('',(-1.74869731566807,-3.5228605845499,7.00006232951278));
#23922=CARTESIAN_POINT('Ctrl Pts',(3.93299927912326,-0.0023812635191002,
7.40416352203497));
#23923=CARTESIAN_POINT('Ctrl Pts',(3.93292585737052,-0.123647850894427,
7.39799858961059));
#23924=CARTESIAN_POINT('Ctrl Pts',(3.92724440793317,-0.244754597722826,
7.3918336571862));
#23925=CARTESIAN_POINT('Ctrl Pts',(3.91599597959321,-0.36532791819104,7.38566872476181));
#23926=CARTESIAN_POINT('Ctrl Pts',(3.90526101570742,-0.480397348488062,
7.37978520708859));
#23927=CARTESIAN_POINT('Ctrl Pts',(3.88943218768411,-0.595182928816867,
7.37390168941536));
#23928=CARTESIAN_POINT('Ctrl Pts',(3.86853025860236,-0.709198588745032,
7.36801817174214));
#23929=CARTESIAN_POINT('Ctrl Pts',(3.84765547744091,-0.823066162435068,
7.36214229572095));
#23930=CARTESIAN_POINT('Ctrl Pts',(3.82172077314429,-0.936165403225679,
7.35626641969975));
#23931=CARTESIAN_POINT('Ctrl Pts',(3.7907987530201,-1.04801422418841,7.35039054367856));
#23932=CARTESIAN_POINT('Ctrl Pts',(3.75990870699832,-1.15974739081674,7.34452074345258));
#23933=CARTESIAN_POINT('Ctrl Pts',(3.72404171256226,-1.27023231513042,7.33865094322661));
#23934=CARTESIAN_POINT('Ctrl Pts',(3.68332150352764,-1.37899662858577,7.33278114300062));
#23935=CARTESIAN_POINT('Ctrl Pts',(3.64110685382046,-1.49175261638668,7.32669591980886));
#23936=CARTESIAN_POINT('Ctrl Pts',(3.59367600534624,-1.60265883264998,7.32061069661709));
#23937=CARTESIAN_POINT('Ctrl Pts',(3.54122374104448,-1.7112052524063,7.31452547342533));
#23938=CARTESIAN_POINT('Ctrl Pts',(3.49068837256741,-1.81578478566906,7.30866263794331));
#23939=CARTESIAN_POINT('Ctrl Pts',(3.43549237357525,-1.91817357726072,7.30279980246129));
#23940=CARTESIAN_POINT('Ctrl Pts',(3.37585883407791,-2.01793610710997,7.29693696697926));
#23941=CARTESIAN_POINT('Ctrl Pts',(3.31623521582783,-2.11768203944153,7.29107510689868));
#23942=CARTESIAN_POINT('Ctrl Pts',(3.25217573637191,-2.21480222565135,7.2852132468181));
#23943=CARTESIAN_POINT('Ctrl Pts',(3.18394863562698,-2.30888719639767,7.27935138673752));
#23944=CARTESIAN_POINT('Ctrl Pts',(3.11571652777115,-2.40297907193515,7.27348909646156));
#23945=CARTESIAN_POINT('Ctrl Pts',(3.04331643237488,-2.49403495594284,7.26762680618561));
#23946=CARTESIAN_POINT('Ctrl Pts',(2.96705855633027,-2.58167630103143,7.26176451590965));
#23947=CARTESIAN_POINT('Ctrl Pts',(2.8907768004645,-2.66934509062484,7.25590038988307));
#23948=CARTESIAN_POINT('Ctrl Pts',(2.81063513182465,-2.75359690462564,7.25003626385649));
#23949=CARTESIAN_POINT('Ctrl Pts',(2.72698200459874,-2.83408859187476,7.24417213782991));
#23950=CARTESIAN_POINT('Ctrl Pts',(2.64323690311214,-2.91466877747022,7.23830156436169));
#23951=CARTESIAN_POINT('Ctrl Pts',(2.55597293371334,-2.9914802987659,7.23243099089347));
#23952=CARTESIAN_POINT('Ctrl Pts',(2.46557322678828,-3.06421893201919,7.22656041742525));
#23953=CARTESIAN_POINT('Ctrl Pts',(2.37511446262001,-3.13700508470923,7.22068600876887));
#23954=CARTESIAN_POINT('Ctrl Pts',(2.2815162124136,-3.2057128073294,7.2148116001125));
#23955=CARTESIAN_POINT('Ctrl Pts',(2.18519089692271,-3.27008099960936,7.20893719145613));
#23956=CARTESIAN_POINT('Ctrl Pts',(2.08872771426264,-3.33454131990789,7.20305437495714));
#23957=CARTESIAN_POINT('Ctrl Pts',(1.98953002689324,-3.39464950063828,7.19717155845815));
#23958=CARTESIAN_POINT('Ctrl Pts',(1.88803521411711,-3.45019014407232,7.19128874195916));
#23959=CARTESIAN_POINT('Ctrl Pts',(1.8618515330919,-3.46451854620277,7.18977109010557));
#23960=CARTESIAN_POINT('Ctrl Pts',(1.83551507272312,-3.47854321029207,7.18825343825199));
#23961=CARTESIAN_POINT('Ctrl Pts',(1.80903354477158,-3.49226096302828,7.1867357863984));
#23962=CARTESIAN_POINT('Ctrl Pts',(1.70742084100427,-3.54489757628143,7.18091237966361));
#23963=CARTESIAN_POINT('Ctrl Pts',(1.60332732097401,-3.59318953488544,7.17508897292881));
#23964=CARTESIAN_POINT('Ctrl Pts',(1.49716436618334,-3.63689261054418,7.16926556619402));
#23965=CARTESIAN_POINT('Ctrl Pts',(1.39113729163722,-3.68053974969833,7.1634496129625));
#23966=CARTESIAN_POINT('Ctrl Pts',(1.28304643338149,-3.7196095233296,7.15763365973098));
#23967=CARTESIAN_POINT('Ctrl Pts',(1.17332818810424,-3.75390329696971,7.15181770649946));
#23968=CARTESIAN_POINT('Ctrl Pts',(1.06371979961478,-3.78816273353302,7.14600757656505));
#23969=CARTESIAN_POINT('Ctrl Pts',(0.952487663460509,-3.81765555398607,
7.14019744663064));
#23970=CARTESIAN_POINT('Ctrl Pts',(0.840087882685277,-3.84223129826477,
7.13438731669622));
#23971=CARTESIAN_POINT('Ctrl Pts',(0.727766419218824,-3.86678991878984,
7.12858123511259));
#23972=CARTESIAN_POINT('Ctrl Pts',(0.614279338846755,-3.88643818659611,
7.12277515352895));
#23973=CARTESIAN_POINT('Ctrl Pts',(0.500096915293078,-3.90107575872532,
7.11696907194531));
#23974=CARTESIAN_POINT('Ctrl Pts',(0.385955601725311,-3.91570806077561,
7.11116508077038));
#23975=CARTESIAN_POINT('Ctrl Pts',(0.271119859460527,-3.92533319898689,
7.10536108959544));
#23976=CARTESIAN_POINT('Ctrl Pts',(0.156068457457715,-3.92990224262472,
7.09955709842051));
#23977=CARTESIAN_POINT('Ctrl Pts',(0.0410294744845688,-3.93447079306482,
7.09375373374762));
#23978=CARTESIAN_POINT('Ctrl Pts',(-0.0742247014207859,-3.93398431752344,
7.08795036907474));
#23979=CARTESIAN_POINT('Ctrl Pts',(-0.189212714966521,-3.9284459457265,
7.08214700440185));
#23980=CARTESIAN_POINT('Ctrl Pts',(-0.304217305000114,-3.92290677552676,
7.0763428031252));
#23981=CARTESIAN_POINT('Ctrl Pts',(-0.418955236063756,-3.91231428262367,
7.07053860184856));
#23982=CARTESIAN_POINT('Ctrl Pts',(-0.53294851104485,-3.89672360895343,
7.06473440057192));
#23983=CARTESIAN_POINT('Ctrl Pts',(-0.647054491955444,-3.88111752067766,
7.05892446064184));
#23984=CARTESIAN_POINT('Ctrl Pts',(-0.760413929013011,-3.86050344122573,
7.05311452071175));
#23985=CARTESIAN_POINT('Ctrl Pts',(-0.872557250876692,-3.83498798484982,
7.04730458078166));
#23986=CARTESIAN_POINT('Ctrl Pts',(-0.984759398021493,-3.80945914422714,
7.0414915932216));
#23987=CARTESIAN_POINT('Ctrl Pts',(-1.09574375418876,-3.77902391875517,
7.03567860566153));
#23988=CARTESIAN_POINT('Ctrl Pts',(-1.20505597687301,-3.74383881765797,
7.02986561810146));
#23989=CARTESIAN_POINT('Ctrl Pts',(-1.31453623477521,-3.70859962987232,
7.02404369479197));
#23990=CARTESIAN_POINT('Ctrl Pts',(-1.4223388316586,-3.66859613125696,7.01822177148247));
#23991=CARTESIAN_POINT('Ctrl Pts',(-1.52802922734547,-3.62403306833395,
7.01239984817297));
#23992=CARTESIAN_POINT('Ctrl Pts',(-1.60268710010629,-3.59255448922639,
7.00828734195291));
#23993=CARTESIAN_POINT('Ctrl Pts',(-1.67629148578956,-3.55880179689948,
7.00417483573285));
#23994=CARTESIAN_POINT('Ctrl Pts',(-1.74869731566807,-3.5228605845499,7.00006232951278));
#23995=CARTESIAN_POINT('',(1.748694475331,-3.52286199445094,7.));
#23996=CARTESIAN_POINT('Origin',(0.,0.,7.));
#23997=CARTESIAN_POINT('',(3.93500029318814,-0.00400916611326436,7.22083647796505));
#23998=CARTESIAN_POINT('Ctrl Pts',(1.74869447533099,-3.52286199445094,7.));
#23999=CARTESIAN_POINT('Ctrl Pts',(2.9229184098028,-2.93999530530824,7.06631097945448));
#24000=CARTESIAN_POINT('Ctrl Pts',(3.86598732707265,-1.59538332201294,7.13992313877617));
#24001=CARTESIAN_POINT('Ctrl Pts',(3.93807145761699,-0.14775304387093,7.21353529809785));
#24002=CARTESIAN_POINT('Ctrl Pts',(3.93699603905802,-0.00401119947441216,
7.22083647796505));
#24003=CARTESIAN_POINT('',(3.93141612693361,-0.00220398940945714,8.47083644545494));
#24004=CARTESIAN_POINT('Ctrl Pts',(3.9329979586749,-0.00400712603929224,
7.22083647796505));
#24005=CARTESIAN_POINT('Ctrl Pts',(3.93311290453778,0.108812345978177,7.22657287120762));
#24006=CARTESIAN_POINT('Ctrl Pts',(3.92836938073138,0.221859929722491,7.23230926445019));
#24007=CARTESIAN_POINT('Ctrl Pts',(3.91873516811271,0.334669511901911,7.23804565769276));
#24008=CARTESIAN_POINT('Ctrl Pts',(3.90911290769752,0.447339142521888,7.24377493436629));
#24009=CARTESIAN_POINT('Ctrl Pts',(3.89461204877992,0.559770931113545,7.24950421103982));
#24010=CARTESIAN_POINT('Ctrl Pts',(3.87525235530899,0.671496971454175,7.25523348771335));
#24011=CARTESIAN_POINT('Ctrl Pts',(3.85517041850384,0.787391124684349,7.26117650392225));
#24012=CARTESIAN_POINT('Ctrl Pts',(3.82986000999708,0.902525375176162,7.26711952013114));
#24013=CARTESIAN_POINT('Ctrl Pts',(3.79940243032467,1.01638091896837,7.27306253634004));
#24014=CARTESIAN_POINT('Ctrl Pts',(3.7700858418477,1.12597124620641,7.27878291735463));
#24015=CARTESIAN_POINT('Ctrl Pts',(3.7360009146518,1.23437648833816,7.28450329836921));
#24016=CARTESIAN_POINT('Ctrl Pts',(3.69727230456486,1.34114373051425,7.29022367938379));
#24017=CARTESIAN_POINT('Ctrl Pts',(3.65855424625676,1.44788188348923,7.2959425018556));
#24018=CARTESIAN_POINT('Ctrl Pts',(3.61519516540431,1.55298251607409,7.30166132432741));
#24019=CARTESIAN_POINT('Ctrl Pts',(3.56736922138118,1.65600900913679,7.30738014679922));
#24020=CARTESIAN_POINT('Ctrl Pts',(3.51954362641718,1.75903475025746,7.31309892753203));
#24021=CARTESIAN_POINT('Ctrl Pts',(3.46725141621909,1.85998598947352,7.31881770826484));
#24022=CARTESIAN_POINT('Ctrl Pts',(3.410714010603,1.95844809425127,7.32453648899765));
#24023=CARTESIAN_POINT('Ctrl Pts',(3.35416202302715,2.05693559408266,7.3302567447014));
#24024=CARTESIAN_POINT('Ctrl Pts',(3.29336288198745,2.15293230961354,7.33597700040514));
#24025=CARTESIAN_POINT('Ctrl Pts',(3.22858235517417,2.24605097356627,7.34169725610889));
#24026=CARTESIAN_POINT('Ctrl Pts',(3.16373129213117,2.33927102970884,7.34742374030893));
#24027=CARTESIAN_POINT('Ctrl Pts',(3.09489044247763,2.42960642705178,7.35315022450896));
#24028=CARTESIAN_POINT('Ctrl Pts',(3.02236691452957,2.51670165771729,7.35887670870899));
#24029=CARTESIAN_POINT('Ctrl Pts',(2.94979643021604,2.6038532793996,7.36460690060076));
#24030=CARTESIAN_POINT('Ctrl Pts',(2.87353881682546,2.68776024383179,7.37033709249253));
#24031=CARTESIAN_POINT('Ctrl Pts',(2.79393781419547,2.7681041328694,7.37606728438429));
#24032=CARTESIAN_POINT('Ctrl Pts',(2.71421878928923,2.84856714564105,7.38180597227822));
#24033=CARTESIAN_POINT('Ctrl Pts',(2.63114680560452,2.92545625576873,7.38754466017214));
#24034=CARTESIAN_POINT('Ctrl Pts',(2.54509822031751,2.99849362996433,7.39328334806607));
#24035=CARTESIAN_POINT('Ctrl Pts',(2.52219402365628,3.0179345350834,7.39481085761967));
#24036=CARTESIAN_POINT('Ctrl Pts',(2.49907908717383,3.03710278437769,7.39633836717327));
#24037=CARTESIAN_POINT('Ctrl Pts',(2.47576082822077,3.05599367169627,7.39786587672687));
#24038=CARTESIAN_POINT('Ctrl Pts',(2.38599445874981,3.12871635541322,7.40374620369447));
#24039=CARTESIAN_POINT('Ctrl Pts',(2.29287298841318,3.19760055359902,7.40962653066206));
#24040=CARTESIAN_POINT('Ctrl Pts',(2.19675830299184,3.26232155960084,7.41550685762966));
#24041=CARTESIAN_POINT('Ctrl Pts',(2.1007680438308,3.3269587803548,7.42137957215915));
#24042=CARTESIAN_POINT('Ctrl Pts',(2.00179261458001,3.38744329934152,7.42725228668864));
#24043=CARTESIAN_POINT('Ctrl Pts',(1.90022729055141,3.44349027067649,7.43312500121813));
#24044=CARTESIAN_POINT('Ctrl Pts',(1.79876649403358,3.49947956041141,7.4389916717534));
#24045=CARTESIAN_POINT('Ctrl Pts',(1.69472146340341,3.55104018909941,7.44485834228867));
#24046=CARTESIAN_POINT('Ctrl Pts',(1.58851625654027,3.59793066952481,7.45072501282394));
#24047=CARTESIAN_POINT('Ctrl Pts',(1.47833310201707,3.64657744686256,7.45681142125171));
#24048=CARTESIAN_POINT('Ctrl Pts',(1.36582515837295,3.6901971321489,7.46289782967947));
#24049=CARTESIAN_POINT('Ctrl Pts',(1.25149413262529,3.72857230532069,7.46898423810724));
#24050=CARTESIAN_POINT('Ctrl Pts',(1.14141986485899,3.76551869900226,7.47484403816266));
#24051=CARTESIAN_POINT('Ctrl Pts',(1.02965626948239,3.79760398859222,7.48070383821808));
#24052=CARTESIAN_POINT('Ctrl Pts',(0.916670495179452,3.82468354289181,7.48656363827351));
#24053=CARTESIAN_POINT('Ctrl Pts',(0.803702774904854,3.85175877014188,7.49242250198985));
#24054=CARTESIAN_POINT('Ctrl Pts',(0.689513664648633,3.87382975664777,7.4982813657062));
#24055=CARTESIAN_POINT('Ctrl Pts',(0.574583218563554,3.89080237546771,7.50414022942254));
#24056=CARTESIAN_POINT('Ctrl Pts',(0.459643519947996,3.90777636067643,7.5099995648095));
#24057=CARTESIAN_POINT('Ctrl Pts',(0.343962774535669,3.91965110209251,7.51585890019647));
#24058=CARTESIAN_POINT('Ctrl Pts',(0.228028227937334,3.92638410337855,7.52171823558344));
#24059=CARTESIAN_POINT('Ctrl Pts',(0.11205648961027,3.93311926460711,7.52757945064146));
#24060=CARTESIAN_POINT('Ctrl Pts',(-0.00416880063361079,3.93470938181026,
7.53344066569948));
#24061=CARTESIAN_POINT('Ctrl Pts',(-0.120159010774501,3.93116405306745,
7.53930188075751));
#24062=CARTESIAN_POINT('Ctrl Pts',(-0.236278348012045,3.92761477745699,
7.54516962086349));
#24063=CARTESIAN_POINT('Ctrl Pts',(-0.352161670640159,3.91891865709447,
7.55103736096948));
#24064=CARTESIAN_POINT('Ctrl Pts',(-0.467323979016736,3.90513729574723,
7.55690510107546));
#24065=CARTESIAN_POINT('Ctrl Pts',(-0.582562376489921,3.89134682889185,
7.56277671806659));
#24066=CARTESIAN_POINT('Ctrl Pts',(-0.697078405367553,3.87246449701755,
7.56864833505772));
#24067=CARTESIAN_POINT('Ctrl Pts',(-0.810397477410202,3.84860298401994,
7.57451995204886));
#24068=CARTESIAN_POINT('Ctrl Pts',(-0.923880375902674,3.82470697420823,
7.58040005769199));
#24069=CARTESIAN_POINT('Ctrl Pts',(-1.03616246611069,3.79581751833037,7.58628016333511));
#24070=CARTESIAN_POINT('Ctrl Pts',(-1.14678443855703,3.76209708161332,7.59216026897824));
#24071=CARTESIAN_POINT('Ctrl Pts',(-1.17587264157831,3.75323024541884,7.5937064510156));
#24072=CARTESIAN_POINT('Ctrl Pts',(-1.20484616862641,3.74402963576712,7.59525263305295));
#24073=CARTESIAN_POINT('Ctrl Pts',(-1.23369691855059,3.73449874992063,7.59679881509031));
#24074=CARTESIAN_POINT('Ctrl Pts',(-1.34345847125961,3.69823886648773,7.60268120433972));
#24075=CARTESIAN_POINT('Ctrl Pts',(-1.45179681044438,3.65707747085414,7.60856359358913));
#24076=CARTESIAN_POINT('Ctrl Pts',(-1.55824306996784,3.61114490638318,7.61444598283854));
#24077=CARTESIAN_POINT('Ctrl Pts',(-1.66455493795266,3.56527033312808,7.62032094539823));
#24078=CARTESIAN_POINT('Ctrl Pts',(-1.76897910248425,3.51463673299237,7.62619590795792));
#24079=CARTESIAN_POINT('Ctrl Pts',(-1.87106234597096,3.45942404129497,7.6320708705176));
#24080=CARTESIAN_POINT('Ctrl Pts',(-1.97304373632805,3.40426643783001,7.63793997135793));
#24081=CARTESIAN_POINT('Ctrl Pts',(-2.07268849171423,3.34453902597639,7.64380907219826));
#24082=CARTESIAN_POINT('Ctrl Pts',(-2.16956446485834,3.28046933118173,7.64967817303859));
#24083=CARTESIAN_POINT('Ctrl Pts',(-2.2700134313952,3.21403660880917,7.65576373888923));
#24084=CARTESIAN_POINT('Ctrl Pts',(-2.36748502619612,3.14293530214689,7.66184930473986));
#24085=CARTESIAN_POINT('Ctrl Pts',(-2.46152634707033,3.06747078921358,7.66793487059049));
#24086=CARTESIAN_POINT('Ctrl Pts',(-2.55212327068198,2.99477027150441,7.67379754392789));
#24087=CARTESIAN_POINT('Ctrl Pts',(-2.63953643783171,2.91802083391656,7.67966021726529));
#24088=CARTESIAN_POINT('Ctrl Pts',(-2.72339212490094,2.83753842864331,7.68552289060269));
#24089=CARTESIAN_POINT('Ctrl Pts',(-2.80723670136208,2.75706668702919,7.69138478715479));
#24090=CARTESIAN_POINT('Ctrl Pts',(-2.88752443803497,2.67286324626018,7.69724668370688));
#24091=CARTESIAN_POINT('Ctrl Pts',(-2.9639172344716,2.58528211752648,7.70310858025897));
#24092=CARTESIAN_POINT('Ctrl Pts',(-3.04031822508946,2.49769159450858,7.70897110558033));
#24093=CARTESIAN_POINT('Ctrl Pts',(-3.11282317413419,2.40672297343814,7.7148336309017));
#24094=CARTESIAN_POINT('Ctrl Pts',(-3.18113362464812,2.31276411727031,7.72069615622306));
#24095=CARTESIAN_POINT('Ctrl Pts',(-3.24946778044208,2.21877265524232,7.72656071597405));
#24096=CARTESIAN_POINT('Ctrl Pts',(-3.3136043010335,2.12178922731686,7.73242527572503));
#24097=CARTESIAN_POINT('Ctrl Pts',(-3.3732878846183,2.02223090854813,7.73828983547602));
#24098=CARTESIAN_POINT('Ctrl Pts',(-3.43304005453589,1.92255818076484,7.74416113457848));
#24099=CARTESIAN_POINT('Ctrl Pts',(-3.48832886172091,1.8203050093091,7.75003243368094));
#24100=CARTESIAN_POINT('Ctrl Pts',(-3.53894477635643,1.71591342144629,7.7559037327834));
#24101=CARTESIAN_POINT('Ctrl Pts',(-3.58959522811968,1.6114506033068,7.76177903809237));
#24102=CARTESIAN_POINT('Ctrl Pts',(-3.63556627523173,1.50484684023992,7.76765434340135));
#24103=CARTESIAN_POINT('Ctrl Pts',(-3.67669703722869,1.39656288667349,7.77352964871032));
#24104=CARTESIAN_POINT('Ctrl Pts',(-3.71788836184128,1.28811949138651,7.77941360505905));
#24105=CARTESIAN_POINT('Ctrl Pts',(-3.75422504826353,1.17799135740374,7.78529756140779));
#24106=CARTESIAN_POINT('Ctrl Pts',(-3.78559638614092,1.06665317757781,7.79118151775652));
#24107=CARTESIAN_POINT('Ctrl Pts',(-3.7936831774663,1.0379528196167,7.79269826298893));
#24108=CARTESIAN_POINT('Ctrl Pts',(-3.80144029403778,1.00917209940504,7.79421500822134));
#24109=CARTESIAN_POINT('Ctrl Pts',(-3.80886639532414,0.98031922482961,7.79573175345375));
#24110=CARTESIAN_POINT('Ctrl Pts',(-3.83757891436247,0.868761534109808,
7.80159614644847));
#24111=CARTESIAN_POINT('Ctrl Pts',(-3.86143551269301,0.755749566578593,
7.80746053944319));
#24112=CARTESIAN_POINT('Ctrl Pts',(-3.8802903004427,0.641744641029695,7.81332493243792));
#24113=CARTESIAN_POINT('Ctrl Pts',(-3.89912030216079,0.527889583499651,
7.81918161624854));
#24114=CARTESIAN_POINT('Ctrl Pts',(-3.91296150113471,0.413044568746285,
7.82503830005917));
#24115=CARTESIAN_POINT('Ctrl Pts',(-3.92171807829749,0.297684924634476,
7.83089498386979));
#24116=CARTESIAN_POINT('Ctrl Pts',(-3.93046550417522,0.182445840070855,
7.83674554700312));
#24117=CARTESIAN_POINT('Ctrl Pts',(-3.93413884572687,0.0666936067228916,
7.84259611013644));
#24118=CARTESIAN_POINT('Ctrl Pts',(-3.93269365160892,-0.0490881105248623,
7.84844667326977));
#24119=CARTESIAN_POINT('Ctrl Pts',(-3.9311887151358,-0.169656086163691,
7.85453909070925));
#24120=CARTESIAN_POINT('Ctrl Pts',(-3.92413286646031,-0.290255584384087,
7.86063150814872));
#24121=CARTESIAN_POINT('Ctrl Pts',(-3.91153590472006,-0.410336284144846,
7.8667239255882));
#24122=CARTESIAN_POINT('Ctrl Pts',(-3.89945339953288,-0.5255129201987,7.87256753032662));
#24123=CARTESIAN_POINT('Ctrl Pts',(-3.88227352681979,-0.640211846360301,
7.87841113506504));
#24124=CARTESIAN_POINT('Ctrl Pts',(-3.86005803938839,-0.753950218882538,
7.88425473980346));
#24125=CARTESIAN_POINT('Ctrl Pts',(-3.83784612814636,-0.867670282107759,
7.89009740385412));
#24126=CARTESIAN_POINT('Ctrl Pts',(-3.8106002933054,-0.980429692266308,
7.89594006790478));
#24127=CARTESIAN_POINT('Ctrl Pts',(-3.77843359716715,-1.09175480388157,
7.90178273195544));
#24128=CARTESIAN_POINT('Ctrl Pts',(-3.74626423163027,-1.20308915396821,
7.90762588086781));
#24129=CARTESIAN_POINT('Ctrl Pts',(-3.70917330821319,-1.31298857052792,
7.91346902978019));
#24130=CARTESIAN_POINT('Ctrl Pts',(-3.66732384442588,-1.42099430685187,
7.91931217869256));
#24131=CARTESIAN_POINT('Ctrl Pts',(-3.62546069787914,-1.52903535585063,
7.92515723803326));
#24132=CARTESIAN_POINT('Ctrl Pts',(-3.57883606732273,-1.6351811071349,7.93100229737395));
#24133=CARTESIAN_POINT('Ctrl Pts',(-3.52766092273846,-1.73899321855609,
7.93684735671465));
#24134=CARTESIAN_POINT('Ctrl Pts',(-3.4764275273619,-1.84292349550056,7.94269906927226));
#24135=CARTESIAN_POINT('Ctrl Pts',(-3.42063346306906,-1.94451445861301,
7.94855078182987));
#24136=CARTESIAN_POINT('Ctrl Pts',(-3.36053547687665,-2.04335271273793,
7.95440249438748));
#24137=CARTESIAN_POINT('Ctrl Pts',(-3.30039711067037,-2.14225737657679,
7.96025813872799));
#24138=CARTESIAN_POINT('Ctrl Pts',(-3.23594929514515,-2.23840530530489,
7.96611378306849));
#24139=CARTESIAN_POINT('Ctrl Pts',(-3.16749085903314,-2.33141387530002,
7.97196942740899));
#24140=CARTESIAN_POINT('Ctrl Pts',(-3.09893078147948,-2.4245605367515,7.97783376572743));
#24141=CARTESIAN_POINT('Ctrl Pts',(-3.02634845855472,-2.51455821550396,
7.98369810404587));
#24142=CARTESIAN_POINT('Ctrl Pts',(-2.95008158690857,-2.60105894408086,
7.98956244236431));
#24143=CARTESIAN_POINT('Ctrl Pts',(-2.92796300148598,-2.62614550804825,
7.99126319218193));
#24144=CARTESIAN_POINT('Ctrl Pts',(-2.90553473678805,-2.65093819525922,
7.99296394199956));
#24145=CARTESIAN_POINT('Ctrl Pts',(-2.88280556274161,-2.67542914079705,
7.99466469181719));
#24146=CARTESIAN_POINT('Ctrl Pts',(-2.8043081914697,-2.76001095801379,8.00053839358929));
#24147=CARTESIAN_POINT('Ctrl Pts',(-2.72195407090228,-2.84127646596739,
8.00641209536139));
#24148=CARTESIAN_POINT('Ctrl Pts',(-2.63605453258703,-2.91885345662083,
8.0122857971335));
#24149=CARTESIAN_POINT('Ctrl Pts',(-2.55026625588345,-2.9963299654652,8.01815189097733));
#24150=CARTESIAN_POINT('Ctrl Pts',(-2.46094199760085,-3.07012718360594,
8.02401798482117));
#24151=CARTESIAN_POINT('Ctrl Pts',(-2.36843181965343,-3.13990759667433,
8.02988407866501));
#24152=CARTESIAN_POINT('Ctrl Pts',(-2.27601675373697,-3.2096162667523,8.03574414143084));
#24153=CARTESIAN_POINT('Ctrl Pts',(-2.18042261128095,-3.27531609887929,
8.04160420419668));
#24154=CARTESIAN_POINT('Ctrl Pts',(-2.0820341128983,-3.33670840091366,8.04746426696251));
#24155=CARTESIAN_POINT('Ctrl Pts',(-1.97980367936051,-3.40049798766442,
8.0535531570966));
#24156=CARTESIAN_POINT('Ctrl Pts',(-1.87455654824124,-3.45963647775856,
8.05964204723068));
#24157=CARTESIAN_POINT('Ctrl Pts',(-1.76675979720991,-3.51383676612372,
8.06573093736477));
#24158=CARTESIAN_POINT('Ctrl Pts',(-1.66313443646764,-3.56593967628047,
8.07158420688011));
#24159=CARTESIAN_POINT('Ctrl Pts',(-1.55715351553769,-3.61347926252958,
8.07743747639547));
#24160=CARTESIAN_POINT('Ctrl Pts',(-1.44925819231429,-3.65624666728189,
8.08329074591081));
#24161=CARTESIAN_POINT('Ctrl Pts',(-1.34137938292998,-3.69900752630061,
8.0891431195583));
#24162=CARTESIAN_POINT('Ctrl Pts',(-1.23158713783247,-3.7369975039187,8.0949954932058));
#24163=CARTESIAN_POINT('Ctrl Pts',(-1.12034252612701,-3.77005591790776,
8.1008478668533));
#24164=CARTESIAN_POINT('Ctrl Pts',(-1.00908803632947,-3.80311726735637,
8.10670076016899));
#24165=CARTESIAN_POINT('Ctrl Pts',(-0.896381319617469,-3.83124606496304,
8.11255365348467));
#24166=CARTESIAN_POINT('Ctrl Pts',(-0.78269784444515,-3.85433172992426,
8.11840654680035));
#24167=CARTESIAN_POINT('Ctrl Pts',(-0.668976780273355,-3.87742502807092,
8.12426137535248));
#24168=CARTESIAN_POINT('Ctrl Pts',(-0.554278720128107,-3.8954717956566,
8.1301162039046));
#24169=CARTESIAN_POINT('Ctrl Pts',(-0.439087835519406,-3.90841283294113,
8.13597103245673));
#24170=CARTESIAN_POINT('Ctrl Pts',(-0.323766291036385,-3.92136854911548,
8.14183250208263));
#24171=CARTESIAN_POINT('Ctrl Pts',(-0.207951217146528,-3.92920692934892,
8.14769397170852));
#24172=CARTESIAN_POINT('Ctrl Pts',(-0.0921305048125156,-3.93192077362744,
8.15355544133442));
#24173=CARTESIAN_POINT('Ctrl Pts',(0.0237680012788959,-3.93463644072451,
8.15942084795688));
#24174=CARTESIAN_POINT('Ctrl Pts',(0.139671741283028,-3.93222072659018,
8.16528625457934));
#24175=CARTESIAN_POINT('Ctrl Pts',(0.255095976324763,-3.92471846670088,
8.1711516612018));
#24176=CARTESIAN_POINT('Ctrl Pts',(0.370689957236543,-3.91720517379385,
8.17702569364318));
#24177=CARTESIAN_POINT('Ctrl Pts',(0.485802616608141,-3.9045904503839,8.18289972608456));
#24178=CARTESIAN_POINT('Ctrl Pts',(0.59995736727677,-3.88697056297708,8.18877375852594));
#24179=CARTESIAN_POINT('Ctrl Pts',(0.631206080518413,-3.882147296265,8.19038171574416));
#24180=CARTESIAN_POINT('Ctrl Pts',(0.662383093154374,-3.87694926574991,
8.19198967296239));
#24181=CARTESIAN_POINT('Ctrl Pts',(0.693478824783114,-3.87137909788972,
8.19359763018062));
#24182=CARTESIAN_POINT('Ctrl Pts',(0.807061363038884,-3.85103309633476,
8.19947097204096));
#24183=CARTESIAN_POINT('Ctrl Pts',(0.919937230665374,-3.82565031194341,
8.2053443139013));
#24184=CARTESIAN_POINT('Ctrl Pts',(1.03162505281565,-3.79529165551254,8.21121765576164));
#24185=CARTESIAN_POINT('Ctrl Pts',(1.14316854615067,-3.76497223011717,8.21708340778403));
#24186=CARTESIAN_POINT('Ctrl Pts',(1.25352665202299,-3.72968982732742,8.22294915980642));
#24187=CARTESIAN_POINT('Ctrl Pts',(1.36222626986069,-3.68955669284285,8.22881491182881));
#24188=CARTESIAN_POINT('Ctrl Pts',(1.47081446598169,-3.6494646965226,8.23467465120668));
#24189=CARTESIAN_POINT('Ctrl Pts',(1.57774717021002,-3.60453200084474,8.24053439058456));
#24190=CARTESIAN_POINT('Ctrl Pts',(1.68256523073041,-3.55492098988671,8.24639412996243));
#24191=CARTESIAN_POINT('Ctrl Pts',(1.79148459468508,-3.50336880763997,8.25248314823667));
#24192=CARTESIAN_POINT('Ctrl Pts',(1.89812001434187,-3.446764849266,8.2585721665109));
#24193=CARTESIAN_POINT('Ctrl Pts',(2.00197749850025,-3.38534711595409,8.26466118478513));
#24194=CARTESIAN_POINT('Ctrl Pts',(2.10180924051122,-3.32631006767028,8.2705141794574));
#24195=CARTESIAN_POINT('Ctrl Pts',(2.19907400558695,-3.26282570995485,8.27636717412966));
#24196=CARTESIAN_POINT('Ctrl Pts',(2.29335775739799,-3.19515245279196,8.28222016880192));
#24197=CARTESIAN_POINT('Ctrl Pts',(2.38762737583228,-3.12748934002427,8.28807228609524));
#24198=CARTESIAN_POINT('Ctrl Pts',(2.47891653390792,-3.05563881721695,8.29392440338855));
#24199=CARTESIAN_POINT('Ctrl Pts',(2.56684098390339,-2.97990207277922,8.29977652068187));
#24200=CARTESIAN_POINT('Ctrl Pts',(2.65477352494775,-2.90415835883867,8.30562917650306));
#24201=CARTESIAN_POINT('Ctrl Pts',(2.73934042928356,-2.82452798202587,8.31148183232425));
#24202=CARTESIAN_POINT('Ctrl Pts',(2.82019183635457,-2.74135131024082,8.31733448814544));
#24203=CARTESIAN_POINT('Ctrl Pts',(2.9010702435716,-2.6581468617928,8.32318909844791));
#24204=CARTESIAN_POINT('Ctrl Pts',(2.97823039841043,-2.57139405961669,8.32904370875039));
#24205=CARTESIAN_POINT('Ctrl Pts',(3.05136098149761,-2.48146834769133,8.33489831905286));
#24206=CARTESIAN_POINT('Ctrl Pts',(3.12457489228793,-2.3914401710691,8.34075960031581));
#24207=CARTESIAN_POINT('Ctrl Pts',(3.19374980604273,-2.29823218935168,8.34662088157875));
#24208=CARTESIAN_POINT('Ctrl Pts',(3.25861615586611,-2.2022510639635,8.3524821628417));
#24209=CARTESIAN_POINT('Ctrl Pts',(3.32352626626546,-2.10620518713886,8.35834739828188));
#24210=CARTESIAN_POINT('Ctrl Pts',(3.38412180944998,-2.00738279280494,8.36421263372207));
#24211=CARTESIAN_POINT('Ctrl Pts',(3.44017871465808,-1.90621599280183,8.37007786916226));
#24212=CARTESIAN_POINT('Ctrl Pts',(3.49631831661629,-1.8048999486414,8.37595175716554));
#24213=CARTESIAN_POINT('Ctrl Pts',(3.54790573413224,-1.70123296475599,8.38182564516883));
#24214=CARTESIAN_POINT('Ctrl Pts',(3.59476458326332,-1.59566807040679,8.38769953317212));
#24215=CARTESIAN_POINT('Ctrl Pts',(3.60761108615397,-1.56672711804547,8.3893098782961));
#24216=CARTESIAN_POINT('Ctrl Pts',(3.62010247822007,-1.53764360972564,8.39092022342007));
#24217=CARTESIAN_POINT('Ctrl Pts',(3.63223578236975,-1.5084270685959,8.39253056854406));
#24218=CARTESIAN_POINT('Ctrl Pts',(3.68161746855028,-1.38951782116001,8.39908455883176));
#24219=CARTESIAN_POINT('Ctrl Pts',(3.72520412016676,-1.26806629056107,8.40563854911947));
#24220=CARTESIAN_POINT('Ctrl Pts',(3.76275585153874,-1.14462107341731,8.41219253940718));
#24221=CARTESIAN_POINT('Ctrl Pts',(3.80019800167,-1.02153608680251,8.4187274042282));
#24222=CARTESIAN_POINT('Ctrl Pts',(3.83164026942457,-0.896469241021658,
8.42526226904922));
#24223=CARTESIAN_POINT('Ctrl Pts',(3.85689102631617,-0.769987409716397,
8.43179713387024));
#24224=CARTESIAN_POINT('Ctrl Pts',(3.88203237318332,-0.644053616646821,
8.43830368351153));
#24225=CARTESIAN_POINT('Ctrl Pts',(3.90103563430197,-0.516717295157309,
8.4448102331528));
#24226=CARTESIAN_POINT('Ctrl Pts',(3.91375931073664,-0.388557663188167,
8.45131678279408));
#24227=CARTESIAN_POINT('Ctrl Pts',(3.92648298717131,-0.260398031219027,
8.45782333243537));
#24228=CARTESIAN_POINT('Ctrl Pts',(3.93292693640676,-0.131415309978197,
8.46432988207665));
#24229=CARTESIAN_POINT('Ctrl Pts',(3.93299938180971,-0.00220514953339285,
8.47083643171793));
#24230=CARTESIAN_POINT('',(3.93299870264977,0.00319451955702668,9.72083652192225));
#24231=CARTESIAN_POINT('Ctrl Pts',(3.92766918394753,-0.00220124385136065,
8.47083647796505));
#24232=CARTESIAN_POINT('Ctrl Pts',(3.92369425708854,0.795208744126929,8.51104548761253));
#24233=CARTESIAN_POINT('Ctrl Pts',(3.29976413746548,2.91342972784538,8.61756547671448));
#24234=CARTESIAN_POINT('Ctrl Pts',(-0.165076056764658,4.64938694469499,
8.79039644527095));
#24235=CARTESIAN_POINT('Ctrl Pts',(-4.00140116403964,2.37342693484846,8.98932938363437));
#24236=CARTESIAN_POINT('Ctrl Pts',(-4.15924136175396,-2.08449287814342,
9.18826232199783));
#24237=CARTESIAN_POINT('Ctrl Pts',(-0.493461012700928,-4.62609887161364,
9.38719526036124));
#24238=CARTESIAN_POINT('Ctrl Pts',(3.18264251973689,-3.09907510464914,9.56471997901699));
#24239=CARTESIAN_POINT('Ctrl Pts',(3.92290577835605,-0.886171555639169,
9.67593371821826));
#24240=CARTESIAN_POINT('Ctrl Pts',(3.92964724161972,0.00319092675375862,
9.72083647796504));
#24241=CARTESIAN_POINT('',(3.93299988442888,0.000953458131951196,10.9708364779374));
#24242=CARTESIAN_POINT('Ctrl Pts',(3.93299870264977,0.00319451955702668,
9.72083652192224));
#24243=CARTESIAN_POINT('Ctrl Pts',(3.93288780561851,0.139727689034319,9.72772407767723));
#24244=CARTESIAN_POINT('Ctrl Pts',(3.92566347168156,0.275958603419552,9.73461163343222));
#24245=CARTESIAN_POINT('Ctrl Pts',(3.91144310631301,0.411219924221101,9.7414991891872));
#24246=CARTESIAN_POINT('Ctrl Pts',(3.89645310508584,0.553801870061144,9.74875951383735));
#24247=CARTESIAN_POINT('Ctrl Pts',(3.87368900560028,0.695306167485196,9.75601983848751));
#24248=CARTESIAN_POINT('Ctrl Pts',(3.84334558860368,0.834975261047055,9.76328016313766));
#24249=CARTESIAN_POINT('Ctrl Pts',(3.81300217160709,0.974644354608916,9.77054048778781));
#24250=CARTESIAN_POINT('Ctrl Pts',(3.77507959544271,1.11247819590628,9.77780081243797));
#24251=CARTESIAN_POINT('Ctrl Pts',(3.72982868428875,1.24774475989957,9.78506113708812));
#24252=CARTESIAN_POINT('Ctrl Pts',(3.69322985994942,1.35714802026115,9.79093326959863));
#24253=CARTESIAN_POINT('Ctrl Pts',(3.65175207701635,1.4651230498948,9.79680540210914));
#24254=CARTESIAN_POINT('Ctrl Pts',(3.60552515296765,1.57120252396614,9.80267753461965));
#24255=CARTESIAN_POINT('Ctrl Pts',(3.55935816232143,1.67714446555086,9.80854205388554));
#24256=CARTESIAN_POINT('Ctrl Pts',(3.5084544387876,1.78119536335366,9.81440657315142));
#24257=CARTESIAN_POINT('Ctrl Pts',(3.45299339963115,1.88290349782024,9.82027109241731));
#24258=CARTESIAN_POINT('Ctrl Pts',(3.39758942858733,1.98450697699438,9.82612957722998));
#24259=CARTESIAN_POINT('Ctrl Pts',(3.33763766603066,2.08377212695668,9.83198806204266));
#24260=CARTESIAN_POINT('Ctrl Pts',(3.27336512418679,2.18026827793224,9.83784654685533));
#24261=CARTESIAN_POINT('Ctrl Pts',(3.20655836550377,2.28056919784488,9.8439360272135));
#24262=CARTESIAN_POINT('Ctrl Pts',(3.13508326984826,2.37787785054927,9.85002550757168));
#24263=CARTESIAN_POINT('Ctrl Pts',(3.05924697979565,2.47173965388979,9.85611498792985));
#24264=CARTESIAN_POINT('Ctrl Pts',(2.98637200739073,2.56193626455693,9.86196668126499));
#24265=CARTESIAN_POINT('Ctrl Pts',(2.90947033265802,2.64894981354038,9.86781837460013));
#24266=CARTESIAN_POINT('Ctrl Pts',(2.82885746948552,2.73240817180303,9.87367006793527));
#24267=CARTESIAN_POINT('Ctrl Pts',(2.74825690110632,2.81585380128738,9.87952086879051));
#24268=CARTESIAN_POINT('Ctrl Pts',(2.66394655684131,2.8957450208958,9.88537166964574));
#24269=CARTESIAN_POINT('Ctrl Pts',(2.5762799669011,2.97174536798563,9.89122247050098));
#24270=CARTESIAN_POINT('Ctrl Pts',(2.4886055139896,3.04775253168082,9.89707379612488));
#24271=CARTESIAN_POINT('Ctrl Pts',(2.39757452937672,3.11986785830091,9.90292512174879));
#24272=CARTESIAN_POINT('Ctrl Pts',(2.30357433103063,3.18779458268828,9.90877644737269));
#24273=CARTESIAN_POINT('Ctrl Pts',(2.20954293401993,3.2557438519546,9.91462971505149));
#24274=CARTESIAN_POINT('Ctrl Pts',(2.11254069861223,3.31950151266318,9.92048298273028));
#24275=CARTESIAN_POINT('Ctrl Pts',(2.01298406674388,3.3788140148631,9.92633625040908));
#24276=CARTESIAN_POINT('Ctrl Pts',(1.91331417045744,3.43819399620449,9.9321961772822));
#24277=CARTESIAN_POINT('Ctrl Pts',(1.81108443256838,3.49311851327191,9.93805610415533));
#24278=CARTESIAN_POINT('Ctrl Pts',(1.70673613336183,3.54337985136749,9.94391603102845));
#24279=CARTESIAN_POINT('Ctrl Pts',(1.60231757367317,3.59367503175733,9.94977990354601));
#24280=CARTESIAN_POINT('Ctrl Pts',(1.49577799136053,3.63930061878401,9.95564377606358));
#24281=CARTESIAN_POINT('Ctrl Pts',(1.38757725451918,3.68009760233897,9.96150764858114));
#24282=CARTESIAN_POINT('Ctrl Pts',(1.27921689725041,3.72095477062226,9.9673801716298));
#24283=CARTESIAN_POINT('Ctrl Pts',(1.1691908859848,3.75696899057257,9.97325269467845));
#24284=CARTESIAN_POINT('Ctrl Pts',(1.05797287258894,3.78803146777662,9.9791252177271));
#24285=CARTESIAN_POINT('Ctrl Pts',(1.02723624376487,3.79661601090075,9.98074817030192));
#24286=CARTESIAN_POINT('Ctrl Pts',(0.996408622409986,3.80482265792298,9.98237112287675));
#24287=CARTESIAN_POINT('Ctrl Pts',(0.965500099630154,3.81264980789138,9.98399407545157));
#24288=CARTESIAN_POINT('Ctrl Pts',(0.853667681362951,3.84096979960826,9.98986620051131));
#24289=CARTESIAN_POINT('Ctrl Pts',(0.740400701749089,3.86441270438932,9.99573832557106));
#24290=CARTESIAN_POINT('Ctrl Pts',(0.626162532712097,3.88283523763597,10.0016104506308));
#24291=CARTESIAN_POINT('Ctrl Pts',(0.512072474938538,3.90123388583003,10.0074749624045));
#24292=CARTESIAN_POINT('Ctrl Pts',(0.39701413612062,3.91462504127279,10.0133394741781));
#24293=CARTESIAN_POINT('Ctrl Pts',(0.281464558483938,3.92291558694773,10.0192039859518));
#24294=CARTESIAN_POINT('Ctrl Pts',(0.166033879447143,3.9311976017886,10.0250624632401));
#24295=CARTESIAN_POINT('Ctrl Pts',(0.0501133768782267,3.93438941685644,
10.0309209405284));
#24296=CARTESIAN_POINT('Ctrl Pts',(-0.0658119012407749,3.93244933770991,
10.0367794178166));
#24297=CARTESIAN_POINT('Ctrl Pts',(-0.1863082341534,3.93043275921632,10.0428689009832));
#24298=CARTESIAN_POINT('Ctrl Pts',(-0.306809277726285,3.92287117608799,
10.0489583841498));
#24299=CARTESIAN_POINT('Ctrl Pts',(-0.426766562019581,3.90977739795273,
10.0550478673164));
#24300=CARTESIAN_POINT('Ctrl Pts',(-0.542039453875697,3.89719493845586,
10.0608995530949));
#24301=CARTESIAN_POINT('Ctrl Pts',(-0.656809807979611,3.87950429505613,
10.0667512388734));
#24302=CARTESIAN_POINT('Ctrl Pts',(-0.770594013171069,3.85676987476112,
10.0726029246518));
#24303=CARTESIAN_POINT('Ctrl Pts',(-0.884360864389838,3.83403892184111,
10.0784537179515));
#24304=CARTESIAN_POINT('Ctrl Pts',(-0.997141460458635,3.80626580253215,
10.0843045112511));
#24305=CARTESIAN_POINT('Ctrl Pts',(-1.10846165934521,3.77356618462717,10.0901553045507));
#24306=CARTESIAN_POINT('Ctrl Pts',(-1.21979184292451,3.74086363378064,10.0960066226282));
#24307=CARTESIAN_POINT('Ctrl Pts',(-1.32966097225197,3.7032338224534,10.1018579407057));
#24308=CARTESIAN_POINT('Ctrl Pts',(-1.43761005126368,3.66084229932206,10.1077092587831));
#24309=CARTESIAN_POINT('Ctrl Pts',(-1.54559495893886,3.6184367063012,10.1135625189328));
#24310=CARTESIAN_POINT('Ctrl Pts',(-1.65165816452456,3.5712664099305,10.1194157790825));
#24311=CARTESIAN_POINT('Ctrl Pts',(-1.75536129796696,3.51954481625107,10.1252690392322));
#24312=CARTESIAN_POINT('Ctrl Pts',(-1.85918241454032,3.46776437887658,10.1311289586402));
#24313=CARTESIAN_POINT('Ctrl Pts',(-1.96063772949673,3.41142249363674,10.1369888780483));
#24314=CARTESIAN_POINT('Ctrl Pts',(-2.05931401914049,3.35077823357074,10.1428487974563));
#24315=CARTESIAN_POINT('Ctrl Pts',(-2.15805675070839,3.29009313977111,10.1487126625368));
#24316=CARTESIAN_POINT('Ctrl Pts',(-2.25401638956751,3.22510013406245,10.1545765276174));
#24317=CARTESIAN_POINT('Ctrl Pts',(-2.34681065024533,3.15610024744068,10.1604403926979));
#24318=CARTESIAN_POINT('Ctrl Pts',(-2.43974180507728,3.08699856916665,10.1663129084088));
#24319=CARTESIAN_POINT('Ctrl Pts',(-2.5294979425478,3.01387847260215,10.1721854241197));
#24320=CARTESIAN_POINT('Ctrl Pts',(-2.6157315827658,2.93707972089991,10.1780579398306));
#24321=CARTESIAN_POINT('Ctrl Pts',(-2.63956452449162,2.91585435955244,10.1796809644921));
#24322=CARTESIAN_POINT('Ctrl Pts',(-2.66312863249218,2.89434821296909,10.1813039891535));
#24323=CARTESIAN_POINT('Ctrl Pts',(-2.6864171060488,2.87256890819496,10.182927013815));
#24324=CARTESIAN_POINT('Ctrl Pts',(-2.77067505880192,2.79377114464928,10.1887991348413));
#24325=CARTESIAN_POINT('Ctrl Pts',(-2.85160439663599,2.71113096212789,10.1946712558677));
#24326=CARTESIAN_POINT('Ctrl Pts',(-2.92883417188751,2.624960836581,10.200543376894));
#24327=CARTESIAN_POINT('Ctrl Pts',(-3.00596381657239,2.5389024330153,10.206407884551));
#24328=CARTESIAN_POINT('Ctrl Pts',(-3.07940316397512,2.44932349277566,10.2122723922079));
#24329=CARTESIAN_POINT('Ctrl Pts',(-3.14881609273798,2.35657510258306,10.2181368998649));
#24330=CARTESIAN_POINT('Ctrl Pts',(-3.21815759577494,2.26392215024638,10.2239953729585));
#24331=CARTESIAN_POINT('Ctrl Pts',(-3.2834806749253,2.16810656393992,10.2298538460521));
#24332=CARTESIAN_POINT('Ctrl Pts',(-3.34448815197973,2.06951395290469,10.2357123191457));
#24333=CARTESIAN_POINT('Ctrl Pts',(-3.40790127904621,1.96703363289711,10.2418018038554));
#24334=CARTESIAN_POINT('Ctrl Pts',(-3.46665115215085,1.86155311374219,10.2478912885651));
#24335=CARTESIAN_POINT('Ctrl Pts',(-3.52045218427856,1.75354082308008,10.2539807732748));
#24336=CARTESIAN_POINT('Ctrl Pts',(-3.57215220731775,1.64974657053688,10.2598324546894));
#24337=CARTESIAN_POINT('Ctrl Pts',(-3.61928245327851,1.54361497941328,10.265684136104));
#24338=CARTESIAN_POINT('Ctrl Pts',(-3.66163579849187,1.43558778178236,10.2715358175186));
#24339=CARTESIAN_POINT('Ctrl Pts',(-3.70398268371517,1.3275770611173,10.2773866063991));
#24340=CARTESIAN_POINT('Ctrl Pts',(-3.74155396602138,1.21767169360762,10.2832373952797));
#24341=CARTESIAN_POINT('Ctrl Pts',(-3.774190771307,1.10633314231341,10.2890881841602));
#24342=CARTESIAN_POINT('Ctrl Pts',(-3.8068305036193,0.994984605638975,10.2949394977678));
#24343=CARTESIAN_POINT('Ctrl Pts',(-3.83453476286883,0.882203026408219,
10.3007908113754));
#24344=CARTESIAN_POINT('Ctrl Pts',(-3.85719483088805,0.768464076304509,
10.306642124983));
#24345=CARTESIAN_POINT('Ctrl Pts',(-3.87986241968654,0.654687376731623,
10.3124953806165));
#24346=CARTESIAN_POINT('Ctrl Pts',(-3.8974824075923,0.539953079696709,10.3183486362499));
#24347=CARTESIAN_POINT('Ctrl Pts',(-3.90999749083604,0.424745360958616,
10.3242018918834));
#24348=CARTESIAN_POINT('Ctrl Pts',(-3.92252681241093,0.309406571126669,
10.3300618067288));
#24349=CARTESIAN_POINT('Ctrl Pts',(-3.92993959240011,0.193593695783005,
10.3359217215742));
#24350=CARTESIAN_POINT('Ctrl Pts',(-3.93223054093183,0.0777944275827514,
10.3417816364196));
#24351=CARTESIAN_POINT('Ctrl Pts',(-3.93452303202141,-0.0380828114091053,
10.3476454969048));
#24352=CARTESIAN_POINT('Ctrl Pts',(-3.9316868347727,-0.15394601273332,10.35350935739));
#24353=CARTESIAN_POINT('Ctrl Pts',(-3.92376868189452,-0.269310844534226,
10.3593732178752));
#24354=CARTESIAN_POINT('Ctrl Pts',(-3.91583884781867,-0.384845867467452,
10.3652457289781));
#24355=CARTESIAN_POINT('Ctrl Pts',(-3.9028121416016,-0.499880644273067,
10.371118240081));
#24356=CARTESIAN_POINT('Ctrl Pts',(-3.88478669393042,-0.613939201111262,
10.3769907511839));
#24357=CARTESIAN_POINT('Ctrl Pts',(-3.87980475200986,-0.645463139716109,
10.3786138181821));
#24358=CARTESIAN_POINT('Ctrl Pts',(-3.87444126192626,-0.676912588316585,
10.3802368851803));
#24359=CARTESIAN_POINT('Ctrl Pts',(-3.86869896686081,-0.708277702465682,
10.3818599521785));
#24360=CARTESIAN_POINT('Ctrl Pts',(-3.84792380704504,-0.821754152501958,
10.3877320775037));
#24361=CARTESIAN_POINT('Ctrl Pts',(-3.82211685801432,-0.93450600488425,
10.393604202829));
#24362=CARTESIAN_POINT('Ctrl Pts',(-3.79134061016334,-1.04605228250135,
10.3994763281542));
#24363=CARTESIAN_POINT('Ctrl Pts',(-3.76060426424535,-1.15745393845705,
10.4053408401683));
#24364=CARTESIAN_POINT('Ctrl Pts',(-3.72491154079952,-1.26765273314512,
10.4112053521824));
#24365=CARTESIAN_POINT('Ctrl Pts',(-3.68437623724042,-1.37617613060905,
10.4170698641965));
#24366=CARTESIAN_POINT('Ctrl Pts',(-3.64388264400972,-1.48458785883285,
10.4229283416999));
#24367=CARTESIAN_POINT('Ctrl Pts',(-3.59855652578488,-1.59132723393031,
10.4287868192034));
#24368=CARTESIAN_POINT('Ctrl Pts',(-3.54856177149421,-1.69593583424901,
10.4346452967068));
#24369=CARTESIAN_POINT('Ctrl Pts',(-3.49659567450274,-1.80466925533351,
10.4407347797832));
#24370=CARTESIAN_POINT('Ctrl Pts',(-3.43958531012525,-1.91109996885889,
10.4468242628597));
#24371=CARTESIAN_POINT('Ctrl Pts',(-3.37777051672664,-2.01473455728845,
10.4529137459362));
#24372=CARTESIAN_POINT('Ctrl Pts',(-3.31836961977622,-2.11432216681269,
10.4587654318647));
#24373=CARTESIAN_POINT('Ctrl Pts',(-3.25453271454795,-2.21132754472085,
10.4646171177932));
#24374=CARTESIAN_POINT('Ctrl Pts',(-3.18651957473406,-2.30533771925865,
10.4704688037218));
#24375=CARTESIAN_POINT('Ctrl Pts',(-3.1185168083319,-2.39933355529877,10.4763195971471));
#24376=CARTESIAN_POINT('Ctrl Pts',(-3.04633931608047,-2.49033476143605,
10.4821703905724));
#24377=CARTESIAN_POINT('Ctrl Pts',(-2.97028954566743,-2.57795830356094,
10.4880211839977));
#24378=CARTESIAN_POINT('Ctrl Pts',(-2.89423295440869,-2.66558970457424,
10.4938725021762));
#24379=CARTESIAN_POINT('Ctrl Pts',(-2.81430366557959,-2.7498425271212,10.4997238203546));
#24380=CARTESIAN_POINT('Ctrl Pts',(-2.7308431842205,-2.83036826282313,10.5055751385331));
#24381=CARTESIAN_POINT('Ctrl Pts',(-2.64735500240226,-2.91092072494476,
10.5114283987589));
#24382=CARTESIAN_POINT('Ctrl Pts',(-2.56033359496256,-2.98774335359664,
10.5172816589847));
#24383=CARTESIAN_POINT('Ctrl Pts',(-2.47015540426082,-3.0605263074839,10.5231349192104));
#24384=CARTESIAN_POINT('Ctrl Pts',(-2.37987461834705,-3.13339206612173,
10.5289948386569));
#24385=CARTESIAN_POINT('Ctrl Pts',(-2.28643020261903,-3.20220871686826,
10.5348547581033));
#24386=CARTESIAN_POINT('Ctrl Pts',(-2.19022966427678,-3.26670828476037,
10.5407146775498));
#24387=CARTESIAN_POINT('Ctrl Pts',(-2.09396435137341,-3.33125128204772,
10.5465785426468));
#24388=CARTESIAN_POINT('Ctrl Pts',(-1.99493957300605,-3.39147119416107,
10.5524424077439));
#24389=CARTESIAN_POINT('Ctrl Pts',(-1.89358811873438,-3.44714563611519,
10.5583062728409));
#24390=CARTESIAN_POINT('Ctrl Pts',(-1.79208714692477,-3.50290221113338,
10.5641787885358));
#24391=CARTESIAN_POINT('Ctrl Pts',(-1.6882530181765,-3.55409975061671,10.5700513042307));
#24392=CARTESIAN_POINT('Ctrl Pts',(-1.58253926204241,-3.60056363422371,
10.5759238199256));
#24393=CARTESIAN_POINT('Ctrl Pts',(-1.55332249643609,-3.61340514554777,
10.5775468434643));
#24394=CARTESIAN_POINT('Ctrl Pts',(-1.52396224897608,-3.62588537512602,
10.5791698670031));
#24395=CARTESIAN_POINT('Ctrl Pts',(-1.49446828466722,-3.63800131200139,
10.5807928905419));
#24396=CARTESIAN_POINT('Ctrl Pts',(-1.38775867046928,-3.68183695701938,
10.5866650145413));
#24397=CARTESIAN_POINT('Ctrl Pts',(-1.27893984741821,-3.7210471120347,10.5925371385407));
#24398=CARTESIAN_POINT('Ctrl Pts',(-1.16845029605637,-3.75542446411132,
10.5984092625401));
#24399=CARTESIAN_POINT('Ctrl Pts',(-1.05810399651562,-3.78975724529205,
10.6042737732182));
#24400=CARTESIAN_POINT('Ctrl Pts',(-0.946091667411633,-3.81926956229493,
10.6101382838963));
#24401=CARTESIAN_POINT('Ctrl Pts',(-0.832872410197733,-3.84380183520579,
10.6160027945744));
#24402=CARTESIAN_POINT('Ctrl Pts',(-0.719769654396316,-3.86830886466853,
10.6218612707333));
#24403=CARTESIAN_POINT('Ctrl Pts',(-0.605462842319242,-3.88784595571986,
10.6277197468922));
#24404=CARTESIAN_POINT('Ctrl Pts',(-0.490426265907847,-3.90230330416636,
10.6335782230512));
#24405=CARTESIAN_POINT('Ctrl Pts',(-0.370853646025683,-3.91733072487223,
10.6396677066284));
#24406=CARTESIAN_POINT('Ctrl Pts',(-0.25049296118244,-3.92686942434664,
10.6457571902057));
#24407=CARTESIAN_POINT('Ctrl Pts',(-0.129888989929251,-3.93085459541499,
10.6518466737829));
#24408=CARTESIAN_POINT('Ctrl Pts',(-0.0139946962873338,-3.93468414249548,
10.6576983583543));
#24409=CARTESIAN_POINT('Ctrl Pts',(0.102123787176804,-3.93338574595293,
10.6635500429257));
#24410=CARTESIAN_POINT('Ctrl Pts',(0.217978600822607,-3.92695484180598,
10.6694017274971));
#24411=CARTESIAN_POINT('Ctrl Pts',(0.33381574416035,-3.92052491850784,10.6752525195629));
#24412=CARTESIAN_POINT('Ctrl Pts',(0.44938888497686,-3.9089640669948,10.6811033116287));
#24413=CARTESIAN_POINT('Ctrl Pts',(0.564212295612798,-3.89231980770842,
10.6869541036945));
#24414=CARTESIAN_POINT('Ctrl Pts',(0.679046004657021,-3.87567405561342,
10.6928054205125));
#24415=CARTESIAN_POINT('Ctrl Pts',(0.793129440687579,-3.85394404871565,
10.6986567373306));
#24416=CARTESIAN_POINT('Ctrl Pts',(0.905984822881521,-3.82722882784768,
10.7045080541487));
#24417=CARTESIAN_POINT('Ctrl Pts',(1.01887766169491,-3.8005047402173,10.7103613130145));
#24418=CARTESIAN_POINT('Ctrl Pts',(1.13054123412321,-3.7687922437558,10.7162145718804));
#24419=CARTESIAN_POINT('Ctrl Pts',(1.24051141714121,-3.73224067068863,10.7220678307463));
#24420=CARTESIAN_POINT('Ctrl Pts',(1.35060671278147,-3.695647513048,10.7279277488405));
#24421=CARTESIAN_POINT('Ctrl Pts',(1.45900438110027,-3.65420442064697,10.7337876669348));
#24422=CARTESIAN_POINT('Ctrl Pts',(1.56525874133763,-3.6081094873446,10.7396475850291));
#24423=CARTESIAN_POINT('Ctrl Pts',(1.67158464572791,-3.56198351698221,10.7455114487767));
#24424=CARTESIAN_POINT('Ctrl Pts',(1.77576399773429,-3.51119964956191,10.7513753125244));
#24425=CARTESIAN_POINT('Ctrl Pts',(1.87737581664801,-3.45600188701702,10.757239176272));
#24426=CARTESIAN_POINT('Ctrl Pts',(1.97913753748759,-3.40072269446727,10.7631116906321));
#24427=CARTESIAN_POINT('Ctrl Pts',(2.07832381276221,-3.34101682334,10.7689842049923));
#24428=CARTESIAN_POINT('Ctrl Pts',(2.17454264612672,-3.27717153658093,10.7748567193524));
#24429=CARTESIAN_POINT('Ctrl Pts',(2.20113545981049,-3.25952607408671,10.77647975587));
#24430=CARTESIAN_POINT('Ctrl Pts',(2.22750180242423,-3.24156465711916,10.7781027923877));
#24431=CARTESIAN_POINT('Ctrl Pts',(2.25363386373655,-3.22329387555957,10.7797258289053));
#24432=CARTESIAN_POINT('Ctrl Pts',(2.3475878928883,-3.15760393542214,10.7855612208581));
#24433=CARTESIAN_POINT('Ctrl Pts',(2.43883457827334,-3.08768560540386,10.7913966128109));
#24434=CARTESIAN_POINT('Ctrl Pts',(2.52696543690863,-3.01379074931707,10.7972320047637));
#24435=CARTESIAN_POINT('Ctrl Pts',(2.61498173994283,-2.93999194437274,10.803059811668));
#24436=CARTESIAN_POINT('Ctrl Pts',(2.69988995004763,-2.86222715618575,10.8088876185723));
#24437=CARTESIAN_POINT('Ctrl Pts',(2.7813103475408,-2.78079156907929,10.8147154254767));
#24438=CARTESIAN_POINT('Ctrl Pts',(2.86264740219996,-2.69943934035511,10.8205372669723));
#24439=CARTESIAN_POINT('Ctrl Pts',(2.94050344911103,-2.61442407917905,10.826359108468));
#24440=CARTESIAN_POINT('Ctrl Pts',(3.01453226499092,-2.52608080300862,10.8321809499637));
#24441=CARTESIAN_POINT('Ctrl Pts',(3.08850724603668,-2.43780177135654,10.8379985577314));
#24442=CARTESIAN_POINT('Ctrl Pts',(3.15866026295215,-2.34619985805649,10.8438161654991));
#24443=CARTESIAN_POINT('Ctrl Pts',(3.22468287120717,-2.25164592690393,10.8496337732667));
#24444=CARTESIAN_POINT('Ctrl Pts',(3.29068011935583,-2.15712831509433,10.8554491464188));
#24445=CARTESIAN_POINT('Ctrl Pts',(3.35254987236369,-2.05966128217619,10.8612645195708));
#24446=CARTESIAN_POINT('Ctrl Pts',(3.41002522892359,-1.95964714632625,10.8670798927229));
#24447=CARTESIAN_POINT('Ctrl Pts',(3.4674928737749,-1.85964642979055,10.8728944856021));
#24448=CARTESIAN_POINT('Ctrl Pts',(3.5205670856315,-1.75709965315912,10.8787090784812));
#24449=CARTESIAN_POINT('Ctrl Pts',(3.56902582108089,-1.65243568360704,10.8845236713604));
#24450=CARTESIAN_POINT('Ctrl Pts',(3.61749016656738,-1.54775959717354,10.8903389373913));
#24451=CARTESIAN_POINT('Ctrl Pts',(3.66133779794951,-1.44096621124018,10.8961542034221));
#24452=CARTESIAN_POINT('Ctrl Pts',(3.70039424991618,-1.33250568298497,10.901969469453));
#24453=CARTESIAN_POINT('Ctrl Pts',(3.73948958897038,-1.22393716452989,10.9077905255326));
#24454=CARTESIAN_POINT('Ctrl Pts',(3.77378407801915,-1.11369858340012,10.9136115816122));
#24455=CARTESIAN_POINT('Ctrl Pts',(3.80315269796462,-1.00225673156352,10.9194326376918));
#24456=CARTESIAN_POINT('Ctrl Pts',(3.83253583908598,-0.890759777827898,
10.9252565719652));
#24457=CARTESIAN_POINT('Ctrl Pts',(3.85698817143527,-0.778058778113033,
10.9310805062385));
#24458=CARTESIAN_POINT('Ctrl Pts',(3.87643592228907,-0.664630378772178,
10.9369044405119));
#24459=CARTESIAN_POINT('Ctrl Pts',(3.89591544239246,-0.551016686275567,
10.9427378885858));
#24460=CARTESIAN_POINT('Ctrl Pts',(3.91037399450792,-0.436673636291081,
10.9485713366596));
#24461=CARTESIAN_POINT('Ctrl Pts',(3.91978972160551,-0.322083123425976,
10.9544047847335));
#24462=CARTESIAN_POINT('Ctrl Pts',(3.92863048136433,-0.214490031104953,
10.9598820158014));
#24463=CARTESIAN_POINT('Ctrl Pts',(3.93302597726497,-0.106679082682813,
10.9653592468694));
#24464=CARTESIAN_POINT('Ctrl Pts',(3.93299988442888,0.000953458131958574,
10.9708364779374));
#24465=CARTESIAN_POINT('',(3.93299831367774,-0.00364206096290877,12.2208364640931));
#24466=CARTESIAN_POINT('Ctrl Pts',(3.93299988442875,0.000953458676826257,
10.9708364779651));
#24467=CARTESIAN_POINT('Ctrl Pts',(3.93298746295601,0.0521918102145222,
10.973443907733));
#24468=CARTESIAN_POINT('Ctrl Pts',(3.93197379978628,0.103416823419383,10.9760513375009));
#24469=CARTESIAN_POINT('Ctrl Pts',(3.92996019662714,0.154602241013298,10.9786587672688));
#24470=CARTESIAN_POINT('Ctrl Pts',(3.92542541377817,0.269875577156574,10.9845308914447));
#24471=CARTESIAN_POINT('Ctrl Pts',(3.91580694317262,0.385142477321062,10.9904030156205));
#24472=CARTESIAN_POINT('Ctrl Pts',(3.90109869562193,0.499917960286333,10.9962751397964));
#24473=CARTESIAN_POINT('Ctrl Pts',(3.88640951759966,0.614544634610346,11.0021396506493));
#24474=CARTESIAN_POINT('Ctrl Pts',(3.86664373770084,0.728680752490247,11.0080041615022));
#24475=CARTESIAN_POINT('Ctrl Pts',(3.84184725169761,0.841842440497926,11.0138686723551));
#24476=CARTESIAN_POINT('Ctrl Pts',(3.81707628102204,0.954887686298954,11.019727148687));
#24477=CARTESIAN_POINT('Ctrl Pts',(3.78728498859164,1.06696009520279,11.0255856250189));
#24478=CARTESIAN_POINT('Ctrl Pts',(3.75257085333169,1.17758268954901,11.0314441013508));
#24479=CARTESIAN_POINT('Ctrl Pts',(3.71648789552596,1.29256727361729,11.0375335848625));
#24480=CARTESIAN_POINT('Ctrl Pts',(3.67508593781408,1.4059849034682,11.0436230683742));
#24481=CARTESIAN_POINT('Ctrl Pts',(3.62853270265492,1.51731322598988,11.0497125518859));
#24482=CARTESIAN_POINT('Ctrl Pts',(3.58379740528761,1.62429409630713,11.0555642366245));
#24483=CARTESIAN_POINT('Ctrl Pts',(3.53430577746659,1.72934535777942,11.061415921363));
#24484=CARTESIAN_POINT('Ctrl Pts',(3.4802566423204,1.83202148011008,11.0672676061016));
#24485=CARTESIAN_POINT('Ctrl Pts',(3.42621575083215,1.93468194211929,11.0731183983321));
#24486=CARTESIAN_POINT('Ctrl Pts',(3.3676189266489,2.03496761955094,11.0789691905626));
#24487=CARTESIAN_POINT('Ctrl Pts',(3.30471146846356,2.13245659046214,11.0848199827931));
#24488=CARTESIAN_POINT('Ctrl Pts',(3.24179836819332,2.22995430502739,11.0906712997732));
#24489=CARTESIAN_POINT('Ctrl Pts',(3.17457408953004,2.32465446704812,11.0965226167534));
#24490=CARTESIAN_POINT('Ctrl Pts',(3.10332747457054,2.4161638159644,11.1023739337335));
#24491=CARTESIAN_POINT('Ctrl Pts',(3.03205721294617,2.5077035367223,11.1082271927586));
#24492=CARTESIAN_POINT('Ctrl Pts',(2.95676221428615,2.5960500125395,11.1140804517838));
#24493=CARTESIAN_POINT('Ctrl Pts',(2.87777137047377,2.6808433261348,11.1199337108089));
#24494=CARTESIAN_POINT('Ctrl Pts',(2.79869065917546,2.76573310865675,11.1257936290574));
#24495=CARTESIAN_POINT('Ctrl Pts',(2.71590599212807,2.8470613577299,11.1316535473059));
#24496=CARTESIAN_POINT('Ctrl Pts',(2.62978292935532,2.92450521361672,11.1375134655545));
#24497=CARTESIAN_POINT('Ctrl Pts',(2.54360187745987,3.00200121466787,11.1433773294536));
#24498=CARTESIAN_POINT('Ctrl Pts',(2.45407827250996,3.0756073526987,11.1492411933528));
#24499=CARTESIAN_POINT('Ctrl Pts',(2.36160914426483,3.14504232876518,11.1551050572519));
#24500=CARTESIAN_POINT('Ctrl Pts',(2.26900360185219,3.21457973809384,11.1609775717583));
#24501=CARTESIAN_POINT('Ctrl Pts',(2.17344420358745,3.27993347178056,11.1668500862648));
#24502=CARTESIAN_POINT('Ctrl Pts',(2.07535525939748,3.34086658627537,11.1727226007712));
#24503=CARTESIAN_POINT('Ctrl Pts',(2.04824561414862,3.35770717041565,11.1743456357248));
#24504=CARTESIAN_POINT('Ctrl Pts',(2.02094288146688,3.37421036303248,11.1759686706785));
#24505=CARTESIAN_POINT('Ctrl Pts',(1.99345630321953,3.39037180367498,11.1775917056321));
#24506=CARTESIAN_POINT('Ctrl Pts',(1.89401014270427,3.44884373153116,11.1834638295856));
#24507=CARTESIAN_POINT('Ctrl Pts',(1.79182243863439,3.5030345546962,11.189335953539));
#24508=CARTESIAN_POINT('Ctrl Pts',(1.68729798416334,3.55267709096089,11.1952080774924));
#24509=CARTESIAN_POINT('Ctrl Pts',(1.58290904771732,3.60225526469429,11.2010725881208));
#24510=CARTESIAN_POINT('Ctrl Pts',(1.47618975571495,3.6472967026905,11.2069370987492));
#24511=CARTESIAN_POINT('Ctrl Pts',(1.36757205912588,3.68757856365097,11.2128016093776));
#24512=CARTESIAN_POINT('Ctrl Pts',(1.25906612905989,3.72781897497954,11.2186600854833));
#24513=CARTESIAN_POINT('Ctrl Pts',(1.14866606517241,3.76330940786109,11.224518561589));
#24514=CARTESIAN_POINT('Ctrl Pts',(1.03682588888875,3.79387415133002,11.2303770376946));
#24515=CARTESIAN_POINT('Ctrl Pts',(0.920575705981865,3.82564410320985,11.2364665212905));
#24516=CARTESIAN_POINT('Ctrl Pts',(0.80276991414309,3.85209172587159,11.2425560048864));
#24517=CARTESIAN_POINT('Ctrl Pts',(0.683938671616597,3.87307589565029,11.2486454884822));
#24518=CARTESIAN_POINT('Ctrl Pts',(0.569747881842849,3.89324061722376,11.2544971729917));
#24519=CARTESIAN_POINT('Ctrl Pts',(0.454610673223435,3.90836050409038,11.2603488575011));
#24520=CARTESIAN_POINT('Ctrl Pts',(0.339009367172975,3.91836211304787,11.2662005420105));
#24521=CARTESIAN_POINT('Ctrl Pts',(0.223425692827235,3.92836219654322,11.2720513340112));
#24522=CARTESIAN_POINT('Ctrl Pts',(0.107378473553437,3.9332455186781,11.2779021260119));
#24523=CARTESIAN_POINT('Ctrl Pts',(-0.00864472132234088,3.93299049945372,
11.2837529180126));
#24524=CARTESIAN_POINT('Ctrl Pts',(-0.124678322153347,3.93273545735704,
11.2896042347625));
#24525=CARTESIAN_POINT('Ctrl Pts',(-0.240687480866707,3.92734115868139,
11.2954555515124));
#24526=CARTESIAN_POINT('Ctrl Pts',(-0.356185216441638,3.91683814978209,
11.3013068682623));
#24527=CARTESIAN_POINT('Ctrl Pts',(-0.471721285572108,3.90633165494714,
11.307160127057));
#24528=CARTESIAN_POINT('Ctrl Pts',(-0.586745182549625,3.89071311576923,
11.3130133858517));
#24529=CARTESIAN_POINT('Ctrl Pts',(-0.700776341970374,3.87006479513388,
11.3188666446464));
#24530=CARTESIAN_POINT('Ctrl Pts',(-0.814937234090088,3.84939298300393,
11.3247265626653));
#24531=CARTESIAN_POINT('Ctrl Pts',(-0.928102727295191,3.82368004144668,
11.3305864806843));
#24532=CARTESIAN_POINT('Ctrl Pts',(-1.03980362440171,3.79305911141404,11.3364463987032));
#24533=CARTESIAN_POINT('Ctrl Pts',(-1.1515797329261,3.76241756343093,11.342310262373));
#24534=CARTESIAN_POINT('Ctrl Pts',(-1.26188888920827,3.7268615732093,11.3481741260429));
#24535=CARTESIAN_POINT('Ctrl Pts',(-1.37027986245381,3.68657321893294,11.3540379897127));
#24536=CARTESIAN_POINT('Ctrl Pts',(-1.47883073845663,3.64622542964329,11.3599105039919));
#24537=CARTESIAN_POINT('Ctrl Pts',(-1.58545740436847,3.6011315031968,11.3657830182711));
#24538=CARTESIAN_POINT('Ctrl Pts',(-1.68973121110186,3.55152043978748,11.3716555325503));
#24539=CARTESIAN_POINT('Ctrl Pts',(-1.71855025757699,3.53780900460674,11.3732785696987));
#24540=CARTESIAN_POINT('Ctrl Pts',(-1.74718974259254,3.52375278790568,11.3749016068472));
#24541=CARTESIAN_POINT('Ctrl Pts',(-1.77564100322541,3.5093572100407,11.3765246439956));
#24542=CARTESIAN_POINT('Ctrl Pts',(-1.87857723494723,3.45727422651317,11.3823967679117));
#24543=CARTESIAN_POINT('Ctrl Pts',(-1.97939255309076,3.40057110844041,11.3882688918278));
#24544=CARTESIAN_POINT('Ctrl Pts',(-2.07764341031177,3.33944409439477,11.3941410157439));
#24545=CARTESIAN_POINT('Ctrl Pts',(-2.17576688333062,3.27839633274584,11.4000055263338));
#24546=CARTESIAN_POINT('Ctrl Pts',(-2.27133215961957,3.21293629766038,11.4058700369238));
#24547=CARTESIAN_POINT('Ctrl Pts',(-2.3639183274651,3.14330703894396,11.4117345475137));
#24548=CARTESIAN_POINT('Ctrl Pts',(-2.45640922505211,3.07374942805173,11.4175930235798));
#24549=CARTESIAN_POINT('Ctrl Pts',(-2.5459267831523,3.00003137370619,11.4234514996459));
#24550=CARTESIAN_POINT('Ctrl Pts',(-2.63207782176324,2.92243996348634,11.429309975712));
#24551=CARTESIAN_POINT('Ctrl Pts',(-2.72162591101277,2.84178902021982,11.4353994593223));
#24552=CARTESIAN_POINT('Ctrl Pts',(-2.8075361396866,2.75695321396994,11.4414889429326));
#24553=CARTESIAN_POINT('Ctrl Pts',(-2.88940329061361,2.66830238619824,11.4475784265429));
#24554=CARTESIAN_POINT('Ctrl Pts',(-2.96807346465768,2.58311344324641,11.4534301110101));
#24555=CARTESIAN_POINT('Ctrl Pts',(-3.04301009918702,2.49440217892352,11.4592817954774));
#24556=CARTESIAN_POINT('Ctrl Pts',(-3.11389077473526,2.40253475375875,11.4651334799447));
#24557=CARTESIAN_POINT('Ctrl Pts',(-3.18476063943358,2.31068134038124,11.4709842719024));
#24558=CARTESIAN_POINT('Ctrl Pts',(-3.25157552269572,2.21567305052555,11.4768350638601));
#24559=CARTESIAN_POINT('Ctrl Pts',(-3.31405380922571,2.11790848469818,11.4826858558178));
#24560=CARTESIAN_POINT('Ctrl Pts',(-3.37653769933548,2.02013515051985,11.4885371725239));
#24561=CARTESIAN_POINT('Ctrl Pts',(-3.43468399689634,1.91960539732049,11.4943884892299));
#24562=CARTESIAN_POINT('Ctrl Pts',(-3.4882552657953,1.81674549693989,11.500239805936));
#24563=CARTESIAN_POINT('Ctrl Pts',(-3.54184431492509,1.71385145749913,11.5060930646861));
#24564=CARTESIAN_POINT('Ctrl Pts',(-3.59085512519853,1.60862609954607,11.5119463234362));
#24565=CARTESIAN_POINT('Ctrl Pts',(-3.63509724361739,1.50151824146271,11.5177995821863));
#24566=CARTESIAN_POINT('Ctrl Pts',(-3.67938969607372,1.39428852730337,11.5236595001596));
#24567=CARTESIAN_POINT('Ctrl Pts',(-3.71890246996207,1.28517242054227,11.529519418133));
#24568=CARTESIAN_POINT('Ctrl Pts',(-3.75349406600832,1.17463666571425,11.5353793361064));
#24569=CARTESIAN_POINT('Ctrl Pts',(-3.78810895356494,1.06402648400304,11.54124319973));
#24570=CARTESIAN_POINT('Ctrl Pts',(-3.81779595967751,0.951995149506696,
11.5471070633536));
#24571=CARTESIAN_POINT('Ctrl Pts',(-3.84246447100285,0.839020732211552,
11.5529709269773));
#24572=CARTESIAN_POINT('Ctrl Pts',(-3.86716937431399,0.725879650485935,
11.5588434412097));
#24573=CARTESIAN_POINT('Ctrl Pts',(-3.88684093686975,0.611793115112664,
11.5647159554422));
#24574=CARTESIAN_POINT('Ctrl Pts',(-3.90144022944247,0.49724554908803,11.5705884696747));
#24575=CARTESIAN_POINT('Ctrl Pts',(-3.90547516222909,0.465587047316269,
11.5722115072361));
#24576=CARTESIAN_POINT('Ctrl Pts',(-3.90912295560159,0.433893334131203,
11.5738345447976));
#24577=CARTESIAN_POINT('Ctrl Pts',(-3.9123834894835,0.402174627763785,11.5754575823591));
#24578=CARTESIAN_POINT('Ctrl Pts',(-3.92418004903791,0.287416854281089,
11.5813297063567));
#24579=CARTESIAN_POINT('Ctrl Pts',(-3.93094300318938,0.171947226972836,
11.5872018303543));
#24580=CARTESIAN_POINT('Ctrl Pts',(-3.93259780548776,0.0562450022034934,
11.5930739543519));
#24581=CARTESIAN_POINT('Ctrl Pts',(-3.93425046230221,-0.0593072123422889,
11.5989384650246));
#24582=CARTESIAN_POINT('Ctrl Pts',(-3.93080813179207,-0.175091015091824,
11.6048029756972));
#24583=CARTESIAN_POINT('Ctrl Pts',(-3.92224788754817,-0.290620901904727,
11.6106674863699));
#24584=CARTESIAN_POINT('Ctrl Pts',(-3.9136964517099,-0.406031909620679,
11.6165259625198));
#24585=CARTESIAN_POINT('Ctrl Pts',(-3.90003760738736,-0.521189111292248,
11.6223844386697));
#24586=CARTESIAN_POINT('Ctrl Pts',(-3.88130046816268,-0.635606541690823,
11.6282429148196));
#24587=CARTESIAN_POINT('Ctrl Pts',(-3.86182449886414,-0.754535602041985,
11.6343323983989));
#24588=CARTESIAN_POINT('Ctrl Pts',(-3.83686150121785,-0.872664895569536,
11.6404218819781));
#24589=CARTESIAN_POINT('Ctrl Pts',(-3.80650371712151,-0.989453612626731,
11.6465113655574));
#24590=CARTESIAN_POINT('Ctrl Pts',(-3.77733142788604,-1.10168164029242,
11.6523630501108));
#24591=CARTESIAN_POINT('Ctrl Pts',(-3.74317790042519,-1.21267138998945,
11.6582147346641));
#24592=CARTESIAN_POINT('Ctrl Pts',(-3.70417701890166,-1.32195371047582,
11.6640664192174));
#24593=CARTESIAN_POINT('Ctrl Pts',(-3.66518208585912,-1.43121936303624,
11.6699172112618));
#24594=CARTESIAN_POINT('Ctrl Pts',(-3.62134140768428,-1.53877771492978,
11.6757680033062));
#24595=CARTESIAN_POINT('Ctrl Pts',(-3.57283821333391,-1.64417642038224,
11.6816187953506));
#24596=CARTESIAN_POINT('Ctrl Pts',(-3.52433066880314,-1.7495845788901,11.687470112144));
#24597=CARTESIAN_POINT('Ctrl Pts',(-3.47115994964086,-1.85283233033098,
11.6933214289374));
#24598=CARTESIAN_POINT('Ctrl Pts',(-3.41355644074184,-1.95348955100096,
11.6991727457308));
#24599=CARTESIAN_POINT('Ctrl Pts',(-3.35593381331242,-2.0541801796728,11.7050260045686));
#24600=CARTESIAN_POINT('Ctrl Pts',(-3.29387567591725,-2.1522782093075,11.7108792634065));
#24601=CARTESIAN_POINT('Ctrl Pts',(-3.22765677227372,-2.24738086678595,
11.7167325222444));
#24602=CARTESIAN_POINT('Ctrl Pts',(-3.16136253171153,-2.34259172208673,
11.7225924403059));
#24603=CARTESIAN_POINT('Ctrl Pts',(-3.09089831296656,-2.4348000638389,11.7284523583673));
#24604=CARTESIAN_POINT('Ctrl Pts',(-3.01658039560449,-2.52363462427797,
11.7343122764288));
#24605=CARTESIAN_POINT('Ctrl Pts',(-2.94221243786159,-2.61252899956915,
11.7401761401408));
#24606=CARTESIAN_POINT('Ctrl Pts',(-2.86398589309222,-2.69804476592693,
11.7460400038529));
#24607=CARTESIAN_POINT('Ctrl Pts',(-2.78225406666779,-2.77984735345496,
11.7519038675649));
#24608=CARTESIAN_POINT('Ctrl Pts',(-2.70040166615228,-2.86177061946371,
11.7577763818855));
#24609=CARTESIAN_POINT('Ctrl Pts',(-2.61503396706536,-2.93996949570728,
11.763648896206));
#24610=CARTESIAN_POINT('Ctrl Pts',(-2.52653754786125,-3.01414946863079,
11.7695214105266));
#24611=CARTESIAN_POINT('Ctrl Pts',(-2.50207903977182,-3.03465121869187,
11.7711444472586));
#24612=CARTESIAN_POINT('Ctrl Pts',(-2.4773817136686,-3.05484624018212,11.7727674839905));
#24613=CARTESIAN_POINT('Ctrl Pts',(-2.45245410270203,-3.07472891067489,
11.7743905207225));
#24614=CARTESIAN_POINT('Ctrl Pts',(-2.36226635846595,-3.14666413156455,
11.7802626446843));
#24615=CARTESIAN_POINT('Ctrl Pts',(-2.26875973340759,-3.21474851506088,
11.7861347686461));
#24616=CARTESIAN_POINT('Ctrl Pts',(-2.17229721285864,-3.2786603695727,11.7920068926079));
#24617=CARTESIAN_POINT('Ctrl Pts',(-2.07595975788287,-3.34248936109616,
11.7978714032445));
#24618=CARTESIAN_POINT('Ctrl Pts',(-1.97667437007134,-3.40215635547035,
11.803735913881));
#24619=CARTESIAN_POINT('Ctrl Pts',(-1.87483718466834,-3.45737972039302,
11.8096004245175));
#24620=CARTESIAN_POINT('Ctrl Pts',(-1.77310478871571,-3.51254626102273,
11.8154589006309));
#24621=CARTESIAN_POINT('Ctrl Pts',(-1.6688261791917,-3.56327807113751,11.8213173767443));
#24622=CARTESIAN_POINT('Ctrl Pts',(-1.56242599901136,-3.60933705791152,
11.8271758528578));
#24623=CARTESIAN_POINT('Ctrl Pts',(-1.45183031867757,-3.65721221159191,
11.8332653364506));
#24624=CARTESIAN_POINT('Ctrl Pts',(-1.33894269222286,-3.70003819797956,
11.8393548200434));
#24625=CARTESIAN_POINT('Ctrl Pts',(-1.22426802220387,-3.73760040799027,
11.8454443036363));
#24626=CARTESIAN_POINT('Ctrl Pts',(-1.11407148735314,-3.77369578444812,
11.8512959881526));
#24627=CARTESIAN_POINT('Ctrl Pts',(-1.00222529057778,-3.80493063814588,
11.8571476726689));
#24628=CARTESIAN_POINT('Ctrl Pts',(-0.889196539348197,-3.83116412000467,
11.8629993571852));
#24629=CARTESIAN_POINT('Ctrl Pts',(-0.776185027459509,-3.85739360068738,
11.8688501491924));
#24630=CARTESIAN_POINT('Ctrl Pts',(-0.661991722336443,-3.87862313281099,
11.8747009411997));
#24631=CARTESIAN_POINT('Ctrl Pts',(-0.547096253974035,-3.89476246886605,
11.8805517332069));
#24632=CARTESIAN_POINT('Ctrl Pts',(-0.432190480807463,-3.91090325243423,
11.886403049963));
#24633=CARTESIAN_POINT('Ctrl Pts',(-0.316582828628814,-3.92195287487916,
11.8922543667191));
#24634=CARTESIAN_POINT('Ctrl Pts',(-0.200759709458467,-3.92787277531467,
11.8981056834752));
#24635=CARTESIAN_POINT('Ctrl Pts',(-0.0848981487451517,-3.93379464055745,
11.9039589422757));
#24636=CARTESIAN_POINT('Ctrl Pts',(0.0311786085037482,-3.93458337729355,
11.9098122010763));
#24637=CARTESIAN_POINT('Ctrl Pts',(0.146983195004135,-3.9302525288315,11.9156654598768));
#24638=CARTESIAN_POINT('Ctrl Pts',(0.262919531811611,-3.9259167531845,11.921525377901));
#24639=CARTESIAN_POINT('Ctrl Pts',(0.378582666452337,-3.91644978219727,
11.9273852959252));
#24640=CARTESIAN_POINT('Ctrl Pts',(0.493489297763407,-3.90191713302486,
11.9332452139495));
#24641=CARTESIAN_POINT('Ctrl Pts',(0.608473298998659,-3.88737469860376,
11.9391090776242));
#24642=CARTESIAN_POINT('Ctrl Pts',(0.722699376183601,-3.86775986409176,
11.944972941299));
#24643=CARTESIAN_POINT('Ctrl Pts',(0.835695100465841,-3.84318913131495,
11.9508368049738));
#24644=CARTESIAN_POINT('Ctrl Pts',(0.948857520610756,-3.81858215079937,
11.9567093192574));
#24645=CARTESIAN_POINT('Ctrl Pts',(1.0607855671211,-3.78900478556273,11.962581833541));
#24646=CARTESIAN_POINT('Ctrl Pts',(1.17102253719025,-3.75462317914761,11.9684543478246));
#24647=CARTESIAN_POINT('Ctrl Pts',(1.20148967309694,-3.74512084000782,11.9700773849117));
#24648=CARTESIAN_POINT('Ctrl Pts',(1.23182775947559,-3.73525180915616,11.9717004219989));
#24649=CARTESIAN_POINT('Ctrl Pts',(1.26202745450664,-3.7250202286795,11.973323459086));
#24650=CARTESIAN_POINT('Ctrl Pts',(1.3712895004446,-3.68800252320569,11.9791955830458));
#24651=CARTESIAN_POINT('Ctrl Pts',(1.47910464051812,-3.6461113813765,11.9850677070056));
#24652=CARTESIAN_POINT('Ctrl Pts',(1.58500605166983,-3.59947840890455,11.9909398309654));
#24653=CARTESIAN_POINT('Ctrl Pts',(1.69077015953713,-3.55290589700826,11.9968043415998));
#24654=CARTESIAN_POINT('Ctrl Pts',(1.79462509780673,-3.50160394543342,12.0026688522342));
#24655=CARTESIAN_POINT('Ctrl Pts',(1.89611983850175,-3.44575369956126,12.0085333628686));
#24656=CARTESIAN_POINT('Ctrl Pts',(1.99751014211621,-3.38996092303763,12.0143918389798));
#24657=CARTESIAN_POINT('Ctrl Pts',(2.09654471878094,-3.3296293593651,12.020250315091));
#24658=CARTESIAN_POINT('Ctrl Pts',(2.19279377239964,-3.26498766792853,12.0261087912022));
#24659=CARTESIAN_POINT('Ctrl Pts',(2.29283805384609,-3.1977970688721,12.0321982747958));
#24660=CARTESIAN_POINT('Ctrl Pts',(2.38987220270247,-3.12594962440529,12.0382877583894));
#24661=CARTESIAN_POINT('Ctrl Pts',(2.48344281495836,-3.04975421711844,12.0443772419831));
#24662=CARTESIAN_POINT('Ctrl Pts',(2.57335942188605,-2.97653429986524,12.0502289264968));
#24663=CARTESIAN_POINT('Ctrl Pts',(2.66007757281388,-2.89929991563099,12.0560806110106));
#24664=CARTESIAN_POINT('Ctrl Pts',(2.74322635097398,-2.81836800069153,12.0619322955244));
#24665=CARTESIAN_POINT('Ctrl Pts',(2.82636244713697,-2.73744842962932,12.067783087529));
#24666=CARTESIAN_POINT('Ctrl Pts',(2.90592995681614,-2.65283273745029,12.0736338795336));
#24667=CARTESIAN_POINT('Ctrl Pts',(2.98159377500211,-2.56487573984952,12.0794846715382));
#24668=CARTESIAN_POINT('Ctrl Pts',(3.05726437936244,-2.47691085351759,12.0853359882916));
#24669=CARTESIAN_POINT('Ctrl Pts',(3.12903032661077,-2.38560437945964,12.0911873050449));
#24670=CARTESIAN_POINT('Ctrl Pts',(3.19659633837172,-2.2913447688003,12.0970386217983));
#24671=CARTESIAN_POINT('Ctrl Pts',(3.26418477520299,-2.19705387350032,12.102891880596));
#24672=CARTESIAN_POINT('Ctrl Pts',(3.32757026403745,-2.09980822847908,12.1087451393937));
#24673=CARTESIAN_POINT('Ctrl Pts',(3.38650085297318,-2.00002524304368,12.1145983981914));
#24674=CARTESIAN_POINT('Ctrl Pts',(3.44549848694824,-1.90012873499966,12.1204583162126));
#24675=CARTESIAN_POINT('Ctrl Pts',(3.50003089444123,-1.79768948090604,12.1263182342339));
#24676=CARTESIAN_POINT('Ctrl Pts',(3.54989205363726,-1.69314955261578,12.1321781522551));
#24677=CARTESIAN_POINT('Ctrl Pts',(3.59978678577848,-1.58853923460057,12.1380420159268));
#24678=CARTESIAN_POINT('Ctrl Pts',(3.64500384584713,-1.48182580567601,12.1439058795986));
#24679=CARTESIAN_POINT('Ctrl Pts',(3.68538598749074,-1.37346973872995,12.1497697432703));
#24680=CARTESIAN_POINT('Ctrl Pts',(3.72582770250234,-1.2649538205331,12.1556422575508));
#24681=CARTESIAN_POINT('Ctrl Pts',(3.76142013698568,-1.1547908198029,12.1615147718313));
#24682=CARTESIAN_POINT('Ctrl Pts',(3.79205631273742,-1.04345480066378,12.1673872861118));
#24683=CARTESIAN_POINT('Ctrl Pts',(3.80052349525184,-1.01268391065065,12.1690103232243));
#24684=CARTESIAN_POINT('Ctrl Pts',(3.808612396395,-0.981823467267782,12.1706333603369));
#24685=CARTESIAN_POINT('Ctrl Pts',(3.81632145366088,-0.950883569280524,
12.1722563974494));
#24686=CARTESIAN_POINT('Ctrl Pts',(3.8547788322017,-0.796536892654378,12.1803530752234));
#24687=CARTESIAN_POINT('Ctrl Pts',(3.88388803832101,-0.639774846675686,
12.1884497529973));
#24688=CARTESIAN_POINT('Ctrl Pts',(3.90340589677512,-0.481571806713381,
12.1965464307713));
#24689=CARTESIAN_POINT('Ctrl Pts',(3.92170070402504,-0.333282273347502,
12.2041357449159));
#24690=CARTESIAN_POINT('Ctrl Pts',(3.93156890341389,-0.183726492797682,
12.2117250590606));
#24691=CARTESIAN_POINT('Ctrl Pts',(3.93285535666324,-0.03373045456698,12.2193143732052));
#24692=CARTESIAN_POINT('Ctrl Pts',(3.9329413591105,-0.0237028640777174,
12.2198217368345));
#24693=CARTESIAN_POINT('Ctrl Pts',(3.93298902446914,-0.0136733158283392,
12.2203291004638));
#24694=CARTESIAN_POINT('Ctrl Pts',(3.93299831367774,-0.00364206096290877,
12.2208364640931));
#24695=CARTESIAN_POINT('',(3.92657020349652,0.00060237016638537,13.470836477965));
#24696=CARTESIAN_POINT('Ctrl Pts',(3.93255568468074,-0.00364137684070624,
12.220836477965));
#24697=CARTESIAN_POINT('Ctrl Pts',(3.92346996534201,0.987148471629003,12.2709540972476));
#24698=CARTESIAN_POINT('Ctrl Pts',(3.04053014230206,3.3032803818384,12.3873826959847));
#24699=CARTESIAN_POINT('Ctrl Pts',(-0.855351412277205,4.57304180444516,
12.5701222741763));
#24700=CARTESIAN_POINT('Ctrl Pts',(-4.31013578855369,1.75130433299333,12.7690552125397));
#24701=CARTESIAN_POINT('Ctrl Pts',(-3.80259280182653,-2.68041514802392,
12.9679881509031));
#24702=CARTESIAN_POINT('Ctrl Pts',(0.20069098000617,-4.64801683659501,13.1669210892666));
#24703=CARTESIAN_POINT('Ctrl Pts',(3.4183096060697,-2.70559174609466,13.3345371982872));
#24704=CARTESIAN_POINT('Ctrl Pts',(3.925624757664,-0.693867882632318,13.4358423278534));
#24705=CARTESIAN_POINT('Ctrl Pts',(3.92657020349652,0.00060237016638537,
13.470836477965));
#24706=CARTESIAN_POINT('',(3.93319014431769,0.0034425050413224,14.7208363833869));
#24707=CARTESIAN_POINT('Ctrl Pts',(3.92657020349652,0.00060237016638537,
13.470836477965));
#24708=CARTESIAN_POINT('Ctrl Pts',(3.92741629822079,0.622095000252939,13.5021533073078));
#24709=CARTESIAN_POINT('Ctrl Pts',(3.49488999972759,2.55843734936597,13.5997811161051));
#24710=CARTESIAN_POINT('Ctrl Pts',(0.457995462913449,4.62974918743228,13.7637199043569));
#24711=CARTESIAN_POINT('Ctrl Pts',(-3.64818774369287,2.88705101605783,13.9626528427203));
#24712=CARTESIAN_POINT('Ctrl Pts',(-4.40057542481316,-1.5097262377929,14.1615857810838));
#24713=CARTESIAN_POINT('Ctrl Pts',(-1.10749417555734,-4.5186053195277,14.3605187194471));
#24714=CARTESIAN_POINT('Ctrl Pts',(2.93246189479444,-3.44555640217872,14.546935326452));
#24715=CARTESIAN_POINT('Ctrl Pts',(3.92501016529069,-1.05851774818717,14.6670409540021));
#24716=CARTESIAN_POINT('Ctrl Pts',(3.93477334405261,0.00342846837678905,
14.7208356020977));
#24717=CARTESIAN_POINT('',(3.93483603884783,-0.00214359731175201,15.9708371227931));
#24718=CARTESIAN_POINT('Ctrl Pts',(3.93299849192155,0.00344420423336513,
14.720836477965));
#24719=CARTESIAN_POINT('Ctrl Pts',(3.93284829647542,0.174955073829664,14.729528644049));
#24720=CARTESIAN_POINT('Ctrl Pts',(3.92147599299458,0.345993796770016,14.7382208101329));
#24721=CARTESIAN_POINT('Ctrl Pts',(3.89908469475258,0.515390670410515,14.7469129762169));
#24722=CARTESIAN_POINT('Ctrl Pts',(3.88923427460412,0.589912047382934,14.750736849536));
#24723=CARTESIAN_POINT('Ctrl Pts',(3.8772518881715,0.66411615003633,14.754560722855));
#24724=CARTESIAN_POINT('Ctrl Pts',(3.86315739411471,0.737905107921655,14.7583845961741));
#24725=CARTESIAN_POINT('Ctrl Pts',(3.84151321047313,0.851218984159783,14.7642567201401));
#24726=CARTESIAN_POINT('Ctrl Pts',(3.81484294080112,0.963769723562685,14.7701288441062));
#24727=CARTESIAN_POINT('Ctrl Pts',(3.78321275945683,1.07507684222245,14.7760009680722));
#24728=CARTESIAN_POINT('Ctrl Pts',(3.75162358727073,1.1862396489927,14.7818654787129));
#24729=CARTESIAN_POINT('Ctrl Pts',(3.7150874035512,1.29616164746434,14.7877299893536));
#24730=CARTESIAN_POINT('Ctrl Pts',(3.67372162348358,1.40437118780939,14.7935944999943));
#24731=CARTESIAN_POINT('Ctrl Pts',(3.6323984083921,1.51246938161401,14.799452976112));
#24732=CARTESIAN_POINT('Ctrl Pts',(3.58625562846616,1.61885823836361,14.8053114522296));
#24733=CARTESIAN_POINT('Ctrl Pts',(3.53546068077294,1.72308060598121,14.8111699283472));
#24734=CARTESIAN_POINT('Ctrl Pts',(3.48266282100748,1.8314125996104,14.8172594119384));
#24735=CARTESIAN_POINT('Ctrl Pts',(3.42483848772265,1.93740329631429,14.8233488955297));
#24736=CARTESIAN_POINT('Ctrl Pts',(3.36223129361279,2.04056113073116,14.829438379121));
#24737=CARTESIAN_POINT('Ctrl Pts',(3.30206895913103,2.13969057147421,14.8352900636414));
#24738=CARTESIAN_POINT('Ctrl Pts',(3.23749053752719,2.23620386226628,14.8411417481618));
#24739=CARTESIAN_POINT('Ctrl Pts',(3.16875895953531,2.32969003439614,14.8469934326822));
#24740=CARTESIAN_POINT('Ctrl Pts',(3.10003786460307,2.42316194785268,14.8528442246935));
#24741=CARTESIAN_POINT('Ctrl Pts',(3.02716511758818,2.51360732766554,14.8586950167048));
#24742=CARTESIAN_POINT('Ctrl Pts',(2.95044609254254,2.60064546891738,14.8645458087161));
#24743=CARTESIAN_POINT('Ctrl Pts',(2.87372018668186,2.6876914164904,14.8703971254763));
#24744=CARTESIAN_POINT('Ctrl Pts',(2.79314759040793,2.77132920786618,14.8762484422364));
#24745=CARTESIAN_POINT('Ctrl Pts',(2.70907246939167,2.85121296215911,14.8820997589966));
#24746=CARTESIAN_POINT('Ctrl Pts',(2.62496944395245,2.93112322976585,14.8879530178011));
#24747=CARTESIAN_POINT('Ctrl Pts',(2.53736188179197,3.00727669816909,14.8938062766056));
#24748=CARTESIAN_POINT('Ctrl Pts',(2.44662858854818,3.07936642017457,14.8996595354102));
#24749=CARTESIAN_POINT('Ctrl Pts',(2.35579206848544,3.15153815830021,14.9055194534383));
#24750=CARTESIAN_POINT('Ctrl Pts',(2.26182304327764,3.21963666470747,14.9113793714664));
#24751=CARTESIAN_POINT('Ctrl Pts',(2.16513106164585,3.28339709537185,14.9172392894945));
#24752=CARTESIAN_POINT('Ctrl Pts',(2.06837397453576,3.34720045775885,14.9231031531732));
#24753=CARTESIAN_POINT('Ctrl Pts',(1.96889063425004,3.40665971664292,14.9289670168518));
#24754=CARTESIAN_POINT('Ctrl Pts',(1.86711552174194,3.46155581039369,14.9348308805304));
#24755=CARTESIAN_POINT('Ctrl Pts',(1.76519026647323,3.51653288908135,14.9407033948178));
#24756=CARTESIAN_POINT('Ctrl Pts',(1.66096686208982,3.56693318797672,14.9465759091052));
#24757=CARTESIAN_POINT('Ctrl Pts',(1.5549001628775,3.61258556763484,14.9524484233926));
#24758=CARTESIAN_POINT('Ctrl Pts',(1.52558560117776,3.62520290663159,14.9540714604409));
#24759=CARTESIAN_POINT('Ctrl Pts',(1.49613032818587,3.63745786887671,14.9556944974892));
#24760=CARTESIAN_POINT('Ctrl Pts',(1.46654413194279,3.64934751826462,14.9573175345375));
#24761=CARTESIAN_POINT('Ctrl Pts',(1.35950171279001,3.69236409338985,14.9631896585035));
#24762=CARTESIAN_POINT('Ctrl Pts',(1.25038559468209,3.73073915030892,14.9690617824696));
#24763=CARTESIAN_POINT('Ctrl Pts',(1.13963583403457,3.7642687425029,14.9749339064356));
#24764=CARTESIAN_POINT('Ctrl Pts',(1.02902966265078,3.79775486291483,14.9807984170763));
#24765=CARTESIAN_POINT('Ctrl Pts',(0.916794452779745,3.82640789301592,14.986662927717));
#24766=CARTESIAN_POINT('Ctrl Pts',(0.803390515337624,3.85007177593685,14.9925274383577));
#24767=CARTESIAN_POINT('Ctrl Pts',(0.690103269418896,3.87371130895768,14.9983859144753));
#24768=CARTESIAN_POINT('Ctrl Pts',(0.575650090234624,3.89237182219734,15.004244390593));
#24769=CARTESIAN_POINT('Ctrl Pts',(0.460506097283638,3.90594714945871,15.0101028667106));
#24770=CARTESIAN_POINT('Ctrl Pts',(0.340821824166863,3.92005776985634,15.0161923503018));
#24771=CARTESIAN_POINT('Ctrl Pts',(0.220391572605051,3.92867379076967,15.0222818338931));
#24772=CARTESIAN_POINT('Ctrl Pts',(0.0997606018152224,3.93173458187674,
15.0283713174844));
#24773=CARTESIAN_POINT('Ctrl Pts',(-0.0161596357340333,3.93467584671028,
15.0342230020048));
#24774=CARTESIAN_POINT('Ctrl Pts',(-0.132264757993117,3.93248760048722,
15.0400746865252));
#24775=CARTESIAN_POINT('Ctrl Pts',(-0.248066884677823,3.92516901810944,
15.0459263710456));
#24776=CARTESIAN_POINT('Ctrl Pts',(-0.363851349021001,3.91785155197456,
15.0517771630569));
#24777=CARTESIAN_POINT('Ctrl Pts',(-0.479332497200843,3.90540533158387,
15.0576279550682));
#24778=CARTESIAN_POINT('Ctrl Pts',(-0.594024980004118,3.88788159839405,
15.0634787470795));
#24779=CARTESIAN_POINT('Ctrl Pts',(-0.70872774940532,3.87035629352672,15.0693300638397));
#24780=CARTESIAN_POINT('Ctrl Pts',(-0.822641304122427,3.84775263302172,
15.0751813805998));
#24781=CARTESIAN_POINT('Ctrl Pts',(-0.935288636375196,3.82017331631268,
15.0810326973599));
#24782=CARTESIAN_POINT('Ctrl Pts',(-1.04797335613054,3.79258484606442,15.0868859561645));
#24783=CARTESIAN_POINT('Ctrl Pts',(-1.159390616426,3.76001753414329,15.092739214969));
#24784=CARTESIAN_POINT('Ctrl Pts',(-1.26907745228952,3.7226242652315,15.0985924737735));
#24785=CARTESIAN_POINT('Ctrl Pts',(-1.37888907832363,3.68518845418263,15.1044523918016));
#24786=CARTESIAN_POINT('Ctrl Pts',(-1.48696595892933,3.6429158607928,15.1103123098298));
#24787=CARTESIAN_POINT('Ctrl Pts',(-1.59286394454679,3.59600798861221,15.1161722278579));
#24788=CARTESIAN_POINT('Ctrl Pts',(-1.69883323430863,3.54906853201884,15.1220360915365));
#24789=CARTESIAN_POINT('Ctrl Pts',(-1.80262033846515,3.49748776552355,15.1278999552151));
#24790=CARTESIAN_POINT('Ctrl Pts',(-1.90380615860214,3.44151291011214,15.1337638188938));
#24791=CARTESIAN_POINT('Ctrl Pts',(-2.00514125215168,3.38545547833112,15.1396363331812));
#24792=CARTESIAN_POINT('Ctrl Pts',(-2.10386705147764,3.32499123520002,15.1455088474686));
#24793=CARTESIAN_POINT('Ctrl Pts',(-2.19959377321235,3.26041043932286,15.1513813617559));
#24794=CARTESIAN_POINT('Ctrl Pts',(-2.22605058681703,3.24256169188848,15.1530043988043));
#24795=CARTESIAN_POINT('Ctrl Pts',(-2.25227851449835,3.22439873463254,15.1546274358526));
#24796=CARTESIAN_POINT('Ctrl Pts',(-2.27826979674855,3.20592821710395,15.156250472901));
#24797=CARTESIAN_POINT('Ctrl Pts',(-2.37230587039499,3.13910215866305,15.162122596867));
#24798=CARTESIAN_POINT('Ctrl Pts',(-2.46355689507432,3.06802316936622,15.1679947208331));
#24799=CARTESIAN_POINT('Ctrl Pts',(-2.55161347817067,2.99295132904259,15.1738668447991));
#24800=CARTESIAN_POINT('Ctrl Pts',(-2.63955589415856,2.91797682085057,15.1797313554398));
#24801=CARTESIAN_POINT('Ctrl Pts',(-2.72431179312379,2.83902002216063,15.1855958660805));
#24802=CARTESIAN_POINT('Ctrl Pts',(-2.80550113433061,2.75638393284928,15.1914603767212));
#24803=CARTESIAN_POINT('Ctrl Pts',(-2.88660693251308,2.67383287525169,15.1973188528388));
#24804=CARTESIAN_POINT('Ctrl Pts',(-2.96415318465746,2.58761035059531,15.2031773289564));
#24805=CARTESIAN_POINT('Ctrl Pts',(-3.03779382834163,2.49805877762904,15.209035805074));
#24806=CARTESIAN_POINT('Ctrl Pts',(-3.11433822015321,2.4049760675176,15.2151252886653));
#24807=CARTESIAN_POINT('Ctrl Pts',(-3.18666231397037,2.30829666556898,15.2212147722566));
#24808=CARTESIAN_POINT('Ctrl Pts',(-3.25442046332261,2.20844661423071,15.2273042558478));
#24809=CARTESIAN_POINT('Ctrl Pts',(-3.31953260423783,2.11249578506427,15.2331559403682));
#24810=CARTESIAN_POINT('Ctrl Pts',(-3.38042846209905,2.01361766649564,15.2390076248886));
#24811=CARTESIAN_POINT('Ctrl Pts',(-3.4368437176281,1.91222233555626,15.244859309409));
#24812=CARTESIAN_POINT('Ctrl Pts',(-3.49325036860438,1.81084246960889,15.2507101014203));
#24813=CARTESIAN_POINT('Ctrl Pts',(-3.54517757509486,1.70694651582322,15.2565608934316));
#24814=CARTESIAN_POINT('Ctrl Pts',(-3.59240619645619,1.60097055552661,15.262411685443));
#24815=CARTESIAN_POINT('Ctrl Pts',(-3.63963905368221,1.49498509040399,15.2682630022031));
#24816=CARTESIAN_POINT('Ctrl Pts',(-3.68217231976241,1.38691962555487,15.2741143189632));
#24817=CARTESIAN_POINT('Ctrl Pts',(-3.7198346602213,1.27723102867737,15.2799656357233));
#24818=CARTESIAN_POINT('Ctrl Pts',(-3.75750950076182,1.16750602629776,15.2858188945279));
#24819=CARTESIAN_POINT('Ctrl Pts',(-3.79031006688662,1.05615721148869,15.2916721533324));
#24820=CARTESIAN_POINT('Ctrl Pts',(-3.81811484008639,0.943656753227619,
15.2975254121369));
#24821=CARTESIAN_POINT('Ctrl Pts',(-3.8459512466391,0.831028303751601,15.303385330165));
#24822=CARTESIAN_POINT('Ctrl Pts',(-3.86878041652374,0.71724599723719,15.3092452481931));
#24823=CARTESIAN_POINT('Ctrl Pts',(-3.88653190804482,0.60279244168245,15.3151051662213));
#24824=CARTESIAN_POINT('Ctrl Pts',(-3.90429535215317,0.488261821273257,
15.3209690298999));
#24825=CARTESIAN_POINT('Ctrl Pts',(-3.91697426499136,0.373059461789268,
15.3268328935785));
#24826=CARTESIAN_POINT('Ctrl Pts',(-3.92455020975565,0.257671595459889,
15.3326967572571));
#24827=CARTESIAN_POINT('Ctrl Pts',(-3.93213733085994,0.142113504285216,
15.3385692715445));
#24828=CARTESIAN_POINT('Ctrl Pts',(-3.93460645040682,0.0263697718473956,
15.3444417858319));
#24829=CARTESIAN_POINT('Ctrl Pts',(-3.931991185563,-0.0890747812506412,
15.3503143001193));
#24830=CARTESIAN_POINT('Ctrl Pts',(-3.93126838242877,-0.120981180714116,
15.3519373371676));
#24831=CARTESIAN_POINT('Ctrl Pts',(-3.93015751202227,-0.152864768556174,
15.353560374216));
#24832=CARTESIAN_POINT('Ctrl Pts',(-3.92865997671956,-0.184715422533844,
15.3551834112644));
#24833=CARTESIAN_POINT('Ctrl Pts',(-3.92324191620768,-0.299950616176578,
15.3610555352304));
#24834=CARTESIAN_POINT('Ctrl Pts',(-3.91274036694306,-0.415140414715906,
15.3669276591964));
#24835=CARTESIAN_POINT('Ctrl Pts',(-3.89715295659655,-0.529799804540171,
15.3727997831624));
#24836=CARTESIAN_POINT('Ctrl Pts',(-3.88158575563705,-0.644310536188886,
15.3786642938032));
#24837=CARTESIAN_POINT('Ctrl Pts',(-3.86094586168443,-0.758291820821086,
15.3845288044439));
#24838=CARTESIAN_POINT('Ctrl Pts',(-3.83528287735399,-0.871260150974015,
15.3903933150846));
#24839=CARTESIAN_POINT('Ctrl Pts',(-3.80964629997913,-0.984112237839073,
15.3962517912022));
#24840=CARTESIAN_POINT('Ctrl Pts',(-3.77899700406635,-1.09595304273518,
15.4021102673198));
#24841=CARTESIAN_POINT('Ctrl Pts',(-3.7434361210232,-1.20630634907506,15.4079687434374));
#24842=CARTESIAN_POINT('Ctrl Pts',(-3.70647302525648,-1.32101103246172,
15.4140582270287));
#24843=CARTESIAN_POINT('Ctrl Pts',(-3.66420309412753,-1.4341080449332,15.4201477106199));
#24844=CARTESIAN_POINT('Ctrl Pts',(-3.61679804827907,-1.54507633402518,
15.4262371942112));
#24845=CARTESIAN_POINT('Ctrl Pts',(-3.57124420634438,-1.65171122511293,
15.4320888787316));
#24846=CARTESIAN_POINT('Ctrl Pts',(-3.52094896171056,-1.75638011353525,
15.437940563252));
#24847=CARTESIAN_POINT('Ctrl Pts',(-3.46611454601575,-1.85863900580453,
15.4437922477724));
#24848=CARTESIAN_POINT('Ctrl Pts',(-3.4112884937613,-1.96088230136988,15.4496430397837));
#24849=CARTESIAN_POINT('Ctrl Pts',(-3.35192484231415,-2.06071596740399,
15.455493831795));
#24850=CARTESIAN_POINT('Ctrl Pts',(-3.28827211658734,-2.15771997424925,
15.4613446238064));
#24851=CARTESIAN_POINT('Ctrl Pts',(-3.22461368194239,-2.25473268123938,
15.4671959405665));
#24852=CARTESIAN_POINT('Ctrl Pts',(-3.15666563512766,-2.34891487887022,
15.4730472573266));
#24853=CARTESIAN_POINT('Ctrl Pts',(-3.08471982353216,-2.43987553172446,
15.4788985740868));
#24854=CARTESIAN_POINT('Ctrl Pts',(-3.01275013321574,-2.53086637430061,
15.4847518328913));
#24855=CARTESIAN_POINT('Ctrl Pts',(-2.93678029608717,-2.6186332219377,15.4906050916958));
#24856=CARTESIAN_POINT('Ctrl Pts',(-2.85714195261617,-2.70281868844372,
15.4964583505003));
#24857=CARTESIAN_POINT('Ctrl Pts',(-2.77741300499568,-2.78709993233863,
15.5023182685285));
#24858=CARTESIAN_POINT('Ctrl Pts',(-2.69400750482798,-2.86779136196497,
15.5081781865566));
#24859=CARTESIAN_POINT('Ctrl Pts',(-2.60729347565185,-2.94457292859649,
15.5140381045847));
#24860=CARTESIAN_POINT('Ctrl Pts',(-2.52052105943819,-3.02140619445425,
15.5199019682633));
#24861=CARTESIAN_POINT('Ctrl Pts',(-2.43043599892805,-3.09432409578404,
15.525765831942));
#24862=CARTESIAN_POINT('Ctrl Pts',(-2.3374374679654,-3.16304838460487,15.5316296956206));
#24863=CARTESIAN_POINT('Ctrl Pts',(-2.24430174181019,-3.23187405827491,
15.537502209908));
#24864=CARTESIAN_POINT('Ctrl Pts',(-2.14824430878899,-3.29649354226668,
15.5433747241954));
#24865=CARTESIAN_POINT('Ctrl Pts',(-2.04969128218924,-3.35667315175568,
15.5492472384828));
#24866=CARTESIAN_POINT('Ctrl Pts',(-2.02245333851314,-3.37330550562918,
15.5508702755311));
#24867=CARTESIAN_POINT('Ctrl Pts',(-1.99502489821788,-3.38959899726523,
15.5524933125795));
#24868=CARTESIAN_POINT('Ctrl Pts',(-1.9674152363527,-3.40554933715065,15.5541163496278));
#24869=CARTESIAN_POINT('Ctrl Pts',(-1.86752388926439,-3.46325743026134,
15.5599884735938));
#24870=CARTESIAN_POINT('Ctrl Pts',(-1.76492388788527,-3.51666353423357,
15.5658605975599));
#24871=CARTESIAN_POINT('Ctrl Pts',(-1.66002206106583,-3.5655035768843,15.5717327215259));
#24872=CARTESIAN_POINT('Ctrl Pts',(-1.55525624154774,-3.61428029745,15.5775972321666));
#24873=CARTESIAN_POINT('Ctrl Pts',(-1.44819490272289,-3.65850255652633,
15.5834617428073));
#24874=CARTESIAN_POINT('Ctrl Pts',(-1.33927169064858,-3.69795082966598,
15.589326253448));
#24875=CARTESIAN_POINT('Ctrl Pts',(-1.23046055947581,-3.73735851092504,
15.5951847295657));
#24876=CARTESIAN_POINT('Ctrl Pts',(-1.11979175213365,-3.77200183728434,
15.6010432056833));
#24877=CARTESIAN_POINT('Ctrl Pts',(-1.00772062329801,-3.80170858238501,
15.6069016818009));
#24878=CARTESIAN_POINT('Ctrl Pts',(-0.891230381399196,-3.83258670379556,
15.6129911653922));
#24879=CARTESIAN_POINT('Ctrl Pts',(-0.773225364568132,-3.85813073069646,
15.6190806489834));
#24880=CARTESIAN_POINT('Ctrl Pts',(-0.654236796995729,-3.87820360649834,
15.6251701325747));
#24881=CARTESIAN_POINT('Ctrl Pts',(-0.539894825540682,-3.89749262088675,
15.6310218170951));
#24882=CARTESIAN_POINT('Ctrl Pts',(-0.424645124729601,-3.9117296957019,
15.6368735016155));
#24883=CARTESIAN_POINT('Ctrl Pts',(-0.308970564655511,-3.92084508622522,
15.6427251861359));
#24884=CARTESIAN_POINT('Ctrl Pts',(-0.193313647466286,-3.92995908645334,
15.6485759781472));
#24885=CARTESIAN_POINT('Ctrl Pts',(-0.0772324118786128,-3.93395292312858,
15.6544267701585));
#24886=CARTESIAN_POINT('Ctrl Pts',(0.0387854217168801,-3.93280875343084,
15.6602775621698));
#24887=CARTESIAN_POINT('Ctrl Pts',(0.154813660779084,-3.93166448111423,
15.66612887893));
#24888=CARTESIAN_POINT('Ctrl Pts',(0.270778073127861,-3.9253812904337,15.6719801956901));
#24889=CARTESIAN_POINT('Ctrl Pts',(0.386191926136979,-3.91399345888398,
15.6778315124503));
#24890=CARTESIAN_POINT('Ctrl Pts',(0.501644084853312,-3.90260184772783,
15.6836847712548));
#24891=CARTESIAN_POINT('Ctrl Pts',(0.616544909686108,-3.88610226742192,
15.6895380300593));
#24892=CARTESIAN_POINT('Ctrl Pts',(0.730414479773336,-3.86458066130563,
15.6953912888639));
#24893=CARTESIAN_POINT('Ctrl Pts',(0.844413598707175,-3.84303457016451,
15.701251206892));
#24894=CARTESIAN_POINT('Ctrl Pts',(0.957378714649444,-3.81645512597312,
15.7071111249201));
#24895=CARTESIAN_POINT('Ctrl Pts',(1.06884166453412,-3.78497906152147,15.7129710429482));
#24896=CARTESIAN_POINT('Ctrl Pts',(1.18037966561287,-3.75348180333481,15.7188349066269));
#24897=CARTESIAN_POINT('Ctrl Pts',(1.29041309510056,-3.71708148937148,15.7246987703055));
#24898=CARTESIAN_POINT('Ctrl Pts',(1.39849213082922,-3.67596365052876,15.7305626339841));
#24899=CARTESIAN_POINT('Ctrl Pts',(1.50673060912077,-3.63478515298788,15.7364351482715));
#24900=CARTESIAN_POINT('Ctrl Pts',(1.61300856122449,-3.58887540405998,15.7423076625589));
#24901=CARTESIAN_POINT('Ctrl Pts',(1.71689910560843,-3.53846668221717,15.7481801768463));
#24902=CARTESIAN_POINT('Ctrl Pts',(1.74561222476891,-3.52453479221136,15.7498032138946));
#24903=CARTESIAN_POINT('Ctrl Pts',(1.77414314549015,-3.51025950694262,15.751426250943));
#24904=CARTESIAN_POINT('Ctrl Pts',(1.80248324664458,-3.49564631299644,15.7530492879913));
#24905=CARTESIAN_POINT('Ctrl Pts',(1.90501731224751,-3.44277599405928,15.7589214119573));
#24906=CARTESIAN_POINT('Ctrl Pts',(2.00539511951483,-3.38530193005916,15.7647935359233));
#24907=CARTESIAN_POINT('Ctrl Pts',(2.10317463802229,-3.32342375299627,15.7706656598894));
#24908=CARTESIAN_POINT('Ctrl Pts',(2.20082738344259,-3.26162580221853,15.7765301705301));
#24909=CARTESIAN_POINT('Ctrl Pts',(2.29588819318185,-3.19543531256549,15.7823946811708));
#24910=CARTESIAN_POINT('Ctrl Pts',(2.38793803052643,-3.12509855242448,15.7882591918115));
#24911=CARTESIAN_POINT('Ctrl Pts',(2.47989314950407,-3.05483416810996,15.7941176679291));
#24912=CARTESIAN_POINT('Ctrl Pts',(2.56884313216152,-2.98043224901516,15.7999761440467));
#24913=CARTESIAN_POINT('Ctrl Pts',(2.6543970101716,-2.90218288748178,15.8058346201643));
#24914=CARTESIAN_POINT('Ctrl Pts',(2.74332439091927,-2.82084804997131,15.8119241037556));
#24915=CARTESIAN_POINT('Ctrl Pts',(2.82858194670939,-2.73535635161227,15.8180135873469));
#24916=CARTESIAN_POINT('Ctrl Pts',(2.90976730660895,-2.64608072843398,15.8241030709381));
#24917=CARTESIAN_POINT('Ctrl Pts',(2.98778231505551,-2.56029138778261,15.8299547554585));
#24918=CARTESIAN_POINT('Ctrl Pts',(3.06203689980441,-2.47100844159403,15.8358064399789));
#24919=CARTESIAN_POINT('Ctrl Pts',(3.13221145697249,-2.37860051055453,15.8416581244993));
#24920=CARTESIAN_POINT('Ctrl Pts',(3.20237531099515,-2.28620667373328,15.8475089165107));
#24921=CARTESIAN_POINT('Ctrl Pts',(3.26846012479541,-2.19068912889503,15.853359708522));
#24922=CARTESIAN_POINT('Ctrl Pts',(3.33018734607039,-2.09244862304255,15.8592105005333));
#24923=CARTESIAN_POINT('Ctrl Pts',(3.3919201035679,-1.99419930614543,15.8650618172934));
#24924=CARTESIAN_POINT('Ctrl Pts',(3.44929427165568,-1.89322689282006,15.8709131340535));
#24925=CARTESIAN_POINT('Ctrl Pts',(3.50207568797934,-1.78995946201696,15.8767644508137));
#24926=CARTESIAN_POINT('Ctrl Pts',(3.55487462238606,-1.6866577568886,15.8826177096182));
#24927=CARTESIAN_POINT('Ctrl Pts',(3.60307758595123,-1.58105988758726,15.8884709684227));
#24928=CARTESIAN_POINT('Ctrl Pts',(3.64649757084386,-1.47361611888233,15.8943242272272));
#24929=CARTESIAN_POINT('Ctrl Pts',(3.68996695443863,-1.36605011193295,15.9001841452554));
#24930=CARTESIAN_POINT('Ctrl Pts',(3.72864234313907,-1.25663439742065,15.9060440632835));
#24931=CARTESIAN_POINT('Ctrl Pts',(3.76238581878008,-1.1458367905782,15.9119039813116));
#24932=CARTESIAN_POINT('Ctrl Pts',(3.79615201486897,-1.03496458053606,15.9177678449902));
#24933=CARTESIAN_POINT('Ctrl Pts',(3.82497958296128,-0.922709024863492,
15.9236317086689));
#24934=CARTESIAN_POINT('Ctrl Pts',(3.84878157612253,-0.809548873941413,
15.9294955723475));
#24935=CARTESIAN_POINT('Ctrl Pts',(3.87261868294634,-0.696221784589936,
15.9353680866349));
#24936=CARTESIAN_POINT('Ctrl Pts',(3.89141535113761,-0.581987842983668,
15.9412406009223));
#24937=CARTESIAN_POINT('Ctrl Pts',(3.90513636504672,-0.467331756239275,
15.9471131152097));
#24938=CARTESIAN_POINT('Ctrl Pts',(3.90892855912671,-0.435643271972237,
15.948736152258));
#24939=CARTESIAN_POINT('Ctrl Pts',(3.91233335555995,-0.403922544238162,
15.9503591893064));
#24940=CARTESIAN_POINT('Ctrl Pts',(3.91535071258213,-0.372179791878329,
15.9519822263547));
#24941=CARTESIAN_POINT('Ctrl Pts',(3.92703457166852,-0.249264988340128,
15.9582669768915));
#24942=CARTESIAN_POINT('Ctrl Pts',(3.9329316565498,-0.125791461216173,15.9645517274283));
#24943=CARTESIAN_POINT('Ctrl Pts',(3.93299940944748,-0.00215529249517274,
15.9708364779651));
#24944=CARTESIAN_POINT('',(3.93121378987206,-0.00244485579717362,17.2208359355727));
#24945=CARTESIAN_POINT('Ctrl Pts',(3.93806424214966,-0.00212304094380579,
15.9708382561933));
#24946=CARTESIAN_POINT('Ctrl Pts',(3.93025982083623,1.18025118297352,16.0308638923682));
#24947=CARTESIAN_POINT('Ctrl Pts',(2.73404304350042,3.68246309584126,16.1572005079975));
#24948=CARTESIAN_POINT('Ctrl Pts',(-1.52657745030475,4.39475809013145,16.3498481030817));
#24949=CARTESIAN_POINT('Ctrl Pts',(-4.52281588537782,1.09017147712084,16.5487810414449));
#24950=CARTESIAN_POINT('Ctrl Pts',(-3.36120918071239,-3.21661471520144,
16.7477139798085));
#24951=CARTESIAN_POINT('Ctrl Pts',(0.890372355971627,-4.56635242291656,
16.9466469181718));
#24952=CARTESIAN_POINT('Ctrl Pts',(3.61197945872188,-2.30845509392336,17.1043539150494));
#24953=CARTESIAN_POINT('Ctrl Pts',(3.93082923382665,-0.499818402315335,
17.1957499324723));
#24954=CARTESIAN_POINT('Ctrl Pts',(3.92803675183412,-0.00246202408810856,
17.2208349704406));
#24955=CARTESIAN_POINT('',(3.93299884326148,0.00301643894015496,18.4708364780099));
#24956=CARTESIAN_POINT('Ctrl Pts',(3.93299924609258,-0.00243520742926632,
17.220836477965));
#24957=CARTESIAN_POINT('Ctrl Pts',(3.93307175716978,0.114674328524147,17.2267356713988));
#24958=CARTESIAN_POINT('Ctrl Pts',(3.92790932706125,0.231802111248879,17.2326348648325));
#24959=CARTESIAN_POINT('Ctrl Pts',(3.9175336699977,0.348452212554841,17.2385340582663));
#24960=CARTESIAN_POINT('Ctrl Pts',(3.90715675423114,0.465116465044868,17.2444339673494));
#24961=CARTESIAN_POINT('Ctrl Pts',(3.8915653883706,0.581302518492728,17.2503338764325));
#24962=CARTESIAN_POINT('Ctrl Pts',(3.87083318026104,0.696519555066647,17.2562337855156));
#24963=CARTESIAN_POINT('Ctrl Pts',(3.85009374789081,0.811776739699109,17.262135750457));
#24964=CARTESIAN_POINT('Ctrl Pts',(3.82420997992269,0.92606383820719,17.2680377153984));
#24965=CARTESIAN_POINT('Ctrl Pts',(3.79330649308746,1.03890078905566,17.2739396803398));
#24966=CARTESIAN_POINT('Ctrl Pts',(3.76236280702124,1.15188451811969,17.2798493225524));
#24967=CARTESIAN_POINT('Ctrl Pts',(3.72638646557085,1.26341394123064,17.2857589647651));
#24968=CARTESIAN_POINT('Ctrl Pts',(3.68555197737842,1.37302426127219,17.2916686069777));
#24969=CARTESIAN_POINT('Ctrl Pts',(3.64469073810305,1.48270638813419,17.2975821206563));
#24970=CARTESIAN_POINT('Ctrl Pts',(3.59896516826528,1.59046653530643,17.3034956343349));
#24971=CARTESIAN_POINT('Ctrl Pts',(3.54859718350607,1.69586173646697,17.3094091480134));
#24972=CARTESIAN_POINT('Ctrl Pts',(3.49813571336707,1.80145255614304,17.3153336374551));
#24973=CARTESIAN_POINT('Ctrl Pts',(3.44301479848032,1.9046693008178,17.3212581268969));
#24974=CARTESIAN_POINT('Ctrl Pts',(3.38350180090035,2.00509465195638,17.3271826163386));
#24975=CARTESIAN_POINT('Ctrl Pts',(3.32547312265687,2.10301528485475,17.3329593425253));
#24976=CARTESIAN_POINT('Ctrl Pts',(3.26326912317872,2.1982818815763,17.3387360687121));
#24977=CARTESIAN_POINT('Ctrl Pts',(3.19717471782663,2.29053767130999,17.3445127948988));
#24978=CARTESIAN_POINT('Ctrl Pts',(3.12998881890351,2.38431698789665,17.3503849188648));
#24979=CARTESIAN_POINT('Ctrl Pts',(3.05856069220649,2.47529497941671,17.3562570428309));
#24980=CARTESIAN_POINT('Ctrl Pts',(2.98315198438186,2.56306325284386,17.3621291667969));
#24981=CARTESIAN_POINT('Ctrl Pts',(2.90784104544422,2.65071773296182,17.3679936774376));
#24982=CARTESIAN_POINT('Ctrl Pts',(2.82856005546469,2.73517045995525,17.3738581880783));
#24983=CARTESIAN_POINT('Ctrl Pts',(2.74561346835019,2.81604255692524,17.379722698719));
#24984=CARTESIAN_POINT('Ctrl Pts',(2.66275223244848,2.89683143731215,17.3855811748366));
#24985=CARTESIAN_POINT('Ctrl Pts',(2.57623319604919,2.97404672932306,17.3914396509542));
#24986=CARTESIAN_POINT('Ctrl Pts',(2.48640010144279,3.04734368516997,17.3972981270718));
#24987=CARTESIAN_POINT('Ctrl Pts',(2.39302476892017,3.1235308370775,17.4033876106631));
#24988=CARTESIAN_POINT('Ctrl Pts',(2.29606894246767,3.19548394003025,17.4094770942544));
#24989=CARTESIAN_POINT('Ctrl Pts',(2.19595998586665,3.26285898262131,17.4155665778456));
#24990=CARTESIAN_POINT('Ctrl Pts',(2.09976036188927,3.32760297739243,17.421418262366));
#24991=CARTESIAN_POINT('Ctrl Pts',(2.00064962611799,3.388119503162,17.4272699468864));
#24992=CARTESIAN_POINT('Ctrl Pts',(1.89903886540253,3.44414581394149,17.4331216314068));
#24993=CARTESIAN_POINT('Ctrl Pts',(1.79744360253691,3.50016357949068,17.4389724234182));
#24994=CARTESIAN_POINT('Ctrl Pts',(1.69334943481464,3.55169229219669,17.4448232154295));
#24995=CARTESIAN_POINT('Ctrl Pts',(1.58719328007323,3.59851448401842,17.4506740074408));
#24996=CARTESIAN_POINT('Ctrl Pts',(1.48102760434448,3.64534087525277,17.4565253242009));
#24997=CARTESIAN_POINT('Ctrl Pts',(1.37279995223586,3.68745973961954,17.462376640961));
#24998=CARTESIAN_POINT('Ctrl Pts',(1.26296784461751,3.72470149454452,17.4682279577211));
#24999=CARTESIAN_POINT('Ctrl Pts',(1.15309928386611,3.76195560995932,17.4740812165257));
#25000=CARTESIAN_POINT('Ctrl Pts',(1.04162560004094,3.79432926455533,17.4799344753302));
#25001=CARTESIAN_POINT('Ctrl Pts',(0.929019424292374,3.82170274999083,17.4857877341347));
#25002=CARTESIAN_POINT('Ctrl Pts',(0.816285137054489,3.84910737810535,17.4916476521628));
#25003=CARTESIAN_POINT('Ctrl Pts',(0.702416188173637,3.87150038491822,17.4975075701909));
#25004=CARTESIAN_POINT('Ctrl Pts',(0.587895452026045,3.88881317852723,17.503367488219));
#25005=CARTESIAN_POINT('Ctrl Pts',(0.473297605789349,3.90613762933565,17.5092313518977));
#25006=CARTESIAN_POINT('Ctrl Pts',(0.358047508514276,3.91837501220619,17.5150952155763));
#25007=CARTESIAN_POINT('Ctrl Pts',(0.242631459507403,3.92550875363402,17.5209590792549));
#25008=CARTESIAN_POINT('Ctrl Pts',(0.127045144079103,3.9326530190456,17.5268315935423));
#25009=CARTESIAN_POINT('Ctrl Pts',(0.0112928001081183,3.93467860912628,
17.5327041078297));
#25010=CARTESIAN_POINT('Ctrl Pts',(-0.104140884177499,3.93162099855044,
17.5385766221171));
#25011=CARTESIAN_POINT('Ctrl Pts',(-0.136044279734563,3.9307759405393,17.5401996591654));
#25012=CARTESIAN_POINT('Ctrl Pts',(-0.167923376826395,3.92954290551535,
17.5418226962138));
#25013=CARTESIAN_POINT('Ctrl Pts',(-0.19976805865803,3.92792333463116,17.5434457332622));
#25014=CARTESIAN_POINT('Ctrl Pts',(-0.314981645163972,3.92206375119571,
17.5493178572282));
#25015=CARTESIAN_POINT('Ctrl Pts',(-0.430130357789709,3.91112089027479,
17.5551899811943));
#25016=CARTESIAN_POINT('Ctrl Pts',(-0.544729177393933,3.8950942380507,17.5610621051603));
#25017=CARTESIAN_POINT('Ctrl Pts',(-0.659179417353221,3.87908836469941,
17.566926615801));
#25018=CARTESIAN_POINT('Ctrl Pts',(-0.773080776440481,3.85801186435196,
17.5727911264417));
#25019=CARTESIAN_POINT('Ctrl Pts',(-0.885949940811867,3.83191619198221,
17.5786556370825));
#25020=CARTESIAN_POINT('Ctrl Pts',(-0.998702963935857,3.80584737179975,
17.5845141132001));
#25021=CARTESIAN_POINT('Ctrl Pts',(-1.11042550458523,3.77476974494996,17.5903725893177));
#25022=CARTESIAN_POINT('Ctrl Pts',(-1.22064173718814,3.73878626688319,17.5962310654353));
#25023=CARTESIAN_POINT('Ctrl Pts',(-1.33520394183874,3.70138391261131,17.6023205490266));
#25024=CARTESIAN_POINT('Ctrl Pts',(-1.4481381524386,3.65868092227344,17.6084100326178));
#25025=CARTESIAN_POINT('Ctrl Pts',(-1.55892397835458,3.61085101184072,17.6144995162091));
#25026=CARTESIAN_POINT('Ctrl Pts',(-1.66538353159525,3.56488889661426,17.6203512007295));
#25027=CARTESIAN_POINT('Ctrl Pts',(-1.76985892831254,3.51419294690333,17.6262028852499));
#25028=CARTESIAN_POINT('Ctrl Pts',(-1.87190695319748,3.4589670941729,17.6320545697703));
#25029=CARTESIAN_POINT('Ctrl Pts',(-1.97393941354044,3.40374966458544,17.6379053617816));
#25030=CARTESIAN_POINT('Ctrl Pts',(-2.07354487469328,3.3440039024304,17.6437561537929));
#25031=CARTESIAN_POINT('Ctrl Pts',(-2.17030426238952,3.27997994028224,17.6496069458043));
#25032=CARTESIAN_POINT('Ctrl Pts',(-2.26707232829107,3.21595023592031,17.6554582625644));
#25033=CARTESIAN_POINT('Ctrl Pts',(-2.36099346851071,3.14764179693681,17.6613095793245));
#25034=CARTESIAN_POINT('Ctrl Pts',(-2.45167776881409,3.07534796696289,17.6671608960847));
#25035=CARTESIAN_POINT('Ctrl Pts',(-2.54239216711838,3.00303014276115,17.6730141548892));
#25036=CARTESIAN_POINT('Ctrl Pts',(-2.62986726623438,2.92672455494373,17.6788674136937));
#25037=CARTESIAN_POINT('Ctrl Pts',(-2.71374695338671,2.84676421099191,17.6847206724983));
#25038=CARTESIAN_POINT('Ctrl Pts',(-2.79772207004415,2.76671289655234,17.6905805905264));
#25039=CARTESIAN_POINT('Ctrl Pts',(-2.87809331083056,2.68299881214709,17.6964405085545));
#25040=CARTESIAN_POINT('Ctrl Pts',(-2.95454203957627,2.59599120498827,17.7023004265826));
#25041=CARTESIAN_POINT('Ctrl Pts',(-3.03104224343892,2.5089250131175,17.7081642902613));
#25042=CARTESIAN_POINT('Ctrl Pts',(-3.10361441799898,2.41856120431631,17.7140281539399));
#25043=CARTESIAN_POINT('Ctrl Pts',(-3.1719818468881,2.32530001569956,17.7198920176185));
#25044=CARTESIAN_POINT('Ctrl Pts',(-3.24045013417226,2.23190124440701,17.7257645319059));
#25045=CARTESIAN_POINT('Ctrl Pts',(-3.30470106714789,2.13559690513959,17.7316370461933));
#25046=CARTESIAN_POINT('Ctrl Pts',(-3.36450259550358,2.03681400349902,17.7375095604807));
#25047=CARTESIAN_POINT('Ctrl Pts',(-3.38103045585743,2.00951252729004,17.739132597529));
#25048=CARTESIAN_POINT('Ctrl Pts',(-3.39721872650924,1.98202185432595,17.7407556345774));
#25049=CARTESIAN_POINT('Ctrl Pts',(-3.41306315351781,1.95435127602462,17.7423786716257));
#25050=CARTESIAN_POINT('Ctrl Pts',(-3.47038805541138,1.8542395341734,17.7482507955917));
#25051=CARTESIAN_POINT('Ctrl Pts',(-3.5234006206227,1.75143564244643,17.7541229195577));
#25052=CARTESIAN_POINT('Ctrl Pts',(-3.57183833781004,1.64634743858955,17.7599950435238));
#25053=CARTESIAN_POINT('Ctrl Pts',(-3.62021325453528,1.54139548367559,17.7658595541645));
#25054=CARTESIAN_POINT('Ctrl Pts',(-3.66402494714761,1.43416547827029,17.7717240648052));
#25055=CARTESIAN_POINT('Ctrl Pts',(-3.70305555447318,1.32509190642964,17.7775885754459));
#25056=CARTESIAN_POINT('Ctrl Pts',(-3.74204599969215,1.21613057020918,17.7834470515635));
#25057=CARTESIAN_POINT('Ctrl Pts',(-3.77626500667312,1.10532982769805,17.7893055276811));
#25058=CARTESIAN_POINT('Ctrl Pts',(-3.8055420951674,0.993145690172851,17.7951640037988));
#25059=CARTESIAN_POINT('Ctrl Pts',(-3.83597361804242,0.876537983502165,
17.80125348739));
#25060=CARTESIAN_POINT('Ctrl Pts',(-3.86106528119461,0.758435952410947,
17.8073429709813));
#25061=CARTESIAN_POINT('Ctrl Pts',(-3.88068206460635,0.639371342368892,
17.8134324545725));
#25062=CARTESIAN_POINT('Ctrl Pts',(-3.89953279736724,0.524956297961615,
17.819284139093));
#25063=CARTESIAN_POINT('Ctrl Pts',(-3.9133281493711,0.409652889081125,17.8251358236134));
#25064=CARTESIAN_POINT('Ctrl Pts',(-3.92200022669181,0.29394424952595,17.8309875081338));
#25065=CARTESIAN_POINT('Ctrl Pts',(-3.93067098133221,0.178253258053734,
17.8368383001451));
#25066=CARTESIAN_POINT('Ctrl Pts',(-3.93421998408977,0.0621575709402135,
17.8426890921564));
#25067=CARTESIAN_POINT('Ctrl Pts',(-3.93263126114136,-0.0538550266337851,
17.8485398841677));
#25068=CARTESIAN_POINT('Ctrl Pts',(-3.93104239570276,-0.169878029204725,
17.8543912009278));
#25069=CARTESIAN_POINT('Ctrl Pts',(-3.92431489420144,-0.285817514023418,
17.8602425176879));
#25070=CARTESIAN_POINT('Ctrl Pts',(-3.91248489896147,-0.401186883382818,
17.8660938344481));
#25071=CARTESIAN_POINT('Ctrl Pts',(-3.90065097736151,-0.516594543685525,
17.8719470932526));
#25072=CARTESIAN_POINT('Ctrl Pts',(-3.8837112367347,-0.631431301237319,
17.8778003520571));
#25073=CARTESIAN_POINT('Ctrl Pts',(-3.8617534587689,-0.745217568020551,
17.8836536108616));
#25074=CARTESIAN_POINT('Ctrl Pts',(-3.8397706995477,-0.859133288876737,
17.8895135288898));
#25075=CARTESIAN_POINT('Ctrl Pts',(-3.8127585863616,-0.971995727334371,
17.8953734469179));
#25076=CARTESIAN_POINT('Ctrl Pts',(-3.78085564492224,-1.08333724770249,
17.901233364946));
#25077=CARTESIAN_POINT('Ctrl Pts',(-3.7489312223195,-1.19475373750237,17.9070972286246));
#25078=CARTESIAN_POINT('Ctrl Pts',(-3.71210954521198,-1.30464687903708,
17.9129610923032));
#25079=CARTESIAN_POINT('Ctrl Pts',(-3.67057786678098,-1.41256756436554,
17.9188249559819));
#25080=CARTESIAN_POINT('Ctrl Pts',(-3.62898491913876,-1.52064745865242,
17.9246974702693));
#25081=CARTESIAN_POINT('Ctrl Pts',(-3.58266826726465,-1.62674871175149,
17.9305699845567));
#25082=CARTESIAN_POINT('Ctrl Pts',(-3.53186182366675,-1.73044533531846,
17.9364424988441));
#25083=CARTESIAN_POINT('Ctrl Pts',(-3.51782001189447,-1.75910485892281,
17.9380655358924));
#25084=CARTESIAN_POINT('Ctrl Pts',(-3.50343550553537,-1.78758086959021,
17.9396885729407));
#25085=CARTESIAN_POINT('Ctrl Pts',(-3.48871382416943,-1.81586476728007,
17.9413116099891));
#25086=CARTESIAN_POINT('Ctrl Pts',(-3.43545099935727,-1.91819548958095,
17.9471837339551));
#25087=CARTESIAN_POINT('Ctrl Pts',(-3.37759272571528,-2.0183523285669,17.9530558579211));
#25088=CARTESIAN_POINT('Ctrl Pts',(-3.3153403275674,-2.11589402201653,17.9589279818872));
#25089=CARTESIAN_POINT('Ctrl Pts',(-3.25316864088984,-2.21330925072377,
17.9647924925279));
#25090=CARTESIAN_POINT('Ctrl Pts',(-3.18661437946492,-2.30811573127728,
17.9706570031686));
#25091=CARTESIAN_POINT('Ctrl Pts',(-3.11592541555321,-2.39989537370061,
17.9765215138093));
#25092=CARTESIAN_POINT('Ctrl Pts',(-3.04530918988194,-2.49158057578517,
17.9823799899269));
#25093=CARTESIAN_POINT('Ctrl Pts',(-2.97056697500449,-2.58024480924499,
17.9882384660445));
#25094=CARTESIAN_POINT('Ctrl Pts',(-2.8919903592605,-2.6654982202103,17.9940969421621));
#25095=CARTESIAN_POINT('Ctrl Pts',(-2.81031536347259,-2.75411328609943,
18.0001864257534));
#25096=CARTESIAN_POINT('Ctrl Pts',(-2.72449759953192,-2.83904262555192,
18.0062759093447));
#25097=CARTESIAN_POINT('Ctrl Pts',(-2.63491154255046,-2.91988529961955,
18.0123653929359));
#25098=CARTESIAN_POINT('Ctrl Pts',(-2.54882389077738,-2.99757100438251,
18.0182170774563));
#25099=CARTESIAN_POINT('Ctrl Pts',(-2.45925706845335,-3.07148292612135,
18.0240687619767));
#25100=CARTESIAN_POINT('Ctrl Pts',(-2.36658091822905,-3.14130287579439,
18.0299204464971));
#25101=CARTESIAN_POINT('Ctrl Pts',(-2.27391890313226,-3.21111217640736,
18.0357712385085));
#25102=CARTESIAN_POINT('Ctrl Pts',(-2.17814883317635,-3.27683049719832,
18.0416220305198));
#25103=CARTESIAN_POINT('Ctrl Pts',(-2.07967251978953,-3.33818082350736,
18.0474728225311));
#25104=CARTESIAN_POINT('Ctrl Pts',(-1.98118737420892,-3.39953665223574,
18.0533241392912));
#25105=CARTESIAN_POINT('Ctrl Pts',(-1.8799958536043,-3.45652348908617,18.0591754560513));
#25106=CARTESIAN_POINT('Ctrl Pts',(-1.77652693105584,-3.50890881375297,
18.0650267728115));
#25107=CARTESIAN_POINT('Ctrl Pts',(-1.67302366730741,-3.56131152504048,
18.070880031616));
#25108=CARTESIAN_POINT('Ctrl Pts',(-1.56724186726331,-3.60910950069661,
18.0767332904205));
#25109=CARTESIAN_POINT('Ctrl Pts',(-1.45963250897119,-3.65211745960538,
18.082586549225));
#25110=CARTESIAN_POINT('Ctrl Pts',(-1.351900724044,-3.69517434845643,18.0884464672531));
#25111=CARTESIAN_POINT('Ctrl Pts',(-1.24233761494981,-3.73343018982693,
18.0943063852812));
#25112=CARTESIAN_POINT('Ctrl Pts',(-1.13141152196709,-3.76674885915694,
18.1001663033093));
#25113=CARTESIAN_POINT('Ctrl Pts',(-1.02041073927112,-3.80008996290063,
18.106030166988));
#25114=CARTESIAN_POINT('Ctrl Pts',(-0.90804554512757,-3.82848717414714,
18.1118940306666));
#25115=CARTESIAN_POINT('Ctrl Pts',(-0.79479501956925,-3.85185538109466,
18.1177578943453));
#25116=CARTESIAN_POINT('Ctrl Pts',(-0.681377422257287,-3.87525806176577,
18.1236304086327));
#25117=CARTESIAN_POINT('Ctrl Pts',(-0.567072293497158,-3.89361686589707,
18.1295029229201));
#25118=CARTESIAN_POINT('Ctrl Pts',(-0.452364471787731,-3.90689843541705,
18.1353754372075));
#25119=CARTESIAN_POINT('Ctrl Pts',(-0.420661689085492,-3.91056917648912,
18.1369984742558));
#25120=CARTESIAN_POINT('Ctrl Pts',(-0.388928147598308,-3.91385239920676,
18.1386215113041));
#25121=CARTESIAN_POINT('Ctrl Pts',(-0.35717406625248,-3.91674810096292,
18.1402445483525));
#25122=CARTESIAN_POINT('Ctrl Pts',(-0.242288270958812,-3.92722470696411,
18.1461166723185));
#25123=CARTESIAN_POINT('Ctrl Pts',(-0.126748531622461,-3.93265985724264,
18.1519887962845));
#25124=CARTESIAN_POINT('Ctrl Pts',(-0.0110349298696812,-3.93298451946137,
18.1578609202506));
#25125=CARTESIAN_POINT('Ctrl Pts',(0.104528646901102,-3.93330876074908,
18.1637254308913));
#25126=CARTESIAN_POINT('Ctrl Pts',(0.220265228227679,-3.92853568923793,
18.169589941532));
#25127=CARTESIAN_POINT('Ctrl Pts',(0.335689078507512,-3.918647961041,18.1754544521727));
#25128=CARTESIAN_POINT('Ctrl Pts',(0.450994158793534,-3.90877040721803,
18.1813129282904));
#25129=CARTESIAN_POINT('Ctrl Pts',(0.565986738678701,-3.89378870000194,
18.187171404408));
#25130=CARTESIAN_POINT('Ctrl Pts',(0.680181219717037,-3.87373753735901,
18.1930298805256));
#25131=CARTESIAN_POINT('Ctrl Pts',(0.798878540408689,-3.8528957308126,18.1991193641168));
#25132=CARTESIAN_POINT('Ctrl Pts',(0.916713072146176,-3.82657645198841,
18.2052088477081));
#25133=CARTESIAN_POINT('Ctrl Pts',(1.03314510135539,-3.79487815345175,18.2112983312994));
#25134=CARTESIAN_POINT('Ctrl Pts',(1.14503036925909,-3.76441769812899,18.2171500158198));
#25135=CARTESIAN_POINT('Ctrl Pts',(1.2556201802534,-3.72899056812071,18.2230017003402));
#25136=CARTESIAN_POINT('Ctrl Pts',(1.36444695313568,-3.68873603177006,18.2288533848606));
#25137=CARTESIAN_POINT('Ctrl Pts',(1.47325712756938,-3.64848763511128,18.2347041768719));
#25138=CARTESIAN_POINT('Ctrl Pts',(1.58030441092155,-3.60341343945687,18.2405549688833));
#25139=CARTESIAN_POINT('Ctrl Pts',(1.68513859357947,-3.55370186150006,18.2464057608946));
#25140=CARTESIAN_POINT('Ctrl Pts',(1.78998217865871,-3.50398582498605,18.2522570776547));
#25141=CARTESIAN_POINT('Ctrl Pts',(1.89261189489906,-3.44963175650102,18.2581083944148));
#25142=CARTESIAN_POINT('Ctrl Pts',(1.99260029536081,-3.3908749701114,18.2639597111749));
#25143=CARTESIAN_POINT('Ctrl Pts',(2.09262188184213,-3.33209868242109,18.2698129699795));
#25144=CARTESIAN_POINT('Ctrl Pts',(2.19000005314559,-3.26891698055241,18.275666228784));
#25145=CARTESIAN_POINT('Ctrl Pts',(2.28433522102667,-3.2016092200606,18.2815194875885));
#25146=CARTESIAN_POINT('Ctrl Pts',(2.37877771356199,-3.13422488386235,18.2873794056166));
#25147=CARTESIAN_POINT('Ctrl Pts',(2.47016995586057,-3.06270535980759,18.2932393236447));
#25148=CARTESIAN_POINT('Ctrl Pts',(2.55814434041753,-2.98737117439226,18.2990992416729));
#25149=CARTESIAN_POINT('Ctrl Pts',(2.64617796064519,-2.91198626431403,18.3049631053515));
#25150=CARTESIAN_POINT('Ctrl Pts',(2.73078883963628,-2.83278186028382,18.3108269690301));
#25151=CARTESIAN_POINT('Ctrl Pts',(2.8116464909517,-2.75011509030422,18.3166908327087));
#25152=CARTESIAN_POINT('Ctrl Pts',(2.89262342674343,-2.66732636696332,18.3225633469961));
#25153=CARTESIAN_POINT('Ctrl Pts',(2.96983580951722,-2.58106539029127,18.3284358612835));
#25154=CARTESIAN_POINT('Ctrl Pts',(3.04299358901262,-2.49172209871569,18.3343083755709));
#25155=CARTESIAN_POINT('Ctrl Pts',(3.06321283083729,-2.46702952835285,18.3359314126193));
#25156=CARTESIAN_POINT('Ctrl Pts',(3.08312261895461,-2.44210168159748,18.3375544496676));
#25157=CARTESIAN_POINT('Ctrl Pts',(3.10271742939726,-2.41694715567272,18.339177486716));
#25158=CARTESIAN_POINT('Ctrl Pts',(3.17362919680151,-2.32591530329725,18.345051104427));
#25159=CARTESIAN_POINT('Ctrl Pts',(3.2406541608105,-2.23160238625361,18.3509247221381));
#25160=CARTESIAN_POINT('Ctrl Pts',(3.30347337664496,-2.13437406510619,18.3567983398492));
#25161=CARTESIAN_POINT('Ctrl Pts',(3.36621262879894,-2.03726950759229,18.3626644809293));
#25162=CARTESIAN_POINT('Ctrl Pts',(3.42475655384322,-1.93725726609145,18.3685306220095));
#25163=CARTESIAN_POINT('Ctrl Pts',(3.47882638485046,-1.83473594396259,18.3743967630897));
#25164=CARTESIAN_POINT('Ctrl Pts',(3.53284042763407,-1.73232040138471,18.380256851597));
#25165=CARTESIAN_POINT('Ctrl Pts',(3.58238936433424,-1.62740128815385,18.3861169401043));
#25166=CARTESIAN_POINT('Ctrl Pts',(3.62723809044619,-1.52040548381552,18.3919770286117));
#25167=CARTESIAN_POINT('Ctrl Pts',(3.67205135476632,-1.41349428083085,18.3978324835595));
#25168=CARTESIAN_POINT('Ctrl Pts',(3.71217164172726,-1.30451003165297,18.4036879385074));
#25169=CARTESIAN_POINT('Ctrl Pts',(3.74741043586753,-1.1939028541515,18.4095433934553));
#25170=CARTESIAN_POINT('Ctrl Pts',(3.78263174744206,-1.08335055075398,18.4153959434123));
#25171=CARTESIAN_POINT('Ctrl Pts',(3.81297625756179,-0.97117731256335,18.4212484933693));
#25172=CARTESIAN_POINT('Ctrl Pts',(3.83830434792709,-0.857851229925077,
18.4271010433263));
#25173=CARTESIAN_POINT('Ctrl Pts',(3.86362502022341,-0.744558338130938,
18.4329518791935));
#25174=CARTESIAN_POINT('Ctrl Pts',(3.88393210851618,-0.630113676515642,
18.4388027150608));
#25175=CARTESIAN_POINT('Ctrl Pts',(3.89913662050626,-0.514997684098689,
18.4446535509281));
#25176=CARTESIAN_POINT('Ctrl Pts',(3.91434347859188,-0.399863928986253,
18.4505052895945));
#25177=CARTESIAN_POINT('Ctrl Pts',(3.92444613159445,-0.284059044919621,
18.4563570282608));
#25178=CARTESIAN_POINT('Ctrl Pts',(3.92940725097593,-0.168070389949481,
18.4622087669272));
#25179=CARTESIAN_POINT('Ctrl Pts',(3.93184544965431,-0.111066443156551,
18.4650846706065));
#25180=CARTESIAN_POINT('Ctrl Pts',(3.93304258631382,-0.0540181731665422,
18.4679605742858));
#25181=CARTESIAN_POINT('Ctrl Pts',(3.93299884326216,0.00301643805224686,
18.4708364779651));
#25182=CARTESIAN_POINT('',(3.9344286541877,0.00130879145752274,19.720836477965));
#25183=CARTESIAN_POINT('Ctrl Pts',(3.93299884326148,0.00301643894014107,
18.4708364780099));
#25184=CARTESIAN_POINT('Ctrl Pts',(3.93289556899613,0.137671101008563,18.4776262821271));
#25185=CARTESIAN_POINT('Ctrl Pts',(3.92587308724252,0.272039635390568,18.4844160862444));
#25186=CARTESIAN_POINT('Ctrl Pts',(3.91204290149561,0.405474212321595,18.4912058903616));
#25187=CARTESIAN_POINT('Ctrl Pts',(3.89813028468773,0.539704089760308,18.4980361632598));
#25188=CARTESIAN_POINT('Ctrl Pts',(3.87732868566575,0.672988727294203,18.504866436158));
#25189=CARTESIAN_POINT('Ctrl Pts',(3.84980074140044,0.804688294628814,18.5116967090562));
#25190=CARTESIAN_POINT('Ctrl Pts',(3.8220865626637,0.93727884746791,18.5185731907177));
#25191=CARTESIAN_POINT('Ctrl Pts',(3.78755480536809,1.06826269831912,18.5254496723793));
#25192=CARTESIAN_POINT('Ctrl Pts',(3.74641956867559,1.19700852772427,18.5323261540408));
#25193=CARTESIAN_POINT('Ctrl Pts',(3.73488569762663,1.23310745200056,18.534254244387));
#25194=CARTESIAN_POINT('Ctrl Pts',(3.72283295874,1.26903056256492,18.5361823347332));
#25195=CARTESIAN_POINT('Ctrl Pts',(3.71026673143481,1.30476426284905,18.5381104250794));
#25196=CARTESIAN_POINT('Ctrl Pts',(3.67199547269048,1.41359356031859,18.5439825490454));
#25197=CARTESIAN_POINT('Ctrl Pts',(3.62886773218841,1.52092002594415,18.5498546730115));
#25198=CARTESIAN_POINT('Ctrl Pts',(3.58102047321423,1.62627838035822,18.5557267969775));
#25199=CARTESIAN_POINT('Ctrl Pts',(3.53323524916138,1.73150013557375,18.5615913076182));
#25200=CARTESIAN_POINT('Ctrl Pts',(3.48074284437102,1.83475848103836,18.5674558182589));
#25201=CARTESIAN_POINT('Ctrl Pts',(3.42372957695507,1.93560450089449,18.5733203288996));
#25202=CARTESIAN_POINT('Ctrl Pts',(3.36677497562405,2.03634675119955,18.5791788050172));
#25203=CARTESIAN_POINT('Ctrl Pts',(3.30530896679639,2.13468125551295,18.5850372811348));
#25204=CARTESIAN_POINT('Ctrl Pts',(3.23956513538153,2.23018087464233,18.5908957572524));
#25205=CARTESIAN_POINT('Ctrl Pts',(3.17122893760747,2.32944617025604,18.5969852408437));
#25206=CARTESIAN_POINT('Ctrl Pts',(3.09827080447404,2.42564800037014,18.603074724435));
#25207=CARTESIAN_POINT('Ctrl Pts',(3.02100481017409,2.51833654162921,18.6091642080262));
#25208=CARTESIAN_POINT('Ctrl Pts',(2.94675611305191,2.60740552325554,18.6150158925466));
#25209=CARTESIAN_POINT('Ctrl Pts',(2.86852998137564,2.69323011273485,18.620867577067));
#25210=CARTESIAN_POINT('Ctrl Pts',(2.78664759427774,2.77544306108161,18.6267192615874));
#25211=CARTESIAN_POINT('Ctrl Pts',(2.70477769602373,2.85764347016671,18.6325700535987));
#25212=CARTESIAN_POINT('Ctrl Pts',(2.61925294280469,2.93623304055476,18.63842084561));
#25213=CARTESIAN_POINT('Ctrl Pts',(2.53043197900288,3.01088076808757,18.6442716376214));
#25214=CARTESIAN_POINT('Ctrl Pts',(2.4416030489812,3.0855351906638,18.6501229543815));
#25215=CARTESIAN_POINT('Ctrl Pts',(2.3494776371911,3.15624680158455,18.6559742711416));
#25216=CARTESIAN_POINT('Ctrl Pts',(2.25444756340317,3.22272480734324,18.6618255879018));
#25217=CARTESIAN_POINT('Ctrl Pts',(2.15938594925779,3.28922487706526,18.6676788467063));
#25218=CARTESIAN_POINT('Ctrl Pts',(2.06141809473088,3.35148831077146,18.6735321055108));
#25219=CARTESIAN_POINT('Ctrl Pts',(1.96096427781162,3.40926797144882,18.6793853643153));
#25220=CARTESIAN_POINT('Ctrl Pts',(1.86039617508168,3.46711336776036,18.6852452823434));
#25221=CARTESIAN_POINT('Ctrl Pts',(1.75733682338817,3.52046460300261,18.6911052003716));
#25222=CARTESIAN_POINT('Ctrl Pts',(1.65223063365683,3.56912075071802,18.6969651183997));
#25223=CARTESIAN_POINT('Ctrl Pts',(1.54705367291993,3.61780966001016,18.7028289820783));
#25224=CARTESIAN_POINT('Ctrl Pts',(1.43982751143665,3.66179703041352,18.7086928457569));
#25225=CARTESIAN_POINT('Ctrl Pts',(1.33101439926356,3.70093091923547,18.7145567094356));
#25226=CARTESIAN_POINT('Ctrl Pts',(1.22204076158831,3.7401225399523,18.720429223723));
#25227=CARTESIAN_POINT('Ctrl Pts',(1.11147589410163,3.77444626684249,18.7263017380104));
#25228=CARTESIAN_POINT('Ctrl Pts',(0.999795059351643,3.80380057827642,18.7321742522977));
#25229=CARTESIAN_POINT('Ctrl Pts',(0.968928870949349,3.81191348063042,18.7337972893461));
#25230=CARTESIAN_POINT('Ctrl Pts',(0.937977483556097,3.81964709719531,18.7354203263944));
#25231=CARTESIAN_POINT('Ctrl Pts',(0.906951013230218,3.82699998165674,18.7370433634428));
#25232=CARTESIAN_POINT('Ctrl Pts',(0.794697703814234,3.8536026085711,18.7429154874088));
#25233=CARTESIAN_POINT('Ctrl Pts',(0.681084751037489,3.87530673688424,18.7487876113749));
#25234=CARTESIAN_POINT('Ctrl Pts',(0.566577668216009,3.89197620057971,18.7546597353409));
#25235=CARTESIAN_POINT('Ctrl Pts',(0.452219046101044,3.90862405198452,18.7605242459816));
#25236=CARTESIAN_POINT('Ctrl Pts',(0.336969004602777,3.92025016068099,18.7663887566223));
#25237=CARTESIAN_POINT('Ctrl Pts',(0.221305956864285,3.92676873185274,18.772253267263));
#25238=CARTESIAN_POINT('Ctrl Pts',(0.105761925251269,3.93328059547961,18.7781117433806));
#25239=CARTESIAN_POINT('Ctrl Pts',(-0.0101938570255434,3.9346953521082,
18.7839702194983));
#25240=CARTESIAN_POINT('Ctrl Pts',(-0.12607576011278,3.93097874615368,18.7898286956159));
#25241=CARTESIAN_POINT('Ctrl Pts',(-0.246527040139969,3.92711558950323,
18.7959181792071));
#25242=CARTESIAN_POINT('Ctrl Pts',(-0.366898044498936,3.91770800653887,
18.8020076627984));
#25243=CARTESIAN_POINT('Ctrl Pts',(-0.486640563731101,3.90277721138825,
18.8080971463897));
#25244=CARTESIAN_POINT('Ctrl Pts',(-0.601707044447126,3.88842947540199,
18.8139488309101));
#25245=CARTESIAN_POINT('Ctrl Pts',(-0.716192755698779,3.86898185972451,
18.8198005154305));
#25246=CARTESIAN_POINT('Ctrl Pts',(-0.829615130417031,3.84450617575042,
18.8256521999509));
#25247=CARTESIAN_POINT('Ctrl Pts',(-0.943020205757641,3.82003422485018,
18.8315029919622));
#25248=CARTESIAN_POINT('Ctrl Pts',(-1.05536186303409,3.79053581765028,18.8373537839735));
#25249=CARTESIAN_POINT('Ctrl Pts',(-1.16616778882778,3.75613387518344,18.8432045759848));
#25250=CARTESIAN_POINT('Ctrl Pts',(-1.27698365263991,3.72172884725761,18.849055892745));
#25251=CARTESIAN_POINT('Ctrl Pts',(-1.3862631163148,3.68241953238886,18.8549072095051));
#25252=CARTESIAN_POINT('Ctrl Pts',(-1.49354977511157,3.63837849450331,18.8607585262652));
#25253=CARTESIAN_POINT('Ctrl Pts',(-1.6008720422103,3.5943228394548,18.8666117850698));
#25254=CARTESIAN_POINT('Ctrl Pts',(-1.70619980701989,3.54553249555648,18.8724650438743));
#25255=CARTESIAN_POINT('Ctrl Pts',(-1.80909802186465,3.49222756235693,18.8783183026788));
#25256=CARTESIAN_POINT('Ctrl Pts',(-1.9121133034995,3.43886198439853,18.8841782207069));
#25257=CARTESIAN_POINT('Ctrl Pts',(-2.0126931508247,3.3809717556427,18.8900381387351));
#25258=CARTESIAN_POINT('Ctrl Pts',(-2.11042835948061,3.31882225186887,18.8958980567632));
#25259=CARTESIAN_POINT('Ctrl Pts',(-2.20822937604956,3.25663090105552,18.9017619204418));
#25260=CARTESIAN_POINT('Ctrl Pts',(-2.30318160218773,3.19017480116358,18.9076257841204));
#25261=CARTESIAN_POINT('Ctrl Pts',(-2.39490741118955,3.11976080682948,18.9134896477991));
#25262=CARTESIAN_POINT('Ctrl Pts',(-2.48676853781311,3.04924293492424,18.9193621620865));
#25263=CARTESIAN_POINT('Ctrl Pts',(-2.57539343244822,2.97475578032093,18.9252346763739));
#25264=CARTESIAN_POINT('Ctrl Pts',(-2.66043986350973,2.8966443918176,18.9311071906613));
#25265=CARTESIAN_POINT('Ctrl Pts',(-2.6839448737467,2.87505607866349,18.9327302277096));
#25266=CARTESIAN_POINT('Ctrl Pts',(-2.70717677414301,2.85319112929916,18.9343532647579));
#25267=CARTESIAN_POINT('Ctrl Pts',(-2.73012888152008,2.8310572742864,18.9359763018063));
#25268=CARTESIAN_POINT('Ctrl Pts',(-2.81316926555667,2.75097731516654,18.9418484257723));
#25269=CARTESIAN_POINT('Ctrl Pts',(-2.89282252825392,2.66710640265115,18.9477205497383));
#25270=CARTESIAN_POINT('Ctrl Pts',(-2.96872255476643,2.57976266211082,18.9535926737044));
#25271=CARTESIAN_POINT('Ctrl Pts',(-3.04452417538751,2.49253216446437,18.9594571843451));
#25272=CARTESIAN_POINT('Ctrl Pts',(-3.11658196815892,2.40183810198126,18.9653216949858));
#25273=CARTESIAN_POINT('Ctrl Pts',(-3.1845652322769,2.30803667244981,18.9711862056265));
#25274=CARTESIAN_POINT('Ctrl Pts',(-3.25247854229245,2.21433176365613,18.9770446817441));
#25275=CARTESIAN_POINT('Ctrl Pts',(-3.31632542188778,2.11752618041993,18.9829031578617));
#25276=CARTESIAN_POINT('Ctrl Pts',(-3.37581463799054,2.01801004207828,18.9887616339793));
#25277=CARTESIAN_POINT('Ctrl Pts',(-3.43764959268571,1.91456985057931,18.9948511175706));
#25278=CARTESIAN_POINT('Ctrl Pts',(-3.49477585847065,1.80820128818851,19.0009406011619));
#25279=CARTESIAN_POINT('Ctrl Pts',(-3.54691506206068,1.69937710427293,19.0070300847531));
#25280=CARTESIAN_POINT('Ctrl Pts',(-3.59701818919474,1.59480258938669,19.0128817692735));
#25281=CARTESIAN_POINT('Ctrl Pts',(-3.64251624684647,1.48796104977659,19.0187334537939));
#25282=CARTESIAN_POINT('Ctrl Pts',(-3.6832089061037,1.3792973406769,19.0245851383143));
#25283=CARTESIAN_POINT('Ctrl Pts',(-3.72389535884585,1.27065020515491,19.0304359303256));
#25284=CARTESIAN_POINT('Ctrl Pts',(-3.75977772554019,1.16018183978562,19.036286722337));
#25285=CARTESIAN_POINT('Ctrl Pts',(-3.7907042235979,1.04835608893021,19.0421375143483));
#25286=CARTESIAN_POINT('Ctrl Pts',(-3.82163349540714,0.936520308589818,
19.0479888311084));
#25287=CARTESIAN_POINT('Ctrl Pts',(-3.84760590478224,0.823327299230757,
19.0538401478685));
#25288=CARTESIAN_POINT('Ctrl Pts',(-3.86852003695864,0.709254343412531,
19.0596914646287));
#25289=CARTESIAN_POINT('Ctrl Pts',(-3.8894411105082,0.595143526929192,19.0655447234332));
#25290=CARTESIAN_POINT('Ctrl Pts',(-3.90530049409095,0.480152589678168,
19.0713979822377));
#25291=CARTESIAN_POINT('Ctrl Pts',(-3.91604831164449,0.364766529257176,
19.0772512410422));
#25292=CARTESIAN_POINT('Ctrl Pts',(-3.92680835693691,0.249249194685909,
19.0831111590703));
#25293=CARTESIAN_POINT('Ctrl Pts',(-3.93244519044413,0.133336251571786,
19.0889710770985));
#25294=CARTESIAN_POINT('Ctrl Pts',(-3.93296099779482,0.0175154167745557,
19.0948309951266));
#25295=CARTESIAN_POINT('Ctrl Pts',(-3.93347715245336,-0.0983834035053982,
19.1006948588052));
#25296=CARTESIAN_POINT('Ctrl Pts',(-3.928865431457,-0.214189579898975,19.1065587224838));
#25297=CARTESIAN_POINT('Ctrl Pts',(-3.91917998539294,-0.329419553298565,
19.1124225861625));
#25298=CARTESIAN_POINT('Ctrl Pts',(-3.90948025096728,-0.444819518613378,
19.1182951004499));
#25299=CARTESIAN_POINT('Ctrl Pts',(-3.8946919054861,-0.559641175925521,
19.1241676147373));
#25300=CARTESIAN_POINT('Ctrl Pts',(-3.87492036337435,-0.673410110932998,
19.1300401290246));
#25301=CARTESIAN_POINT('Ctrl Pts',(-3.86945593301628,-0.704853405479625,
19.131663166073));
#25302=CARTESIAN_POINT('Ctrl Pts',(-3.8636111551001,-0.736216373735889,
19.1332862031213));
#25303=CARTESIAN_POINT('Ctrl Pts',(-3.85738892320337,-0.767489215004342,
19.1349092401697));
#25304=CARTESIAN_POINT('Ctrl Pts',(-3.83487698049673,-0.880633890836507,
19.1407813641357));
#25305=CARTESIAN_POINT('Ctrl Pts',(-3.80734494774753,-0.992976934222328,
19.1466534881017));
#25306=CARTESIAN_POINT('Ctrl Pts',(-3.77486267961749,-1.10403838249902,
19.1525256120678));
#25307=CARTESIAN_POINT('Ctrl Pts',(-3.74242252539305,-1.21495583740279,
19.1583901227085));
#25308=CARTESIAN_POINT('Ctrl Pts',(-3.70504501399428,-1.32459460842115,
19.1642546333492));
#25309=CARTESIAN_POINT('Ctrl Pts',(-3.66285117170431,-1.43248395940212,
19.1701191439899));
#25310=CARTESIAN_POINT('Ctrl Pts',(-3.62070074645829,-1.54026229331424,
19.1759776201075));
#25311=CARTESIAN_POINT('Ctrl Pts',(-3.57374399762143,-1.64629440504661,
19.1818360962252));
#25312=CARTESIAN_POINT('Ctrl Pts',(-3.52215182078561,-1.75012443881474,
19.1876945723428));
#25313=CARTESIAN_POINT('Ctrl Pts',(-3.46852529607637,-1.85804862835121,
19.193784055934));
#25314=CARTESIAN_POINT('Ctrl Pts',(-3.40989038826873,-1.9635930687259,19.1998735395253));
#25315=CARTESIAN_POINT('Ctrl Pts',(-3.34649447007401,-2.06626807596789,
19.2059630231166));
#25316=CARTESIAN_POINT('Ctrl Pts',(-3.28557421179645,-2.16493354431272,
19.211814707637));
#25317=CARTESIAN_POINT('Ctrl Pts',(-3.22025804526277,-2.2609490963118,19.2176663921574));
#25318=CARTESIAN_POINT('Ctrl Pts',(-3.15081204299447,-2.35390579032403,
19.2235180766778));
#25319=CARTESIAN_POINT('Ctrl Pts',(-3.0813766327511,-2.44684830641979,19.2293688686891));
#25320=CARTESIAN_POINT('Ctrl Pts',(-3.00781288655098,-2.53673256105849,
19.2352196607004));
#25321=CARTESIAN_POINT('Ctrl Pts',(-2.93042908705681,-2.62318020077374,
19.2410704527117));
#25322=CARTESIAN_POINT('Ctrl Pts',(-2.85303834712496,-2.70963559384901,
19.2469217694719));
#25323=CARTESIAN_POINT('Ctrl Pts',(-2.77182714856107,-2.79265345123121,
19.252773086232));
#25324=CARTESIAN_POINT('Ctrl Pts',(-2.68714229762955,-2.87189053974732,
19.2586244029921));
#25325=CARTESIAN_POINT('Ctrl Pts',(-2.60242933990655,-2.95115392694968,
19.2644776617967));
#25326=CARTESIAN_POINT('Ctrl Pts',(-2.51424073906392,-3.02663376782738,
19.2703309206012));
#25327=CARTESIAN_POINT('Ctrl Pts',(-2.42295764194274,-3.09802602722303,
19.2761841794057));
#25328=CARTESIAN_POINT('Ctrl Pts',(-2.33157069249344,-3.16949950923909,
19.2820440974339));
#25329=CARTESIAN_POINT('Ctrl Pts',(-2.23708254559468,-3.23687587281718,
19.287904015462));
#25330=CARTESIAN_POINT('Ctrl Pts',(-2.13990476760512,-3.29989342033662,
19.2937639334901));
#25331=CARTESIAN_POINT('Ctrl Pts',(-2.04266155703657,-3.36295339937426,
19.2996277971687));
#25332=CARTESIAN_POINT('Ctrl Pts',(-1.94272546491684,-3.42164850950514,
19.3054916608474));
#25333=CARTESIAN_POINT('Ctrl Pts',(-1.84053263824569,-3.47576302522948,
19.311355524526));
#25334=CARTESIAN_POINT('Ctrl Pts',(-1.73818905258519,-3.52995737287514,
19.3172280388134));
#25335=CARTESIAN_POINT('Ctrl Pts',(-1.6335824600058,-3.579557462985,19.3231005531008));
#25336=CARTESIAN_POINT('Ctrl Pts',(-1.527169012984,-3.62439564697088,19.3289730673882));
#25337=CARTESIAN_POINT('Ctrl Pts',(-1.49775861762262,-3.63678795973978,
19.3305961044365));
#25338=CARTESIAN_POINT('Ctrl Pts',(-1.46821029221951,-3.64881682804049,
19.3322191414848));
#25339=CARTESIAN_POINT('Ctrl Pts',(-1.43853384702938,-3.66047939086547,
19.3338421785332));
#25340=CARTESIAN_POINT('Ctrl Pts',(-1.3311649085284,-3.70267437017302,19.3397143024992));
#25341=CARTESIAN_POINT('Ctrl Pts',(-1.2217579028076,-3.74021207553306,19.3455864264652));
#25342=CARTESIAN_POINT('Ctrl Pts',(-1.11075443632876,-3.77289193884161,
19.3514585504313));
#25343=CARTESIAN_POINT('Ctrl Pts',(-0.999894888048273,-3.80552943205848,
19.357323061072));
#25344=CARTESIAN_POINT('Ctrl Pts',(-0.887443388094081,-3.83332149255843,
19.3631875717127));
#25345=CARTESIAN_POINT('Ctrl Pts',(-0.773861429825642,-3.85611559570356,
19.3690520823534));
#25346=CARTESIAN_POINT('Ctrl Pts',(-0.660396346262345,-3.87888624394331,
19.374910558471));
#25347=CARTESIAN_POINT('Ctrl Pts',(-0.545803520995739,-3.89666908334434,
19.3807690345886));
#25348=CARTESIAN_POINT('Ctrl Pts',(-0.430558873189867,-3.90936159196325,
19.3866275107062));
#25349=CARTESIAN_POINT('Ctrl Pts',(-0.310769976263919,-3.92255458300996,
19.3927169942975));
#25350=CARTESIAN_POINT('Ctrl Pts',(-0.190277231330525,-3.93024741903014,
19.3988064778888));
#25351=CARTESIAN_POINT('Ctrl Pts',(-0.0696263462424803,-3.93238365014261,
19.40489596148));
#25352=CARTESIAN_POINT('Ctrl Pts',(0.0463130279362404,-3.9344364597685,
19.4107476460004));
#25353=CARTESIAN_POINT('Ctrl Pts',(0.162397970763817,-3.93135849208445,
19.4165993305208));
#25354=CARTESIAN_POINT('Ctrl Pts',(0.27814060995989,-3.92315266094644,19.4224510150412));
#25355=CARTESIAN_POINT('Ctrl Pts',(0.393865595887476,-3.91494808137606,
19.4283018070525));
#25356=CARTESIAN_POINT('Ctrl Pts',(0.509247969727086,-3.90161722266105,
19.4341525990639));
#25357=CARTESIAN_POINT('Ctrl Pts',(0.623802789213381,-3.88321504428606,
19.4400033910752));
#25358=CARTESIAN_POINT('Ctrl Pts',(0.738367882950747,-3.86481121544712,
19.4458547078353));
#25359=CARTESIAN_POINT('Ctrl Pts',(0.852104866584206,-3.84133522834408,
19.4517060245954));
#25360=CARTESIAN_POINT('Ctrl Pts',(0.964537533390909,-3.81289343500185,
19.4575573413556));
#25361=CARTESIAN_POINT('Ctrl Pts',(1.07700751645285,-3.78444220186555,19.4634106001601));
#25362=CARTESIAN_POINT('Ctrl Pts',(1.18817192131659,-3.75102198659465,19.4692638589646));
#25363=CARTESIAN_POINT('Ctrl Pts',(1.29756896825586,-3.71278921737007,19.4751171177691));
#25364=CARTESIAN_POINT('Ctrl Pts',(1.40709047567452,-3.67451295091298,19.4809770357972));
#25365=CARTESIAN_POINT('Ctrl Pts',(1.51484022133774,-3.63141333858427,19.4868369538253));
#25366=CARTESIAN_POINT('Ctrl Pts',(1.62037561297551,-3.58369528181097,19.4926968718535));
#25367=CARTESIAN_POINT('Ctrl Pts',(1.72598206461274,-3.53594509510443,19.4985607355321));
#25368=CARTESIAN_POINT('Ctrl Pts',(1.82937082548394,-3.48357045823726,19.5044245992107));
#25369=CARTESIAN_POINT('Ctrl Pts',(1.93012470409018,-3.42682179674707,19.5102884628893));
#25370=CARTESIAN_POINT('Ctrl Pts',(2.03102721889137,-3.36998941733724,19.5161609771767));
#25371=CARTESIAN_POINT('Ctrl Pts',(2.12928674395889,-3.3087703526312,19.5220334914641));
#25372=CARTESIAN_POINT('Ctrl Pts',(2.22451573180351,-3.24345783986145,19.5279060057515));
#25373=CARTESIAN_POINT('Ctrl Pts',(2.25083498243191,-3.22540686156519,19.5295290427999));
#25374=CARTESIAN_POINT('Ctrl Pts',(2.27692294587325,-3.20704343676956,19.5311520798482));
#25375=CARTESIAN_POINT('Ctrl Pts',(2.30277191380724,-3.18837427429412,19.5327751168966));
#25376=CARTESIAN_POINT('Ctrl Pts',(2.39552458398488,-3.12138457188128,19.5385989865542));
#25377=CARTESIAN_POINT('Ctrl Pts',(2.48551964526767,-3.05022259204407,19.5444228562118));
#25378=CARTESIAN_POINT('Ctrl Pts',(2.5723534079641,-2.97514486110096,19.5502467258694));
#25379=CARTESIAN_POINT('Ctrl Pts',(2.65907424722462,-2.90016476539875,19.5560630218443));
#25380=CARTESIAN_POINT('Ctrl Pts',(2.74264164523572,-2.82127931423445,19.5618793178192));
#25381=CARTESIAN_POINT('Ctrl Pts',(2.82268126028275,-2.73878796237471,19.567695613794));
#25382=CARTESIAN_POINT('Ctrl Pts',(2.90263909582087,-2.65638089505631,19.5735059670388));
#25383=CARTESIAN_POINT('Ctrl Pts',(2.97907602415453,-2.57037555303375,19.5793163202836));
#25384=CARTESIAN_POINT('Ctrl Pts',(3.05165175501386,-2.48111075248987,19.5851266735283));
#25385=CARTESIAN_POINT('Ctrl Pts',(3.12417493538596,-2.39191058662077,19.5909328196244));
#25386=CARTESIAN_POINT('Ctrl Pts',(3.19284221354518,-2.29945598111866,19.5967389657204));
#25387=CARTESIAN_POINT('Ctrl Pts',(3.25735159402052,-2.20412104770405,19.6025451118165));
#25388=CARTESIAN_POINT('Ctrl Pts',(3.32183656168728,-2.10882219266227,19.6083490606455));
#25389=CARTESIAN_POINT('Ctrl Pts',(3.38216652316824,-2.01064552406509,19.6141530094745));
#25390=CARTESIAN_POINT('Ctrl Pts',(3.43808149197777,-1.90999598285439,19.6199569583036));
#25391=CARTESIAN_POINT('Ctrl Pts',(3.49398939829731,-1.80935915445374,19.6257601740493));
#25392=CARTESIAN_POINT('Ctrl Pts',(3.54548321634294,-1.70625044237268,19.631563389795));
#25393=CARTESIAN_POINT('Ctrl Pts',(3.59234822072463,-1.6011006405147,19.6373666055408));
#25394=CARTESIAN_POINT('Ctrl Pts',(3.63921912209722,-1.49593760773028,19.6431705515011));
#25395=CARTESIAN_POINT('Ctrl Pts',(3.68145988153625,-1.38873335948787,19.6489744974614));
#25396=CARTESIAN_POINT('Ctrl Pts',(3.7189036818442,-1.27993921932476,19.6547784434217));
#25397=CARTESIAN_POINT('Ctrl Pts',(3.75638418468743,-1.17103843879034,19.6605880784288));
#25398=CARTESIAN_POINT('Ctrl Pts',(3.78905820137532,-1.06054505287451,19.6663977134359));
#25399=CARTESIAN_POINT('Ctrl Pts',(3.81680863206719,-0.948926164765915,
19.672207348443));
#25400=CARTESIAN_POINT('Ctrl Pts',(3.84457316313211,-0.83725056157499,19.6780199354051));
#25401=CARTESIAN_POINT('Ctrl Pts',(3.86740904317258,-0.724448729830302,
19.6838325223671));
#25402=CARTESIAN_POINT('Ctrl Pts',(3.8852505658126,-0.610996760100171,19.6896451093291));
#25403=CARTESIAN_POINT('Ctrl Pts',(3.90311995945255,-0.497367562231769,
19.69546677638));
#25404=CARTESIAN_POINT('Ctrl Pts',(3.91597936556538,-0.383086616055516,
19.7012884434309));
#25405=CARTESIAN_POINT('Ctrl Pts',(3.92381506326595,-0.268634229552435,
19.7071101104818));
#25406=CARTESIAN_POINT('Ctrl Pts',(3.92997341763335,-0.17868201582306,19.7116855663095));
#25407=CARTESIAN_POINT('Ctrl Pts',(3.93302969846842,-0.0886240110624213,
19.7162610221373));
#25408=CARTESIAN_POINT('Ctrl Pts',(3.9329997823937,0.00130831614195257,
19.720836477965));
#25409=CARTESIAN_POINT('',(3.93299832388421,-0.00363102244798902,20.9708364779651));
#25410=CARTESIAN_POINT('Ctrl Pts',(3.93900201824057,0.00131031279145309,
19.720836477965));
#25411=CARTESIAN_POINT('Ctrl Pts',(3.93931038383691,0.0726474573565517,
19.7244603370634));
#25412=CARTESIAN_POINT('Ctrl Pts',(3.90516583393947,1.44904206919199,19.7943951756155));
#25413=CARTESIAN_POINT('Ctrl Pts',(2.29631571635523,4.04614279448815,19.9306409936241));
#25414=CARTESIAN_POINT('Ctrl Pts',(-2.16378473825673,4.11854015265543,20.1295739319866));
#25415=CARTESIAN_POINT('Ctrl Pts',(-4.6347080772386,0.404744884258939,20.3285068703506));
#25416=CARTESIAN_POINT('Ctrl Pts',(-2.84492327743589,-3.68113419044451,
20.5274398087137));
#25417=CARTESIAN_POINT('Ctrl Pts',(1.56021238382014,-4.3829299218592,20.7263727470772));
#25418=CARTESIAN_POINT('Ctrl Pts',(3.76741191265789,-1.91077193019647,20.8741716368277));
#25419=CARTESIAN_POINT('Ctrl Pts',(3.93595010307849,-0.303549133925586,
20.9556595471236));
#25420=CARTESIAN_POINT('Ctrl Pts',(3.93316774256311,-0.00363117885869044,
20.9708364779651));
#25421=CARTESIAN_POINT('',(3.93299999067832,0.000270784605071274,22.220836477992));
#25422=CARTESIAN_POINT('Ctrl Pts',(3.93299832388421,-0.00363102244798902,
20.9708364779651));
#25423=CARTESIAN_POINT('Ctrl Pts',(3.93310381018972,0.110628106685084,20.9766187057418));
#25424=CARTESIAN_POINT('Ctrl Pts',(3.92822601209407,0.225031196093933,20.9824009335186));
#25425=CARTESIAN_POINT('Ctrl Pts',(3.91835408310254,0.339102166660221,20.9881831612953));
#25426=CARTESIAN_POINT('Ctrl Pts',(3.90848950901343,0.453088150709805,20.9939610811277));
#25427=CARTESIAN_POINT('Ctrl Pts',(3.89363823801213,0.566742085803051,20.9997390009601));
#25428=CARTESIAN_POINT('Ctrl Pts',(3.87384149043578,0.679588924996797,21.0055169207924));
#25429=CARTESIAN_POINT('Ctrl Pts',(3.8540524889173,0.792391609556333,21.0112925798442));
#25430=CARTESIAN_POINT('Ctrl Pts',(3.829321928639,0.904387407412825,21.0170682388961));
#25431=CARTESIAN_POINT('Ctrl Pts',(3.79974267999181,1.0151081547543,21.0228438979479));
#25432=CARTESIAN_POINT('Ctrl Pts',(3.77016739867057,1.12581405164098,21.0286187823377));
#25433=CARTESIAN_POINT('Ctrl Pts',(3.73574483136308,1.23524482716285,21.0343936667274));
#25434=CARTESIAN_POINT('Ctrl Pts',(3.69661838113476,1.34294510098388,21.0401685511172));
#25435=CARTESIAN_POINT('Ctrl Pts',(3.65748711683048,1.45065862612968,21.0459441460425));
#25436=CARTESIAN_POINT('Ctrl Pts',(3.61365096553608,1.55664082706948,21.0517197409677));
#25437=CARTESIAN_POINT('Ctrl Pts',(3.56530205503563,1.66045483418209,21.057495335893));
#25438=CARTESIAN_POINT('Ctrl Pts',(3.51690448632742,1.76437331941999,21.0632767433608));
#25439=CARTESIAN_POINT('Ctrl Pts',(3.46398526895846,1.86611886724229,21.0690581508285));
#25440=CARTESIAN_POINT('Ctrl Pts',(3.40678324459325,1.96527782370805,21.0748395582963));
#25441=CARTESIAN_POINT('Ctrl Pts',(3.34955186696935,2.06448766366148,21.0806239324974));
#25442=CARTESIAN_POINT('Ctrl Pts',(3.2880335359382,2.16110791166841,21.0864083066984));
#25443=CARTESIAN_POINT('Ctrl Pts',(3.2225102417811,2.2547542530431,21.0921926808995));
#25444=CARTESIAN_POINT('Ctrl Pts',(3.15688054523395,2.34855266544335,21.0979864482675));
#25445=CARTESIAN_POINT('Ctrl Pts',(3.08723315492587,2.43936718858691,21.1037802156355));
#25446=CARTESIAN_POINT('Ctrl Pts',(3.01389031731061,2.52684668217551,21.1095739830034));
#25447=CARTESIAN_POINT('Ctrl Pts',(2.95201081239799,2.60065331318786,21.1144621966037));
#25448=CARTESIAN_POINT('Ctrl Pts',(2.88750153904751,2.67208648082503,21.1193504102039));
#25449=CARTESIAN_POINT('Ctrl Pts',(2.82057507590323,2.74095699367821,21.1242386238041));
#25450=CARTESIAN_POINT('Ctrl Pts',(2.74017750731638,2.82368991456763,21.1301107477701));
#25451=CARTESIAN_POINT('Ctrl Pts',(2.65600199206874,2.90302121266157,21.1359828717362));
#25452=CARTESIAN_POINT('Ctrl Pts',(2.56836805608851,2.97858599480762,21.1418549957022));
#25453=CARTESIAN_POINT('Ctrl Pts',(2.48084773924625,3.05405280571329,21.1477195063429));
#25454=CARTESIAN_POINT('Ctrl Pts',(2.38987822874045,3.12576254443211,21.1535840169836));
#25455=CARTESIAN_POINT('Ctrl Pts',(2.29581698693659,3.19338587748073,21.1594485276243));
#25456=CARTESIAN_POINT('Ctrl Pts',(2.20185253321485,3.26093962679235,21.165307003742));
#25457=CARTESIAN_POINT('Ctrl Pts',(2.10480300972062,3.32441509425251,21.1711654798596));
#25458=CARTESIAN_POINT('Ctrl Pts',(2.00505964888514,3.38352254380144,21.1770239559772));
#25459=CARTESIAN_POINT('Ctrl Pts',(1.90138327520834,3.4449606783819,21.1831134395684));
#25460=CARTESIAN_POINT('Ctrl Pts',(1.79479659507585,3.50167893757552,21.1892029231597));
#25461=CARTESIAN_POINT('Ctrl Pts',(1.68577342106561,3.5534007616407,21.195292406751));
#25462=CARTESIAN_POINT('Ctrl Pts',(1.58100768680266,3.60310280824503,21.2011440912714));
#25463=CARTESIAN_POINT('Ctrl Pts',(1.47399259034375,3.64819113230166,21.2069957757918));
#25464=CARTESIAN_POINT('Ctrl Pts',(1.36517375128535,3.68846711098276,21.2128474603122));
#25465=CARTESIAN_POINT('Ctrl Pts',(1.25637150946539,3.7287369467016,21.2186982523235));
#25466=CARTESIAN_POINT('Ctrl Pts',(1.14576645965264,3.76419575298251,21.2245490443348));
#25467=CARTESIAN_POINT('Ctrl Pts',(1.03382302440939,3.79469352572787,21.2303998363461));
#25468=CARTESIAN_POINT('Ctrl Pts',(0.921869549126134,3.82519403377306,21.2362511531063));
#25469=CARTESIAN_POINT('Ctrl Pts',(0.80857784868674,3.85073251509202,21.2421024698664));
#25470=CARTESIAN_POINT('Ctrl Pts',(0.694425590751786,3.87120938453464,21.2479537866265));
#25471=CARTESIAN_POINT('Ctrl Pts',(0.580235445831579,3.89169305022346,21.2538070454311));
#25472=CARTESIAN_POINT('Ctrl Pts',(0.465184582185747,3.90711169062497,21.2596603042356));
#25473=CARTESIAN_POINT('Ctrl Pts',(0.349758184968424,3.91741728847561,21.2655135630401));
#25474=CARTESIAN_POINT('Ctrl Pts',(0.234200467709677,3.92773461095397,21.2713734810682));
#25475=CARTESIAN_POINT('Ctrl Pts',(0.118266776134782,3.93292724335107,21.2772333990964));
#25476=CARTESIAN_POINT('Ctrl Pts',(0.00244481514791298,3.932999240132,21.2830933171245));
#25477=CARTESIAN_POINT('Ctrl Pts',(-0.113455132079537,3.93307128539042,
21.2889571808031));
#25478=CARTESIAN_POINT('Ctrl Pts',(-0.229242786907232,3.92801584763683,
21.2948210444817));
#25479=CARTESIAN_POINT('Ctrl Pts',(-0.344434801273944,3.91788892998147,
21.3006849081603));
#25480=CARTESIAN_POINT('Ctrl Pts',(-0.459796751557577,3.90774707268775,
21.3065574224477));
#25481=CARTESIAN_POINT('Ctrl Pts',(-0.57456089934629,3.89251885767977,21.3124299367351));
#25482=CARTESIAN_POINT('Ctrl Pts',(-0.688253237752109,3.87231151648776,
21.3183024510225));
#25483=CARTESIAN_POINT('Ctrl Pts',(-0.719675362640237,3.86672664060698,
21.3199254880709));
#25484=CARTESIAN_POINT('Ctrl Pts',(-0.751015704397142,3.86076172775783,
21.3215485251192));
#25485=CARTESIAN_POINT('Ctrl Pts',(-0.78226447348505,3.85441970905131,21.3231715621676));
#25486=CARTESIAN_POINT('Ctrl Pts',(-0.895322056524819,3.83147437944374,
21.3290436861336));
#25487=CARTESIAN_POINT('Ctrl Pts',(-1.00755877682702,3.8035120683751,21.3349158100996));
#25488=CARTESIAN_POINT('Ctrl Pts',(-1.11849494292434,3.77060446913392,21.3407879340657));
#25489=CARTESIAN_POINT('Ctrl Pts',(-1.22928727807958,3.73773953524856,21.3466524447064));
#25490=CARTESIAN_POINT('Ctrl Pts',(-1.33878201957949,3.69994218014727,21.3525169553471));
#25491=CARTESIAN_POINT('Ctrl Pts',(-1.44650889848123,3.65733523300977,21.3583814659878));
#25492=CARTESIAN_POINT('Ctrl Pts',(-1.5541249274962,3.61477212799703,21.3642399421054));
#25493=CARTESIAN_POINT('Ctrl Pts',(-1.65997633009354,3.5674094259213,21.370098418223));
#25494=CARTESIAN_POINT('Ctrl Pts',(-1.76360790867981,3.51541976788577,21.3759568943406));
#25495=CARTESIAN_POINT('Ctrl Pts',(-1.87132581768378,3.46138008876656,21.3820463779319));
#25496=CARTESIAN_POINT('Ctrl Pts',(-1.97664480367967,3.40234118213357,21.3881358615232));
#25497=CARTESIAN_POINT('Ctrl Pts',(-2.07907613418394,3.33855229527213,21.3942253451144));
#25498=CARTESIAN_POINT('Ctrl Pts',(-2.17750744155731,3.27725441405987,21.4000770296348));
#25499=CARTESIAN_POINT('Ctrl Pts',(-2.27327200762698,3.21157081091674,21.4059287141552));
#25500=CARTESIAN_POINT('Ctrl Pts',(-2.36596191330116,3.14176912340934,21.4117803986757));
#25501=CARTESIAN_POINT('Ctrl Pts',(-2.45863768174976,3.0719780821767,21.417631190687));
#25502=CARTESIAN_POINT('Ctrl Pts',(-2.5482393920752,2.99807045406087,21.4234819826983));
#25503=CARTESIAN_POINT('Ctrl Pts',(-2.63438987487826,2.92035596925082,21.4293327747096));
#25504=CARTESIAN_POINT('Ctrl Pts',(-2.72054808438972,2.84263451434447,21.4351840914697));
#25505=CARTESIAN_POINT('Ctrl Pts',(-2.80325414406277,2.76110580093713,21.4410354082298));
#25506=CARTESIAN_POINT('Ctrl Pts',(-2.88216615214998,2.67611794796137,21.44688672499));
#25507=CARTESIAN_POINT('Ctrl Pts',(-2.96110435102948,2.59110188762834,21.4527399837945));
#25508=CARTESIAN_POINT('Ctrl Pts',(-3.03624571325674,2.50262470763229,21.458593242599));
#25509=CARTESIAN_POINT('Ctrl Pts',(-3.10728766639976,2.41106871702984,21.4644465014035));
#25510=CARTESIAN_POINT('Ctrl Pts',(-3.17841044362169,2.31940856362947,21.4703064194316));
#25511=CARTESIAN_POINT('Ctrl Pts',(-3.24542424919564,2.22466293504505,21.4761663374597));
#25512=CARTESIAN_POINT('Ctrl Pts',(-3.30806896447818,2.12724439739684,21.4820262554878));
#25513=CARTESIAN_POINT('Ctrl Pts',(-3.37075586024014,2.02976026505954,21.4878901191665));
#25514=CARTESIAN_POINT('Ctrl Pts',(-3.42906760045181,1.9295999964155,21.4937539828451));
#25515=CARTESIAN_POINT('Ctrl Pts',(-3.4827901324422,1.82720056188784,21.4996178465237));
#25516=CARTESIAN_POINT('Ctrl Pts',(-3.5365919180839,1.72465006357414,21.5054903608111));
#25517=CARTESIAN_POINT('Ctrl Pts',(-3.58579080844062,1.61985417941031,21.5113628750985));
#25518=CARTESIAN_POINT('Ctrl Pts',(-3.6302209040578,1.51326970092637,21.5172353893859));
#25519=CARTESIAN_POINT('Ctrl Pts',(-3.64250042995079,1.48381203613512,21.5188584264342));
#25520=CARTESIAN_POINT('Ctrl Pts',(-3.6544159855181,1.45421783497541,21.5204814634826));
#25521=CARTESIAN_POINT('Ctrl Pts',(-3.66596474736453,1.42449691859285,21.522104500531));
#25522=CARTESIAN_POINT('Ctrl Pts',(-3.70774799641897,1.3169670839792,21.527976624497));
#25523=CARTESIAN_POINT('Ctrl Pts',(-3.7448661961721,1.20741704303183,21.533848748463));
#25524=CARTESIAN_POINT('Ctrl Pts',(-3.7771204721572,1.09628916751512,21.5397208724291));
#25525=CARTESIAN_POINT('Ctrl Pts',(-3.80933292983303,0.985305371495616,
21.5455853830698));
#25526=CARTESIAN_POINT('Ctrl Pts',(-3.8366938902624,0.872748202407449,21.5514498937105));
#25527=CARTESIAN_POINT('Ctrl Pts',(-3.8590525982954,0.759079734671854,21.5573144043512));
#25528=CARTESIAN_POINT('Ctrl Pts',(-3.88138829944023,0.645528230658984,
21.5631728804688));
#25529=CARTESIAN_POINT('Ctrl Pts',(-3.89873190703991,0.530868105702198,
21.5690313565864));
#25530=CARTESIAN_POINT('Ctrl Pts',(-3.9109827235493,0.415575668319147,21.574889832704));
#25531=CARTESIAN_POINT('Ctrl Pts',(-3.92371660598155,0.295737097409332,
21.5809793162952));
#25532=CARTESIAN_POINT('Ctrl Pts',(-3.9309476767346,0.175215759367503,21.5870687998865));
#25533=CARTESIAN_POINT('Ctrl Pts',(-3.93262157740627,0.054557574346977,
21.5931582834778));
#25534=CARTESIAN_POINT('Ctrl Pts',(-3.93423011095468,-0.0613888146960827,
21.5990099679982));
#25535=CARTESIAN_POINT('Ctrl Pts',(-3.93070734706526,-0.1774611110071,21.6048616525186));
#25536=CARTESIAN_POINT('Ctrl Pts',(-3.92205806902059,-0.293171457052866,
21.610713337039));
#25537=CARTESIAN_POINT('Ctrl Pts',(-3.91341011017883,-0.408864154755554,
21.6165641290503));
#25538=CARTESIAN_POINT('Ctrl Pts',(-3.89963722266148,-0.524194599809603,
21.6224149210616));
#25539=CARTESIAN_POINT('Ctrl Pts',(-3.88079622377034,-0.638678064105779,
21.6282657130729));
#25540=CARTESIAN_POINT('Ctrl Pts',(-3.86195353505806,-0.753171796253405,
21.634117029833));
#25541=CARTESIAN_POINT('Ctrl Pts',(-3.83804189850357,-0.866817988683255,
21.6399683465931));
#25542=CARTESIAN_POINT('Ctrl Pts',(-3.80916949009844,-0.979140845692379,
21.6458196633533));
#25543=CARTESIAN_POINT('Ctrl Pts',(-3.78028749897864,-1.09150098251116,
21.6516729221578));
#25544=CARTESIAN_POINT('Ctrl Pts',(-3.74644156496945,-1.20253651037752,
21.6575261809623));
#25545=CARTESIAN_POINT('Ctrl Pts',(-3.70778988456892,-1.31178625236292,
21.6633794397669));
#25546=CARTESIAN_POINT('Ctrl Pts',(-3.66909423034274,-1.42116028723954,
21.669239357795));
#25547=CARTESIAN_POINT('Ctrl Pts',(-3.62558205476129,-1.52874409108368,
21.6750992758231));
#25548=CARTESIAN_POINT('Ctrl Pts',(-3.57745995368959,-1.6340958600239,21.6809591938513));
#25549=CARTESIAN_POINT('Ctrl Pts',(-3.52930545062997,-1.73951856532536,
21.6868230575299));
#25550=CARTESIAN_POINT('Ctrl Pts',(-3.476535029194,-1.84270587599386,21.6926869212085));
#25551=CARTESIAN_POINT('Ctrl Pts',(-3.41940071169139,-1.94324156318365,
21.6985507848872));
#25552=CARTESIAN_POINT('Ctrl Pts',(-3.36218210733394,-2.04392556468334,
21.7044232991746));
#25553=CARTESIAN_POINT('Ctrl Pts',(-3.30058697739615,-2.14194978678147,
21.710295813462));
#25554=CARTESIAN_POINT('Ctrl Pts',(-3.23491004197727,-2.23692780847183,
21.7161683277494));
#25555=CARTESIAN_POINT('Ctrl Pts',(-3.21675834507387,-2.26317769743533,
21.7177913647977));
#25556=CARTESIAN_POINT('Ctrl Pts',(-3.19829509022018,-2.2891951036651,21.719414401846));
#25557=CARTESIAN_POINT('Ctrl Pts',(-3.17952701572355,-2.31497234460459,
21.7210374388944));
#25558=CARTESIAN_POINT('Ctrl Pts',(-3.11162440058543,-2.40823401996461,
21.7269095628604));
#25559=CARTESIAN_POINT('Ctrl Pts',(-3.03950115054583,-2.49866194169334,
21.7327816868264));
#25560=CARTESIAN_POINT('Ctrl Pts',(-2.96342203433715,-2.58584973391825,
21.7386538107924));
#25561=CARTESIAN_POINT('Ctrl Pts',(-2.88744155621313,-2.67292448543948,
21.7445183214332));
#25562=CARTESIAN_POINT('Ctrl Pts',(-2.80751568065602,-2.75676715288993,
21.7503828320739));
#25563=CARTESIAN_POINT('Ctrl Pts',(-2.72395175620129,-2.83700120371633,
21.7562473427146));
#25564=CARTESIAN_POINT('Ctrl Pts',(-2.64047381819366,-2.91715269450247,
21.7621058188322));
#25565=CARTESIAN_POINT('Ctrl Pts',(-2.55336557373237,-2.99370266985572,
21.7679642949498));
#25566=CARTESIAN_POINT('Ctrl Pts',(-2.46297339703016,-3.06630902642276,
21.7738227710674));
#25567=CARTESIAN_POINT('Ctrl Pts',(-2.36901693706379,-3.14177834780629,
21.7799122546586));
#25568=CARTESIAN_POINT('Ctrl Pts',(-2.27151253646121,-3.21298630502146,
21.7860017382499));
#25569=CARTESIAN_POINT('Ctrl Pts',(-2.17089018282705,-3.2795921719179,21.7920912218412));
#25570=CARTESIAN_POINT('Ctrl Pts',(-2.07419721036999,-3.34359702790358,
21.7979429063616));
#25571=CARTESIAN_POINT('Ctrl Pts',(-1.97462560932936,-3.4033522293723,21.803794590882));
#25572=CARTESIAN_POINT('Ctrl Pts',(-1.87258846806875,-3.45859818846537,
21.8096462754024));
#25573=CARTESIAN_POINT('Ctrl Pts',(-1.77056688969027,-3.51383572134874,
21.8154970674137));
#25574=CARTESIAN_POINT('Ctrl Pts',(-1.66608088224018,-3.56456518255316,
21.821347859425));
#25575=CARTESIAN_POINT('Ctrl Pts',(-1.55956901731825,-3.61057245879666,
21.8271986514363));
#25576=CARTESIAN_POINT('Ctrl Pts',(-1.45304759950628,-3.65658386136404,
21.8330499681964));
#25577=CARTESIAN_POINT('Ctrl Pts',(-1.34450034257092,-3.69787207309831,
21.8389012849566));
#25578=CARTESIAN_POINT('Ctrl Pts',(-1.23438605356345,-3.73427102267204,
21.8447526017167));
#25579=CARTESIAN_POINT('Ctrl Pts',(-1.12423521776663,-3.7706820530098,21.8506058605212));
#25580=CARTESIAN_POINT('Ctrl Pts',(-1.01251670803692,-3.80220046479243,
21.8564591193257));
#25581=CARTESIAN_POINT('Ctrl Pts',(-0.899704059044844,-3.82871017525984,
21.8623123781303));
#25582=CARTESIAN_POINT('Ctrl Pts',(-0.78676306366016,-3.85525004569369,
21.8681722961584));
#25583=CARTESIAN_POINT('Ctrl Pts',(-0.672725847122139,-3.8767697463796,
21.8740322141865));
#25584=CARTESIAN_POINT('Ctrl Pts',(-0.558075795289308,-3.89320438799612,
21.8798921322146));
#25585=CARTESIAN_POINT('Ctrl Pts',(-0.443348546295274,-3.90965009552719,
21.8857559958932));
#25586=CARTESIAN_POINT('Ctrl Pts',(-0.328008050780501,-3.92100388590197,
21.8916198595719));
#25587=CARTESIAN_POINT('Ctrl Pts',(-0.212540720783978,-3.92725291291618,
21.8974837232505));
#25588=CARTESIAN_POINT('Ctrl Pts',(-0.0969030487144911,-3.93351115874766,
21.9033562375379));
#25589=CARTESIAN_POINT('Ctrl Pts',(0.0188614194313403,-3.93464960718324,
21.9092287518253));
#25590=CARTESIAN_POINT('Ctrl Pts',(0.134268281523294,-3.93070744632271,
21.9151012661127));
#25591=CARTESIAN_POINT('Ctrl Pts',(0.166164264001246,-3.92961791757673,
21.916724303161));
#25592=CARTESIAN_POINT('Ctrl Pts',(0.198032975418511,-3.9281406094255,21.9183473402094));
#25593=CARTESIAN_POINT('Ctrl Pts',(0.229864310321648,-3.92627704051056,
21.9199703772578));
#25594=CARTESIAN_POINT('Ctrl Pts',(0.345029607837563,-3.91953467581919,
21.9258425012238));
#25595=CARTESIAN_POINT('Ctrl Pts',(0.460091077063301,-3.90770968008665,
21.9317146251898));
#25596=CARTESIAN_POINT('Ctrl Pts',(0.574563709162917,-3.89080525651348,
21.9375867491559));
#25597=CARTESIAN_POINT('Ctrl Pts',(0.688887925222219,-3.87392274986111,
21.9434512597966));
#25598=CARTESIAN_POINT('Ctrl Pts',(0.802624417161421,-3.85197397153181,
21.9493157704373));
#25599=CARTESIAN_POINT('Ctrl Pts',(0.915290279661123,-3.82501407892283,
21.955180281078));
#25600=CARTESIAN_POINT('Ctrl Pts',(1.02784021010917,-3.79808192777513,21.9610387571956));
#25601=CARTESIAN_POINT('Ctrl Pts',(1.13932130274485,-3.76614901427635,21.9668972333132));
#25602=CARTESIAN_POINT('Ctrl Pts',(1.24925853498099,-3.72932193740057,21.9727557094309));
#25603=CARTESIAN_POINT('Ctrl Pts',(1.36353073791085,-3.69104272010116,21.9788451930221));
#25604=CARTESIAN_POINT('Ctrl Pts',(1.47613437252864,-3.64747549872448,21.9849346766134));
#25605=CARTESIAN_POINT('Ctrl Pts',(1.58655039477646,-3.5987979722172,21.9910241602047));
#25606=CARTESIAN_POINT('Ctrl Pts',(1.69265458546996,-3.55202134098317,21.9968758447251));
#25607=CARTESIAN_POINT('Ctrl Pts',(1.79673839959062,-3.5005262201031,22.0027275292455));
#25608=CARTESIAN_POINT('Ctrl Pts',(1.89836019769853,-3.44451993168772,22.0085792137659));
#25609=CARTESIAN_POINT('Ctrl Pts',(1.99996649627292,-3.38852218544894,22.0144300057772));
#25610=CARTESIAN_POINT('Ctrl Pts',(2.09911116350122,-3.32801483922488,22.0202807977885));
#25611=CARTESIAN_POINT('Ctrl Pts',(2.19537705434484,-3.26325122987124,22.0261315897998));
#25612=CARTESIAN_POINT('Ctrl Pts',(2.29165157913314,-3.19848181196574,22.0319829065599));
#25613=CARTESIAN_POINT('Ctrl Pts',(2.38504647123927,-3.12945560284899,22.0378342233201));
#25614=CARTESIAN_POINT('Ctrl Pts',(2.4751740759537,-3.05646892569297,22.0436855400802));
#25615=CARTESIAN_POINT('Ctrl Pts',(2.56533159390193,-2.98345802435453,22.0495387988847));
#25616=CARTESIAN_POINT('Ctrl Pts',(2.65221934707578,-2.90648430126819,22.0553920576892));
#25617=CARTESIAN_POINT('Ctrl Pts',(2.73548378520078,-2.82588348324973,22.0612453164937));
#25618=CARTESIAN_POINT('Ctrl Pts',(2.81884295286569,-2.74519096607879,22.0671052345219));
#25619=CARTESIAN_POINT('Ctrl Pts',(2.89857028040793,-2.66086340524392,22.07296515255));
#25620=CARTESIAN_POINT('Ctrl Pts',(2.97434997078581,-2.57327247902091,22.0788250705781));
#25621=CARTESIAN_POINT('Ctrl Pts',(3.05018068579784,-2.48562257532066,22.0846889342567));
#25622=CARTESIAN_POINT('Ctrl Pts',(3.12205821516943,-2.39470525445788,22.0905527979354));
#25623=CARTESIAN_POINT('Ctrl Pts',(3.18970891792406,-2.30092286244362,22.096416661614));
#25624=CARTESIAN_POINT('Ctrl Pts',(3.2574594217304,-2.20700211885319,22.1022891759014));
#25625=CARTESIAN_POINT('Ctrl Pts',(3.3209704279015,-2.11020821282023,22.1081616901888));
#25626=CARTESIAN_POINT('Ctrl Pts',(3.38001316534968,-2.0109699157528,22.1140342044762));
#25627=CARTESIAN_POINT('Ctrl Pts',(3.39633131216481,-1.98354257801035,22.1156572415245));
#25628=CARTESIAN_POINT('Ctrl Pts',(3.41230842931794,-1.95592865155571,22.1172802785729));
#25629=CARTESIAN_POINT('Ctrl Pts',(3.42794033419869,-1.92813746013447,22.1189033156213));
#25630=CARTESIAN_POINT('Ctrl Pts',(3.48709305513061,-1.82297275992373,22.1250450531969));
#25631=CARTESIAN_POINT('Ctrl Pts',(3.54148206867059,-1.71494248824927,22.1311867907725));
#25632=CARTESIAN_POINT('Ctrl Pts',(3.59083306109141,-1.60449584835016,22.1373285283481));
#25633=CARTESIAN_POINT('Ctrl Pts',(3.64009789866522,-1.4942420214604,22.1434595439416));
#25634=CARTESIAN_POINT('Ctrl Pts',(3.68434208599632,-1.38158055357559,22.149590559535));
#25635=CARTESIAN_POINT('Ctrl Pts',(3.7233365365936,-1.26698620168776,22.1557215751284));
#25636=CARTESIAN_POINT('Ctrl Pts',(3.7622449950462,-1.15264455791443,22.1618390703575));
#25637=CARTESIAN_POINT('Ctrl Pts',(3.79592667883969,-1.03637886525183,22.1679565655866));
#25638=CARTESIAN_POINT('Ctrl Pts',(3.82420041927633,-0.918683924539212,
22.1740740608157));
#25639=CARTESIAN_POINT('Ctrl Pts',(3.852436873825,-0.801144193583254,22.1801834886211));
#25640=CARTESIAN_POINT('Ctrl Pts',(3.87527950163816,-0.682179314835842,
22.1862929164266));
#25641=CARTESIAN_POINT('Ctrl Pts',(3.89259646878022,-0.56230039235246,22.192402344232));
#25642=CARTESIAN_POINT('Ctrl Pts',(3.90988544907727,-0.442615212387448,
22.1985018982756));
#25643=CARTESIAN_POINT('Ctrl Pts',(3.92166651738104,-0.322019287346637,
22.2046014523193));
#25644=CARTESIAN_POINT('Ctrl Pts',(3.92785872762779,-0.201034364719644,
22.2107010063629));
#25645=CARTESIAN_POINT('Ctrl Pts',(3.93128853963601,-0.13402185643831,22.214079496897));
#25646=CARTESIAN_POINT('Ctrl Pts',(3.93300461466183,-0.0668902083912315,
22.217457987431));
#25647=CARTESIAN_POINT('Ctrl Pts',(3.93299999067836,0.000270784070820302,
22.2208364779651));
#25648=CARTESIAN_POINT('',(3.93299840446441,0.00354266571990603,23.4708364779354));
#25649=CARTESIAN_POINT('Ctrl Pts',(3.93299999067832,0.000270784605066124,
22.220836477992));
#25650=CARTESIAN_POINT('Ctrl Pts',(3.93299155737701,0.122759926744457,22.2269982155136));
#25651=CARTESIAN_POINT('Ctrl Pts',(3.92725664341562,0.245125961169734,22.2331599530353));
#25652=CARTESIAN_POINT('Ctrl Pts',(3.91585532059348,0.366832534243778,22.2393216905569));
#25653=CARTESIAN_POINT('Ctrl Pts',(3.90443577122667,0.488733671608779,22.245493278443));
#25654=CARTESIAN_POINT('Ctrl Pts',(3.88733176944826,0.609972902103853,22.251664866329));
#25655=CARTESIAN_POINT('Ctrl Pts',(3.86465467047957,0.730022792754059,22.2578364542151));
#25656=CARTESIAN_POINT('Ctrl Pts',(3.84191835401055,0.850386173875383,22.264024158184));
#25657=CARTESIAN_POINT('Ctrl Pts',(3.81357990986124,0.969553667335715,22.270211862153));
#25658=CARTESIAN_POINT('Ctrl Pts',(3.77980128216693,1.08701024251347,22.276399566122));
#25659=CARTESIAN_POINT('Ctrl Pts',(3.74597350573815,1.20463771989833,22.2825962733525));
#25660=CARTESIAN_POINT('Ctrl Pts',(3.70668985931787,1.32054898604482,22.288792980583));
#25661=CARTESIAN_POINT('Ctrl Pts',(3.66216074202684,1.43424813040053,22.2949896878135));
#25662=CARTESIAN_POINT('Ctrl Pts',(3.61753022850095,1.5482061764782,22.3012005054243));
#25663=CARTESIAN_POINT('Ctrl Pts',(3.5676305095443,1.65994171853242,22.3074113230352));
#25664=CARTESIAN_POINT('Ctrl Pts',(3.5127188247905,1.76898147473694,22.313622140646));
#25665=CARTESIAN_POINT('Ctrl Pts',(3.50029941521256,1.79364306358919,22.3150268450923));
#25666=CARTESIAN_POINT('Ctrl Pts',(3.48762380453704,1.81816686972331,22.3164315495385));
#25667=CARTESIAN_POINT('Ctrl Pts',(3.47469527424782,1.84254762519722,22.3178362539847));
#25668=CARTESIAN_POINT('Ctrl Pts',(3.42064978961855,1.9444671563223,22.3237083779507));
#25669=CARTESIAN_POINT('Ctrl Pts',(3.36202565092841,2.04417765018982,22.3295805019168));
#25670=CARTESIAN_POINT('Ctrl Pts',(3.29902755825593,2.14123940040994,22.3354526258828));
#25671=CARTESIAN_POINT('Ctrl Pts',(3.23611114386145,2.2381753081437,22.3413171365235));
#25672=CARTESIAN_POINT('Ctrl Pts',(3.16883227587687,2.33246895793777,22.3471816471642));
#25673=CARTESIAN_POINT('Ctrl Pts',(3.0974420233671,2.42370417169248,22.3530461578049));
#25674=CARTESIAN_POINT('Ctrl Pts',(3.02612523071679,2.51484550532008,22.3589046339226));
#25675=CARTESIAN_POINT('Ctrl Pts',(2.95070572158437,2.6029343390167,22.3647631100402));
#25676=CARTESIAN_POINT('Ctrl Pts',(2.87147806343923,2.68758306498372,22.3706215861578));
#25677=CARTESIAN_POINT('Ctrl Pts',(2.78912635378591,2.77556960234407,22.3767110697491));
#25678=CARTESIAN_POINT('Ctrl Pts',(2.70266024364892,2.85983877289532,22.3828005533403));
#25679=CARTESIAN_POINT('Ctrl Pts',(2.61245726978783,2.93999251929877,22.3888900369316));
#25680=CARTESIAN_POINT('Ctrl Pts',(2.52577679221918,3.01701619955865,22.394741721452));
#25681=CARTESIAN_POINT('Ctrl Pts',(2.43564616711387,3.09023954456871,22.4005934059724));
#25682=CARTESIAN_POINT('Ctrl Pts',(2.34243766474219,3.15934720896535,22.4064450904928));
#25683=CARTESIAN_POINT('Ctrl Pts',(2.24924337869324,3.22844433294094,22.4122958825041));
#25684=CARTESIAN_POINT('Ctrl Pts',(2.15297248077749,3.29342677827385,22.4181466745154));
#25685=CARTESIAN_POINT('Ctrl Pts',(2.05402889355913,3.3540206177697,22.4239974665267));
#25686=CARTESIAN_POINT('Ctrl Pts',(1.95507643223784,3.41461989183674,22.4298487832869));
#25687=CARTESIAN_POINT('Ctrl Pts',(1.85345115766835,3.47082956169151,22.435700100047));
#25688=CARTESIAN_POINT('Ctrl Pts',(1.74958381228125,3.52242040134385,22.4415514168072));
#25689=CARTESIAN_POINT('Ctrl Pts',(1.64568199345774,3.57402836392857,22.4474046756117));
#25690=CARTESIAN_POINT('Ctrl Pts',(1.53953699420137,3.62101426426451,22.4532579344162));
#25691=CARTESIAN_POINT('Ctrl Pts',(1.43160119924072,3.66319628280174,22.4591111932207));
#25692=CARTESIAN_POINT('Ctrl Pts',(1.32354260626005,3.70542629161281,22.4649711112489));
#25693=CARTESIAN_POINT('Ctrl Pts',(1.2136895363021,3.74284135935537,22.470831029277));
#25694=CARTESIAN_POINT('Ctrl Pts',(1.10251135909919,3.77530895464957,22.4766909473051));
#25695=CARTESIAN_POINT('Ctrl Pts',(0.991258322447728,3.80779841130489,22.4825548109837));
#25696=CARTESIAN_POINT('Ctrl Pts',(0.878678802537223,3.83533366431226,22.4884186746624));
#25697=CARTESIAN_POINT('Ctrl Pts',(0.765252517596467,3.85783327585735,22.494282538341));
#25698=CARTESIAN_POINT('Ctrl Pts',(0.651658901614758,3.88036607973897,22.5001550526284));
#25699=CARTESIAN_POINT('Ctrl Pts',(0.537216434609229,3.89784835349401,22.5060275669158));
#25700=CARTESIAN_POINT('Ctrl Pts',(0.422410196484637,3.91025045564933,22.5119000812032));
#25701=CARTESIAN_POINT('Ctrl Pts',(0.390680213595296,3.91367813079668,22.5135231182515));
#25702=CARTESIAN_POINT('Ctrl Pts',(0.358922442618301,3.91671806324577,22.5151461552998));
#25703=CARTESIAN_POINT('Ctrl Pts',(0.327147102199838,3.91937032870361,22.5167691923482));
#25704=CARTESIAN_POINT('Ctrl Pts',(0.212184391896045,3.92896618578848,22.5226413163142));
#25705=CARTESIAN_POINT('Ctrl Pts',(0.0966063925621662,3.93351572361829,
22.5285134402802));
#25706=CARTESIAN_POINT('Ctrl Pts',(-0.0191062992359001,3.932953591047,22.5343855642463));
#25707=CARTESIAN_POINT('Ctrl Pts',(-0.134668967231466,3.93239218729176,
22.540250074887));
#25708=CARTESIAN_POINT('Ctrl Pts',(-0.250365570825991,3.92673229458379,
22.5461145855277));
#25709=CARTESIAN_POINT('Ctrl Pts',(-0.365710255764052,3.91596029203936,
22.5519790961684));
#25710=CARTESIAN_POINT('Ctrl Pts',(-0.480936252168838,3.90519937377838,
22.557837572286));
#25711=CARTESIAN_POINT('Ctrl Pts',(-0.595810641049526,3.88933684689757,
22.5636960484036));
#25712=CARTESIAN_POINT('Ctrl Pts',(-0.709848104132318,3.86841112978698,
22.5695545245212));
#25713=CARTESIAN_POINT('Ctrl Pts',(-0.828382215442429,3.84666028393179,
22.5756440081125));
#25714=CARTESIAN_POINT('Ctrl Pts',(-0.946011585860243,3.8194387387382,22.5817334917038));
#25715=CARTESIAN_POINT('Ctrl Pts',(-1.06219727216408,3.78684908004098,22.587822975295));
#25716=CARTESIAN_POINT('Ctrl Pts',(-1.17384581704424,3.75553207286531,22.5936746598154));
#25717=CARTESIAN_POINT('Ctrl Pts',(-1.28416088034208,3.71925846474694,22.5995263443358));
#25718=CARTESIAN_POINT('Ctrl Pts',(-1.39267596188577,3.67817110330468,22.6053780288562));
#25719=CARTESIAN_POINT('Ctrl Pts',(-1.50117449252069,3.63709000857816,22.6112288208675));
#25720=CARTESIAN_POINT('Ctrl Pts',(-1.60787320074576,3.59119676670049,22.6170796128788));
#25721=CARTESIAN_POINT('Ctrl Pts',(-1.71232333412335,3.54068323906795,22.6229304048902));
#25722=CARTESIAN_POINT('Ctrl Pts',(-1.81678283547781,3.49016518095236,22.6287817216503));
#25723=CARTESIAN_POINT('Ctrl Pts',(-1.91899298888386,3.43502619331911,22.6346330384104));
#25724=CARTESIAN_POINT('Ctrl Pts',(-2.01852816331218,3.37550485911597,22.6404843551705));
#25725=CARTESIAN_POINT('Ctrl Pts',(-2.11809637333493,3.31596376985973,22.6463376139751));
#25726=CARTESIAN_POINT('Ctrl Pts',(-2.2149874843791,3.25203765392801,22.6521908727796));
#25727=CARTESIAN_POINT('Ctrl Pts',(-2.30880406080973,3.1840089209656,22.6580441315841));
#25728=CARTESIAN_POINT('Ctrl Pts',(-2.40272737189537,3.11590279205015,22.6639040496122));
#25729=CARTESIAN_POINT('Ctrl Pts',(-2.49356883180296,3.04368497267559,22.6697639676403));
#25730=CARTESIAN_POINT('Ctrl Pts',(-2.58096330021652,2.96767879713008,22.6756238856685));
#25731=CARTESIAN_POINT('Ctrl Pts',(-2.6684166138268,2.89162144445137,22.6814877493471));
#25732=CARTESIAN_POINT('Ctrl Pts',(-2.75241801555635,2.81177094057748,22.6873516130257));
#25733=CARTESIAN_POINT('Ctrl Pts',(-2.83263976556501,2.72848693574659,22.6932154767043));
#25734=CARTESIAN_POINT('Ctrl Pts',(-2.91297986194246,2.6450800669848,22.6990879909917));
#25735=CARTESIAN_POINT('Ctrl Pts',(-2.9895289058162,2.55822989696775,22.7049605052791));
#25736=CARTESIAN_POINT('Ctrl Pts',(-3.06199984378392,2.46832857550757,22.7108330195665));
#25737=CARTESIAN_POINT('Ctrl Pts',(-3.08202925733558,2.44348177764815,22.7124560566149));
#25738=CARTESIAN_POINT('Ctrl Pts',(-3.10174742319807,2.41840208184142,22.7140790936632));
#25739=CARTESIAN_POINT('Ctrl Pts',(-3.12114888345213,2.39309812739168,22.7157021307116));
#25740=CARTESIAN_POINT('Ctrl Pts',(-3.19134307886485,2.30154879553204,22.7215742546776));
#25741=CARTESIAN_POINT('Ctrl Pts',(-3.25762356028316,2.20675496657971,22.7274463786436));
#25742=CARTESIAN_POINT('Ctrl Pts',(-3.31967564925479,2.10908572223719,22.7333185026096));
#25743=CARTESIAN_POINT('Ctrl Pts',(-3.38164728646099,2.01154310800923,22.7391830132504));
#25744=CARTESIAN_POINT('Ctrl Pts',(-3.43940121367192,1.91113283781489,22.7450475238911));
#25745=CARTESIAN_POINT('Ctrl Pts',(-3.49266343946043,1.80825636972649,22.7509120345318));
#25746=CARTESIAN_POINT('Ctrl Pts',(-3.54587085894847,1.70548576050032,22.7567705106494));
#25747=CARTESIAN_POINT('Ctrl Pts',(-3.59459558129651,1.60025436588892,22.762628986767));
#25748=CARTESIAN_POINT('Ctrl Pts',(-3.63860769271482,1.49299131227094,22.7684874628846));
#25749=CARTESIAN_POINT('Ctrl Pts',(-3.68435525998632,1.38149873436446,22.7745769464759));
#25750=CARTESIAN_POINT('Ctrl Pts',(-3.72501067739193,1.26781136328398,22.7806664300671));
#25751=CARTESIAN_POINT('Ctrl Pts',(-3.76036904819388,1.15243812041491,22.7867559136584));
#25752=CARTESIAN_POINT('Ctrl Pts',(-3.79434664711298,1.0415702924214,22.7926075981788));
#25753=CARTESIAN_POINT('Ctrl Pts',(-3.82343301099241,0.929146223501031,
22.7984592826992));
#25754=CARTESIAN_POINT('Ctrl Pts',(-3.84749626548086,0.815635633791727,
22.8043109672196));
#25755=CARTESIAN_POINT('Ctrl Pts',(-3.87155584979993,0.702142356914769,
22.8101617592309));
#25756=CARTESIAN_POINT('Ctrl Pts',(-3.89059376233024,0.587563293061722,
22.8160125512422));
#25757=CARTESIAN_POINT('Ctrl Pts',(-3.90452896091025,0.472379713168461,
22.8218633432536));
#25758=CARTESIAN_POINT('Ctrl Pts',(-3.91846540931746,0.357185802631517,
22.8277146600137));
#25759=CARTESIAN_POINT('Ctrl Pts',(-3.92729818434212,0.24138767871805,22.8335659767738));
#25760=CARTESIAN_POINT('Ctrl Pts',(-3.9309980508903,0.125472402928658,22.839417293534));
#25761=CARTESIAN_POINT('Ctrl Pts',(-3.93469914541935,0.00951865501057846,
22.8452705523385));
#25762=CARTESIAN_POINT('Ctrl Pts',(-3.93326393078135,-0.106551909115038,
22.851123811143));
#25763=CARTESIAN_POINT('Ctrl Pts',(-3.92671528481529,-0.222252271074949,
22.8569770699475));
#25764=CARTESIAN_POINT('Ctrl Pts',(-3.9201591884871,-0.338084264764432,
22.8628369879757));
#25765=CARTESIAN_POINT('Ctrl Pts',(-3.90847807257971,-0.453544802631376,
22.8686969060038));
#25766=CARTESIAN_POINT('Ctrl Pts',(-3.8917467013407,-0.568151927395994,
22.8745568240319));
#25767=CARTESIAN_POINT('Ctrl Pts',(-3.8750040643906,-0.682836220417626,
22.8804206877105));
#25768=CARTESIAN_POINT('Ctrl Pts',(-3.85320447865518,-0.796665551098302,
22.8862845513892));
#25769=CARTESIAN_POINT('Ctrl Pts',(-3.82647347540322,-0.909169809241145,
22.8921484150678));
#25770=CARTESIAN_POINT('Ctrl Pts',(-3.79970303749459,-1.0218400382139,22.8980209293552));
#25771=CARTESIAN_POINT('Ctrl Pts',(-3.76798677530151,-1.1331808971224,22.9038934436426));
#25772=CARTESIAN_POINT('Ctrl Pts',(-3.73149955141773,-1.24273894996869,
22.90976595793));
#25773=CARTESIAN_POINT('Ctrl Pts',(-3.72141526498499,-1.27301844696287,
22.9113889949783));
#25774=CARTESIAN_POINT('Ctrl Pts',(-3.71096682649742,-1.30316189301501,
22.9130120320267));
#25775=CARTESIAN_POINT('Ctrl Pts',(-3.70015855625258,-1.33316002737512,
22.914635069075));
#25776=CARTESIAN_POINT('Ctrl Pts',(-3.66105439482814,-1.44169283252124,
22.920507193041));
#25777=CARTESIAN_POINT('Ctrl Pts',(-3.61710541139586,-1.54868563171709,
22.9263793170071));
#25778=CARTESIAN_POINT('Ctrl Pts',(-3.56845213094431,-1.65367420889334,
22.9322514409731));
#25779=CARTESIAN_POINT('Ctrl Pts',(-3.51986193043693,-1.75852666629462,
22.9381159516138));
#25780=CARTESIAN_POINT('Ctrl Pts',(-3.46657973425234,-1.86137969755053,
22.9439804622545));
#25781=CARTESIAN_POINT('Ctrl Pts',(-3.40879529535231,-1.96178582785786,
22.9498449728952));
#25782=CARTESIAN_POINT('Ctrl Pts',(-3.35107031606503,-2.06208864125602,
22.9557034490129));
#25783=CARTESIAN_POINT('Ctrl Pts',(-3.28885251381717,-2.15994920564847,
22.9615619251305));
#25784=CARTESIAN_POINT('Ctrl Pts',(-3.22237874009185,-2.25494218449256,
22.9674204012481));
#25785=CARTESIAN_POINT('Ctrl Pts',(-3.15328381741511,-2.35368086232342,
22.9735098848393));
#25786=CARTESIAN_POINT('Ctrl Pts',(-3.07959057234699,-2.44932074385276,
22.9795993684306));
#25787=CARTESIAN_POINT('Ctrl Pts',(-3.00161651713321,-2.54141442588041,
22.9856888520219));
#25788=CARTESIAN_POINT('Ctrl Pts',(-2.92668740942658,-2.62991177799109,
22.9915405365423));
#25789=CARTESIAN_POINT('Ctrl Pts',(-2.8478058477608,-2.7151343516762,22.9973922210627));
#25790=CARTESIAN_POINT('Ctrl Pts',(-2.76529581629384,-2.79671737013016,
23.0032439055831));
#25791=CARTESIAN_POINT('Ctrl Pts',(-2.68279836940026,-2.87828794540039,
23.0090946975944));
#25792=CARTESIAN_POINT('Ctrl Pts',(-2.59667384697142,-2.95621977858399,
23.0149454896057));
#25793=CARTESIAN_POINT('Ctrl Pts',(-2.50728341954824,-3.03018462375785,
23.0207962816171));
#25794=CARTESIAN_POINT('Ctrl Pts',(-2.41788497483077,-3.1041561027285,23.0266475983772));
#25795=CARTESIAN_POINT('Ctrl Pts',(-2.32522036136581,-3.17415962283936,
23.0324989151373));
#25796=CARTESIAN_POINT('Ctrl Pts',(-2.22968361594914,-3.23990740188172,
23.0383502318975));
#25797=CARTESIAN_POINT('Ctrl Pts',(-2.13411516201148,-3.30567700252606,
23.044203490702));
#25798=CARTESIAN_POINT('Ctrl Pts',(-2.03567302101211,-3.36718781924102,
23.0500567495065));
#25799=CARTESIAN_POINT('Ctrl Pts',(-1.93477935256286,-3.42419594312248,
23.055910008311));
#25800=CARTESIAN_POINT('Ctrl Pts',(-1.83377089788595,-3.48126892486457,
23.0617699263392));
#25801=CARTESIAN_POINT('Ctrl Pts',(-1.73030570895322,-3.53382878552347,
23.0676298443673));
#25802=CARTESIAN_POINT('Ctrl Pts',(-1.62482972346416,-3.5816780103392,23.0734897623954));
#25803=CARTESIAN_POINT('Ctrl Pts',(-1.51928271797545,-3.6295594534074,23.079353626074));
#25804=CARTESIAN_POINT('Ctrl Pts',(-1.41172260273204,-3.67272379135303,
23.0852174897527));
#25805=CARTESIAN_POINT('Ctrl Pts',(-1.30261277864739,-3.71102262845493,
23.0910813534313));
#25806=CARTESIAN_POINT('Ctrl Pts',(-1.1933419913392,-3.74937796554964,23.0969538677187));
#25807=CARTESIAN_POINT('Ctrl Pts',(-1.0825173266438,-3.78285335718505,23.1028263820061));
#25808=CARTESIAN_POINT('Ctrl Pts',(-0.970614811176123,-3.81135092694513,
23.1086988962935));
#25809=CARTESIAN_POINT('Ctrl Pts',(-0.939687354976457,-3.81922704426804,
23.1103219333418));
#25810=CARTESIAN_POINT('Ctrl Pts',(-0.908677608990547,-3.82672323400713,
23.1119449703901));
#25811=CARTESIAN_POINT('Ctrl Pts',(-0.877595700063661,-3.83383812741615,
23.1135680074385));
#25812=CARTESIAN_POINT('Ctrl Pts',(-0.765141814610189,-3.85957970623339,
23.1194401314045));
#25813=CARTESIAN_POINT('Ctrl Pts',(-0.651365865962822,-3.88041251050641,
23.1253122553705));
#25814=CARTESIAN_POINT('Ctrl Pts',(-0.53673439729216,-3.89620394573531,
23.1311843793366));
#25815=CARTESIAN_POINT('Ctrl Pts',(-0.422251550596726,-3.91197490705489,
23.1370488899773));
#25816=CARTESIAN_POINT('Ctrl Pts',(-0.306915795431205,-3.92271744163368,
23.142913400618));
#25817=CARTESIAN_POINT('Ctrl Pts',(-0.191206188388605,-3.92834942355207,
23.1487779112587));
#25818=CARTESIAN_POINT('Ctrl Pts',(-0.075615645380534,-3.9339756102171,
23.1546363873763));
#25819=CARTESIAN_POINT('Ctrl Pts',(0.040347573900666,-3.9345016840641,23.1604948634939));
#25820=CARTESIAN_POINT('Ctrl Pts',(0.156197591340774,-3.92989711219764,
23.1663533396115));
#25821=CARTESIAN_POINT('Ctrl Pts',(0.276615728427503,-3.9251109759631,23.1724428232028));
#25822=CARTESIAN_POINT('Ctrl Pts',(0.396911101818212,-3.9147811914345,23.1785323067941));
#25823=CARTESIAN_POINT('Ctrl Pts',(0.516535680730075,-3.89893317338637,
23.1846217903853));
#25824=CARTESIAN_POINT('Ctrl Pts',(0.631488826787063,-3.88370403277019,
23.1904734749057));
#25825=CARTESIAN_POINT('Ctrl Pts',(0.745822136886462,-3.86337961302314,
23.1963251594261));
#25826=CARTESIAN_POINT('Ctrl Pts',(0.859053608465656,-3.83803542164245,
23.2021768439465));
#25827=CARTESIAN_POINT('Ctrl Pts',(0.972267809784067,-3.81269509580186,
23.2080276359578));
#25828=CARTESIAN_POINT('Ctrl Pts',(1.08438010340764,-3.78233661090207,23.2138784279692));
#25829=CARTESIAN_POINT('Ctrl Pts',(1.194919131808,-3.74708650399737,23.2197292199805));
#25830=CARTESIAN_POINT('Ctrl Pts',(1.30546807428901,-3.71183323556314,23.2255805367406));
#25831=CARTESIAN_POINT('Ctrl Pts',(1.41444307715141,-3.67168759859444,23.2314318535007));
#25832=CARTESIAN_POINT('Ctrl Pts',(1.52138907152172,-3.62682564966312,23.2372831702608));
#25833=CARTESIAN_POINT('Ctrl Pts',(1.62837056112805,-3.58194881110946,23.2431364290654));
#25834=CARTESIAN_POINT('Ctrl Pts',(1.73332132215207,-3.53235270785558,23.2489896878699));
#25835=CARTESIAN_POINT('Ctrl Pts',(1.83580800645338,-3.47826076702735,23.2548429466744));
#25836=CARTESIAN_POINT('Ctrl Pts',(1.93841128934854,-3.42410728606556,23.2607028647025));
#25837=CARTESIAN_POINT('Ctrl Pts',(2.03854453424144,-3.3654479514241,23.2665627827306));
#25838=CARTESIAN_POINT('Ctrl Pts',(2.1358005825287,-3.30255126707672,23.2724227007588));
#25839=CARTESIAN_POINT('Ctrl Pts',(2.23312211609666,-3.23961223259172,23.2782865644374));
#25840=CARTESIAN_POINT('Ctrl Pts',(2.32756225946827,-3.17243040631849,23.284150428116));
#25841=CARTESIAN_POINT('Ctrl Pts',(2.41874574864515,-3.10131552787055,23.2900142917947));
#25842=CARTESIAN_POINT('Ctrl Pts',(2.51006375539161,-3.03009573787892,23.2958868060821));
#25843=CARTESIAN_POINT('Ctrl Pts',(2.59811520610417,-2.9549315830084,23.3017593203695));
#25844=CARTESIAN_POINT('Ctrl Pts',(2.68256052357107,-2.87617072465772,23.3076318346568));
#25845=CARTESIAN_POINT('Ctrl Pts',(2.70589939889778,-2.85440291196175,23.3092548717052));
#25846=CARTESIAN_POINT('Ctrl Pts',(2.72896305236874,-2.83236056418971,23.3108779087535));
#25847=CARTESIAN_POINT('Ctrl Pts',(2.75174486024572,-2.81005146289374,23.3125009458019));
#25848=CARTESIAN_POINT('Ctrl Pts',(2.83299241800593,-2.73048973513665,23.31828923956));
#25849=CARTESIAN_POINT('Ctrl Pts',(2.91094157765737,-2.6472492831955,23.324077533318));
#25850=CARTESIAN_POINT('Ctrl Pts',(2.98523330806928,-2.56063880631254,23.3298658270761));
#25851=CARTESIAN_POINT('Ctrl Pts',(3.06062220235696,-2.47274923839251,23.3357396041953));
#25852=CARTESIAN_POINT('Ctrl Pts',(3.13224439973583,-2.38138954781217,23.3416133813144));
#25853=CARTESIAN_POINT('Ctrl Pts',(3.19976052377038,-2.28692404563875,23.3474871584335));
#25854=CARTESIAN_POINT('Ctrl Pts',(3.26612798680753,-2.19406569789692,23.353261004184));
#25855=CARTESIAN_POINT('Ctrl Pts',(3.32852770953646,-2.09820673283369,23.3590348499344));
#25856=CARTESIAN_POINT('Ctrl Pts',(3.38667611170226,-1.99972846017284,23.3648086956848));
#25857=CARTESIAN_POINT('Ctrl Pts',(3.44478728086328,-1.90131324413712,23.3705788443839));
#25858=CARTESIAN_POINT('Ctrl Pts',(3.49865232249158,-1.80028241880843,23.3763489930831));
#25859=CARTESIAN_POINT('Ctrl Pts',(3.54803070385407,-1.69704658878558,23.3821191417822));
#25860=CARTESIAN_POINT('Ctrl Pts',(3.59739022699559,-1.59385018581644,23.3878870867894));
#25861=CARTESIAN_POINT('Ctrl Pts',(3.64226631262948,-1.48845083627596,23.3936550317966));
#25862=CARTESIAN_POINT('Ctrl Pts',(3.68246459138356,-1.38128329216214,23.3994229768038));
#25863=CARTESIAN_POINT('Ctrl Pts',(3.72393949884909,-1.27071228979112,23.4053741018981));
#25864=CARTESIAN_POINT('Ctrl Pts',(3.7604343121092,-1.1582593355855,23.4113252269924));
#25865=CARTESIAN_POINT('Ctrl Pts',(3.79178979392339,-1.04442288307871,23.4172763520867));
#25866=CARTESIAN_POINT('Ctrl Pts',(3.82219121830909,-0.934050147499971,
23.4230464015038));
#25867=CARTESIAN_POINT('Ctrl Pts',(3.84776146736264,-0.822377326441574,
23.4288164509209));
#25868=CARTESIAN_POINT('Ctrl Pts',(3.86840682438445,-0.709871566592036,
23.4345865003379));
#25869=CARTESIAN_POINT('Ctrl Pts',(3.89002402022443,-0.592069823506447,
23.4406281632708));
#25870=CARTESIAN_POINT('Ctrl Pts',(3.90624124665246,-0.473355322211236,
23.4466698262037));
#25871=CARTESIAN_POINT('Ctrl Pts',(3.91701169785944,-0.354271589084256,
23.4527114891366));
#25872=CARTESIAN_POINT('Ctrl Pts',(3.92778214906643,-0.235187855957294,
23.4587531520695));
#25873=CARTESIAN_POINT('Ctrl Pts',(3.93310584473272,-0.11573542519944,23.4647948150024));
#25874=CARTESIAN_POINT('Ctrl Pts',(3.93299840446441,0.00354266571993175,
23.4708364779354));
#25875=CARTESIAN_POINT('',(3.93503799677841,-0.00183665550588484,24.720837107935));
#25876=CARTESIAN_POINT('Ctrl Pts',(3.93299840446388,0.00354266630733597,
23.4708364779651));
#25877=CARTESIAN_POINT('Ctrl Pts',(3.93284996998897,0.16833169872891,23.4791833569372));
#25878=CARTESIAN_POINT('Ctrl Pts',(3.92234140402553,0.33267328203265,23.4875302359094));
#25879=CARTESIAN_POINT('Ctrl Pts',(3.90166060312833,0.495513408492938,23.4958771148815));
#25880=CARTESIAN_POINT('Ctrl Pts',(3.88881242960801,0.596679616283066,23.5010627046428));
#25881=CARTESIAN_POINT('Ctrl Pts',(3.87203901721538,0.697267067072719,23.506248294404));
#25882=CARTESIAN_POINT('Ctrl Pts',(3.85139390028725,0.797028245942498,23.5114338841653));
#25883=CARTESIAN_POINT('Ctrl Pts',(3.82801552068602,0.909997076160445,23.5173060081313));
#25884=CARTESIAN_POINT('Ctrl Pts',(3.79962334186979,1.02212582540236,23.5231781320974));
#25885=CARTESIAN_POINT('Ctrl Pts',(3.76629089470118,1.13293508043973,23.5290502560634));
#25886=CARTESIAN_POINT('Ctrl Pts',(3.73300166371219,1.24360066907769,23.5349147667041));
#25887=CARTESIAN_POINT('Ctrl Pts',(3.69478501988862,1.35294977334302,23.5407792773448));
#25888=CARTESIAN_POINT('Ctrl Pts',(3.65176559350328,1.46051259840702,23.5466437879855));
#25889=CARTESIAN_POINT('Ctrl Pts',(3.60879043367972,1.5679647423941,23.5525022641031));
#25890=CARTESIAN_POINT('Ctrl Pts',(3.5610224737937,1.67363388163574,23.5583607402207));
#25891=CARTESIAN_POINT('Ctrl Pts',(3.50863609792483,1.77706548341326,23.5642192163383));
#25892=CARTESIAN_POINT('Ctrl Pts',(3.45418405786262,1.884575530258,23.5703086999296));
#25893=CARTESIAN_POINT('Ctrl Pts',(3.39474201927512,1.98966751547182,23.5763981835209));
#25894=CARTESIAN_POINT('Ctrl Pts',(3.33056110036195,2.09185366523469,23.5824876671121));
#25895=CARTESIAN_POINT('Ctrl Pts',(3.26888649625462,2.19004936636518,23.5883393516325));
#25896=CARTESIAN_POINT('Ctrl Pts',(3.20283642093742,2.28556154038991,23.5941910361529));
#25897=CARTESIAN_POINT('Ctrl Pts',(3.13268007309236,2.37798329675589,23.6000427206733));
#25898=CARTESIAN_POINT('Ctrl Pts',(3.06253442561533,2.47039095679507,23.6058935126847));
#25899=CARTESIAN_POINT('Ctrl Pts',(2.98828400077268,2.55970880718149,23.611744304696));
#25900=CARTESIAN_POINT('Ctrl Pts',(2.9102399717319,2.64556086812114,23.6175950967073));
#25901=CARTESIAN_POINT('Ctrl Pts',(2.8321889430384,2.73142062900427,23.6234464134674));
#25902=CARTESIAN_POINT('Ctrl Pts',(2.7503439118771,2.81381367659168,23.6292977302276));
#25903=CARTESIAN_POINT('Ctrl Pts',(2.66505430473725,2.89239944558172,23.6351490469877));
#25904=CARTESIAN_POINT('Ctrl Pts',(2.57973639008812,2.97101129708591,23.6410023057923));
#25905=CARTESIAN_POINT('Ctrl Pts',(2.4909719300523,3.04581307735935,23.6468555645968));
#25906=CARTESIAN_POINT('Ctrl Pts',(2.3991443902885,3.11650368113808,23.6527088234013));
#25907=CARTESIAN_POINT('Ctrl Pts',(2.30721237878694,3.18727470926707,23.6585687414295));
#25908=CARTESIAN_POINT('Ctrl Pts',(2.2122106596709,3.25392497287027,23.6644286594576));
#25909=CARTESIAN_POINT('Ctrl Pts',(2.11455279276454,3.31619593610084,23.6702885774857));
#25910=CARTESIAN_POINT('Ctrl Pts',(2.0168291700216,3.37850882815302,23.6761524411644));
#25911=CARTESIAN_POINT('Ctrl Pts',(1.91644619551017,3.43643634225192,23.682016304843));
#25912=CARTESIAN_POINT('Ctrl Pts',(1.81384165666068,3.48976610169829,23.6878801685216));
#25913=CARTESIAN_POINT('Ctrl Pts',(1.71108575144737,3.54317453536181,23.693752682809));
#25914=CARTESIAN_POINT('Ctrl Pts',(1.60610211442179,3.59197150357573,23.6996251970964));
#25915=CARTESIAN_POINT('Ctrl Pts',(1.49934816946042,3.63599285845499,23.7054977113838));
#25916=CARTESIAN_POINT('Ctrl Pts',(1.46984366776866,3.64815941717073,23.7071207484321));
#25917=CARTESIAN_POINT('Ctrl Pts',(1.44020402538649,3.65996148504753,23.7087437854805));
#25918=CARTESIAN_POINT('Ctrl Pts',(1.41043907420621,3.67139627634397,23.7103668225288));
#25919=CARTESIAN_POINT('Ctrl Pts',(1.30274992234508,3.71276718164006,23.7162389464948));
#25920=CARTESIAN_POINT('Ctrl Pts',(1.19305845469911,3.74946533077813,23.7221110704609));
#25921=CARTESIAN_POINT('Ctrl Pts',(1.08180780183994,3.78129354584886,23.7279831944269));
#25922=CARTESIAN_POINT('Ctrl Pts',(0.970701387661194,3.81308049500677,23.7338477050676));
#25923=CARTESIAN_POINT('Ctrl Pts',(0.858040202120724,3.84000995362341,23.7397122157083));
#25924=CARTESIAN_POINT('Ctrl Pts',(0.744286893916885,3.86193293825042,23.745576726349));
#25925=CARTESIAN_POINT('Ctrl Pts',(0.630650636735532,3.88383336434435,23.7514352024666));
#25926=CARTESIAN_POINT('Ctrl Pts',(0.515924895647583,3.90073748548579,23.7572936785843));
#25927=CARTESIAN_POINT('Ctrl Pts',(0.400586361530627,3.91254643000638,23.7631521547019));
#25928=CARTESIAN_POINT('Ctrl Pts',(0.280699876231974,3.92482101685196,23.7692416382931));
#25929=CARTESIAN_POINT('Ctrl Pts',(0.160151714701838,3.93159021616368,23.7753311218844));
#25930=CARTESIAN_POINT('Ctrl Pts',(0.0394880013782968,3.93280176181652,
23.7814206054756));
#25931=CARTESIAN_POINT('Ctrl Pts',(-0.0764637000832616,3.93396599566924,
23.787272289996));
#25932=CARTESIAN_POINT('Ctrl Pts',(-0.192521645583175,3.92999848729928,
23.7931239745164));
#25933=CARTESIAN_POINT('Ctrl Pts',(-0.308197999498619,3.92090588934561,
23.7989756590368));
#25934=CARTESIAN_POINT('Ctrl Pts',(-0.423856710255597,3.91181467821076,
23.8048264510481));
#25935=CARTESIAN_POINT('Ctrl Pts',(-0.53913353312224,3.89759996411889,23.8106772430595));
#25936=CARTESIAN_POINT('Ctrl Pts',(-0.653543961262705,3.87832042135472,
23.8165280350708));
#25937=CARTESIAN_POINT('Ctrl Pts',(-0.76796465070406,3.85903914943707,23.8223793518309));
#25938=CARTESIAN_POINT('Ctrl Pts',(-0.88151838325822,3.83469221452669,23.828230668591));
#25939=CARTESIAN_POINT('Ctrl Pts',(-0.993729781228285,3.80538961499345,
23.8340819853512));
#25940=CARTESIAN_POINT('Ctrl Pts',(-1.10597842201484,3.77607728996567,23.8399352441557));
#25941=CARTESIAN_POINT('Ctrl Pts',(-1.21688344254404,3.74180613417956,23.8457885029602));
#25942=CARTESIAN_POINT('Ctrl Pts',(-1.32598427545659,3.70273611012746,23.8516417617647));
#25943=CARTESIAN_POINT('Ctrl Pts',(-1.43520923184712,3.66362163630224,23.8575016797928));
#25944=CARTESIAN_POINT('Ctrl Pts',(-1.5426255142142,3.61969753635932,23.8633615978209));
#25945=CARTESIAN_POINT('Ctrl Pts',(-1.64779211357196,3.57117209756825,23.8692215158491));
#25946=CARTESIAN_POINT('Ctrl Pts',(-1.75302952461081,3.52261398521051,23.8750853795277));
#25947=CARTESIAN_POINT('Ctrl Pts',(-1.85601386997222,3.46944855403648,23.8809492432063));
#25948=CARTESIAN_POINT('Ctrl Pts',(-1.95632988957507,3.41192941942755,23.8868131068849));
#25949=CARTESIAN_POINT('Ctrl Pts',(-2.05679389942559,3.35432543026586,23.8926856211723));
#25950=CARTESIAN_POINT('Ctrl Pts',(-2.1545813792603,3.29235513950045,23.8985581354597));
#25951=CARTESIAN_POINT('Ctrl Pts',(-2.24930704022988,3.2263147457699,23.9044306497471));
#25952=CARTESIAN_POINT('Ctrl Pts',(-2.27548718210084,3.20806259678109,23.9060536867955));
#25953=CARTESIAN_POINT('Ctrl Pts',(-2.30143364910498,3.18949978296568,23.9076767238438));
#25954=CARTESIAN_POINT('Ctrl Pts',(-2.32713878456223,3.17063307201988,23.9092997608922));
#25955=CARTESIAN_POINT('Ctrl Pts',(-2.42013958335605,3.10237359167248,23.9151718848582));
#25956=CARTESIAN_POINT('Ctrl Pts',(-2.51029047652954,3.02990436589693,23.9210440088242));
#25957=CARTESIAN_POINT('Ctrl Pts',(-2.59718610574472,2.95349171864872,23.9269161327903));
#25958=CARTESIAN_POINT('Ctrl Pts',(-2.68396907305125,2.87717814191489,23.932780643431));
#25959=CARTESIAN_POINT('Ctrl Pts',(-2.76750486188798,2.79693158153872,23.9386451540717));
#25960=CARTESIAN_POINT('Ctrl Pts',(-2.847418120176,2.71306082661141,23.9445096647124));
#25961=CARTESIAN_POINT('Ctrl Pts',(-2.92724914851625,2.62927637385654,23.95036814083));
#25962=CARTESIAN_POINT('Ctrl Pts',(-3.00346477711461,2.541875441727,23.9562266169476));
#25963=CARTESIAN_POINT('Ctrl Pts',(-3.07572423237954,2.45120571277755,23.9620850930652));
#25964=CARTESIAN_POINT('Ctrl Pts',(-3.15083297368294,2.35696075631136,23.9681745766565));
#25965=CARTESIAN_POINT('Ctrl Pts',(-3.22166678696586,2.25918421411733,23.9742640602478));
#25966=CARTESIAN_POINT('Ctrl Pts',(-3.28788659622261,2.15830737625106,23.9803535438391));
#25967=CARTESIAN_POINT('Ctrl Pts',(-3.35152047041967,2.06136985736918,23.9862052283595));
#25968=CARTESIAN_POINT('Ctrl Pts',(-3.41089369085765,1.96157001502884,23.9920569128799));
#25969=CARTESIAN_POINT('Ctrl Pts',(-3.46574825447171,1.85932192925978,23.9979085974003));
#25970=CARTESIAN_POINT('Ctrl Pts',(-3.52059445157244,1.75708943854639,24.0037593894116));
#25971=CARTESIAN_POINT('Ctrl Pts',(-3.57092316679509,1.65240981105857,24.0096101814229));
#25972=CARTESIAN_POINT('Ctrl Pts',(-3.61652196896533,1.54572243562393,24.0154609734342));
#25973=CARTESIAN_POINT('Ctrl Pts',(-3.66212486082419,1.43902549155754,24.0213122901944));
#25974=CARTESIAN_POINT('Ctrl Pts',(-3.70299683383611,1.33032082174698,24.0271636069545));
#25975=CARTESIAN_POINT('Ctrl Pts',(-3.73897357596759,1.22006786623373,24.0330149237146));
#25976=CARTESIAN_POINT('Ctrl Pts',(-3.77496225873282,1.10977831790849,24.0388681825192));
#25977=CARTESIAN_POINT('Ctrl Pts',(-3.80605235178819,0.99793985488568,24.0447214413237));
#25978=CARTESIAN_POINT('Ctrl Pts',(-3.83212958773443,0.885026453169818,
24.0505747001282));
#25979=CARTESIAN_POINT('Ctrl Pts',(-3.85823649162303,0.771984590435271,
24.0564346181563));
#25980=CARTESIAN_POINT('Ctrl Pts',(-3.87931906207649,0.657865751077166,
24.0622945361845));
#25981=CARTESIAN_POINT('Ctrl Pts',(-3.89531426250649,0.543153566050663,
24.0681544542126));
#25982=CARTESIAN_POINT('Ctrl Pts',(-3.91132023296269,0.428364142027082,
24.0740183178912));
#25983=CARTESIAN_POINT('Ctrl Pts',(-3.92223197378313,0.312980987391279,
24.0798821815698));
#25984=CARTESIAN_POINT('Ctrl Pts',(-3.92803850271045,0.197490559835831,
24.0857460452485));
#25985=CARTESIAN_POINT('Ctrl Pts',(-3.93385359766398,0.081829756132633,
24.0916185595359));
#25986=CARTESIAN_POINT('Ctrl Pts',(-3.93454844694656,-0.0339382244770866,
24.0974910738233));
#25987=CARTESIAN_POINT('Ctrl Pts',(-3.93016409452121,-0.149329133581845,
24.1033635881107));
#25988=CARTESIAN_POINT('Ctrl Pts',(-3.92895235350687,-0.181220706995479,
24.104986625159));
#25989=CARTESIAN_POINT('Ctrl Pts',(-3.92735294043249,-0.21308352364042,
24.1066096622073));
#25990=CARTESIAN_POINT('Ctrl Pts',(-3.92536741265095,-0.244907483956606,
24.1082326992557));
#25991=CARTESIAN_POINT('Ctrl Pts',(-3.91818380258912,-0.360046100328655,
24.1141048232217));
#25992=CARTESIAN_POINT('Ctrl Pts',(-3.90591799665363,-0.475061413349325,
24.1199769471878));
#25993=CARTESIAN_POINT('Ctrl Pts',(-3.88857505649726,-0.589468430017523,
24.1258490711538));
#25994=CARTESIAN_POINT('Ctrl Pts',(-3.87125460180716,-0.70372711571697,
24.1317135817945));
#25995=CARTESIAN_POINT('Ctrl Pts',(-3.84887016469844,-0.817378668474101,
24.1375780924352));
#25996=CARTESIAN_POINT('Ctrl Pts',(-3.8214787525788,-0.929940397869027,
24.1434426030759));
#25997=CARTESIAN_POINT('Ctrl Pts',(-3.79411552594972,-1.04238630236423,
24.1493010791935));
#25998=CARTESIAN_POINT('Ctrl Pts',(-3.76175566929711,-1.15374421477812,
24.1551595553111));
#25999=CARTESIAN_POINT('Ctrl Pts',(-3.72450760102247,-1.26353952448105,
24.1610180314288));
#26000=CARTESIAN_POINT('Ctrl Pts',(-3.6857907920757,-1.37766420868421,24.16710751502));
#26001=CARTESIAN_POINT('Ctrl Pts',(-3.64179241155865,-1.49010007404528,
24.1731969986113));
#26002=CARTESIAN_POINT('Ctrl Pts',(-3.59269214600665,-1.60032876123068,
24.1792864822025));
#26003=CARTESIAN_POINT('Ctrl Pts',(-3.54550928401644,-1.7062529324416,24.1851381667229));
#26004=CARTESIAN_POINT('Ctrl Pts',(-3.49361570877868,-1.81013866142006,
24.1909898512433));
#26005=CARTESIAN_POINT('Ctrl Pts',(-3.43722043317324,-1.91154510639334,
24.1968415357637));
#26006=CARTESIAN_POINT('Ctrl Pts',(-3.38083375907323,-2.01293608467945,
24.2026923277751));
#26007=CARTESIAN_POINT('Ctrl Pts',(-3.31994695067006,-2.11184816963082,
24.2085431197864));
#26008=CARTESIAN_POINT('Ctrl Pts',(-3.25481494139214,-2.20786519001738,
24.2143939117977));
#26009=CARTESIAN_POINT('Ctrl Pts',(-3.18967709052134,-2.30389082202744,
24.2202452285578));
#26010=CARTESIAN_POINT('Ctrl Pts',(-3.12029351397924,-2.39702053115799,
24.2260965453179));
#26011=CARTESIAN_POINT('Ctrl Pts',(-3.04696201819274,-2.4868678010081,24.2319478620781));
#26012=CARTESIAN_POINT('Ctrl Pts',(-2.97360618377854,-2.57674489104975,
24.2378011208826));
#26013=CARTESIAN_POINT('Ctrl Pts',(-2.8963000859215,-2.66333705542741,24.2436543796871));
#26014=CARTESIAN_POINT('Ctrl Pts',(-2.81538080372033,-2.7462920329133,24.2495076384916));
#26015=CARTESIAN_POINT('Ctrl Pts',(-2.73436946005198,-2.82934138786683,
24.2553675565198));
#26016=CARTESIAN_POINT('Ctrl Pts',(-2.64973701603279,-2.90874500045913,
24.2612274745479));
#26017=CARTESIAN_POINT('Ctrl Pts',(-2.56185635729329,-2.98418850017823,
24.267087392576));
#26018=CARTESIAN_POINT('Ctrl Pts',(-2.47391652599122,-3.05968279816478,
24.2729512562546));
#26019=CARTESIAN_POINT('Ctrl Pts',(-2.38272444948504,-3.13121141931702,
24.2788151199333));
#26020=CARTESIAN_POINT('Ctrl Pts',(-2.28868351938012,-3.19850226639248,
24.2846789836119));
#26021=CARTESIAN_POINT('Ctrl Pts',(-2.19450385629327,-3.26589238364594,
24.2905514978993));
#26022=CARTESIAN_POINT('Ctrl Pts',(-2.09746729692934,-3.32903202489284,
24.2964240121867));
#26023=CARTESIAN_POINT('Ctrl Pts',(-1.99800348616251,-3.38769406370801,
24.302296526474));
#26024=CARTESIAN_POINT('Ctrl Pts',(-1.97051382126889,-3.40390699358242,
24.3039195635224));
#26025=CARTESIAN_POINT('Ctrl Pts',(-1.94283887580368,-3.41977818132064,
24.3055426005707));
#26026=CARTESIAN_POINT('Ctrl Pts',(-1.91498798947108,-3.43530348007007,
24.3071656376191));
#26027=CARTESIAN_POINT('Ctrl Pts',(-1.81422389583779,-3.49147378065549,
24.3130377615851));
#26028=CARTESIAN_POINT('Ctrl Pts',(-1.71081740177547,-3.54330108243971,
24.3189098855511));
#26029=CARTESIAN_POINT('Ctrl Pts',(-1.6051793357273,-3.5905275796398,24.3247820095172));
#26030=CARTESIAN_POINT('Ctrl Pts',(-1.4996782315293,-3.63769284674855,24.3306465201579));
#26031=CARTESIAN_POINT('Ctrl Pts',(-1.39195168295005,-3.68026900439558,
24.3365110307986));
#26032=CARTESIAN_POINT('Ctrl Pts',(-1.28243664971561,-3.71804320032275,
24.3423755414393));
#26033=CARTESIAN_POINT('Ctrl Pts',(-1.17303430636084,-3.75577852697811,
24.3482340175569));
#26034=CARTESIAN_POINT('Ctrl Pts',(-1.06184752732504,-3.78872158614705,
24.3540924936745));
#26035=CARTESIAN_POINT('Ctrl Pts',(-0.949334253474952,-3.81670715082768,
24.3599509697921));
#26036=CARTESIAN_POINT('Ctrl Pts',(-0.832384432198021,-3.8457962233943,
24.3660404533834));
#26037=CARTESIAN_POINT('Ctrl Pts',(-0.714001768480387,-3.86952861136376,
24.3721299369747));
#26038=CARTESIAN_POINT('Ctrl Pts',(-0.594719524752181,-3.88777541620893,
24.3782194205659));
#26039=CARTESIAN_POINT('Ctrl Pts',(-0.480095345423647,-3.90530966913187,
24.3840711050863));
#26040=CARTESIAN_POINT('Ctrl Pts',(-0.364640973395392,-3.91777866331343,
24.3899227896067));
#26041=CARTESIAN_POINT('Ctrl Pts',(-0.248840291004333,-3.92512006307742,
24.3957744741271));
#26042=CARTESIAN_POINT('Ctrl Pts',(-0.133057270734517,-3.93246034311836,
24.4016252661384));
#26043=CARTESIAN_POINT('Ctrl Pts',(-0.0169284575948743,-3.93467455759177,
24.4074760581498));
#26044=CARTESIAN_POINT('Ctrl Pts',(0.0990582118394604,-3.93175234096289,
24.4133268501611));
#26045=CARTESIAN_POINT('Ctrl Pts',(0.215055283945308,-3.92882986224476,
24.4191781669212));
#26046=CARTESIAN_POINT('Ctrl Pts',(0.330909773696594,-3.92077004705018,
24.4250294836813));
#26047=CARTESIAN_POINT('Ctrl Pts',(0.446135531003836,-3.90761462889778,
24.4308808004415));
#26048=CARTESIAN_POINT('Ctrl Pts',(0.561399531589519,-3.89445484447927,
24.436734059246));
#26049=CARTESIAN_POINT('Ctrl Pts',(0.676033974266391,-3.87619614108461,
24.4425873180505));
#26050=CARTESIAN_POINT('Ctrl Pts',(0.78956031178076,-3.85293180760582,24.448440576855));
#26051=CARTESIAN_POINT('Ctrl Pts',(0.903215807647861,-3.82964100640989,
24.4543004948832));
#26052=CARTESIAN_POINT('Ctrl Pts',(1.01576027681901,-3.80133329134225,24.4601604129113));
#26053=CARTESIAN_POINT('Ctrl Pts',(1.12672770689481,-3.76815255457042,24.4660203309394));
#26054=CARTESIAN_POINT('Ctrl Pts',(1.23776985451707,-3.73494947625891,24.471884194618));
#26055=CARTESIAN_POINT('Ctrl Pts',(1.34723245915725,-3.69686697835184,24.4777480582967));
#26056=CARTESIAN_POINT('Ctrl Pts',(1.45466859507815,-3.6540974642849,24.4836119219753));
#26057=CARTESIAN_POINT('Ctrl Pts',(1.56226322513018,-3.61126485490173,24.4894844362627));
#26058=CARTESIAN_POINT('Ctrl Pts',(1.66782504437113,-3.56373159845388,24.4953569505501));
#26059=CARTESIAN_POINT('Ctrl Pts',(1.77093078149554,-3.51173648885442,24.5012294648375));
#26060=CARTESIAN_POINT('Ctrl Pts',(1.79942699675513,-3.49736615528313,24.5028525018858));
#26061=CARTESIAN_POINT('Ctrl Pts',(1.82773577182878,-3.48265525930262,24.5044755389342));
#26062=CARTESIAN_POINT('Ctrl Pts',(1.85584857069332,-3.46760941898818,24.5060985759825));
#26063=CARTESIAN_POINT('Ctrl Pts',(1.9575602599824,-3.41317379190853,24.5119706999485));
#26064=CARTESIAN_POINT('Ctrl Pts',(2.05704538356677,-3.35416800905721,24.5178428239146));
#26065=CARTESIAN_POINT('Ctrl Pts',(2.15386502266241,-3.29079845389405,24.5237149478806));
#26066=CARTESIAN_POINT('Ctrl Pts',(2.25055913317359,-3.22751105861737,24.5295794585213));
#26067=CARTESIAN_POINT('Ctrl Pts',(2.34459428892378,-3.15987136648445,24.535443969162));
#26068=CARTESIAN_POINT('Ctrl Pts',(2.43555527692493,-3.08813203944442,24.5413084798028));
#26069=CARTESIAN_POINT('Ctrl Pts',(2.52642266697425,-3.01646653145829,24.5471669559204));
#26070=CARTESIAN_POINT('Ctrl Pts',(2.61422185855389,-2.9407100337983,24.553025432038));
#26071=CARTESIAN_POINT('Ctrl Pts',(2.69856637544595,-2.86115859702193,24.5588839081556));
#26072=CARTESIAN_POINT('Ctrl Pts',(2.78623670836476,-2.77847034171686,24.5649733917469));
#26073=CARTESIAN_POINT('Ctrl Pts',(2.87017393604567,-2.69168196048493,24.5710628753381));
#26074=CARTESIAN_POINT('Ctrl Pts',(2.94998145073239,-2.60117251260558,24.5771523589294));
#26075=CARTESIAN_POINT('Ctrl Pts',(3.02667241989339,-2.51419752906747,24.5830040434498));
#26076=CARTESIAN_POINT('Ctrl Pts',(3.09954986129521,-2.42378698559456,24.5888557279702));
#26077=CARTESIAN_POINT('Ctrl Pts',(3.16829985836904,-2.33031435807676,24.5947074124906));
#26078=CARTESIAN_POINT('Ctrl Pts',(3.23703936957381,-2.23685598716659,24.6005582045019));
#26079=CARTESIAN_POINT('Ctrl Pts',(3.30165244326281,-2.14033679376242,24.6064089965132));
#26080=CARTESIAN_POINT('Ctrl Pts',(3.36186670201889,-2.04116174710791,24.6122597885245));
#26081=CARTESIAN_POINT('Ctrl Pts',(3.42208636130212,-1.94197780559124,24.6181111052847));
#26082=CARTESIAN_POINT('Ctrl Pts',(3.47790620680963,-1.84013789070516,24.6239624220448));
#26083=CARTESIAN_POINT('Ctrl Pts',(3.52909866476973,-1.73607362007505,24.6298137388049));
#26084=CARTESIAN_POINT('Ctrl Pts',(3.58030811343977,-1.63197481064944,24.6356669976094));
#26085=CARTESIAN_POINT('Ctrl Pts',(3.62688693828793,-1.52565054825737,24.641520256414));
#26086=CARTESIAN_POINT('Ctrl Pts',(3.66865505456452,-1.41755391100946,24.6473735152185));
#26087=CARTESIAN_POINT('Ctrl Pts',(3.71047069022049,-1.3093342927518,24.6532334332466));
#26088=CARTESIAN_POINT('Ctrl Pts',(3.7474645440102,-1.19933866076966,24.6590933512747));
#26089=CARTESIAN_POINT('Ctrl Pts',(3.77950588407603,-1.08803688918835,24.6649532693028));
#26090=CARTESIAN_POINT('Ctrl Pts',(3.81156879849311,-0.976660174938909,
24.6708171329815));
#26091=CARTESIAN_POINT('Ctrl Pts',(3.83867246276346,-0.863975970879195,
24.6766809966601));
#26092=CARTESIAN_POINT('Ctrl Pts',(3.86073727787361,-0.750464303772734,
24.6825448603387));
#26093=CARTESIAN_POINT('Ctrl Pts',(3.88283464389104,-0.636785179665933,
24.6884173746261));
#26094=CARTESIAN_POINT('Ctrl Pts',(3.89987826420005,-0.522276563585091,
24.6942898889135));
#26095=CARTESIAN_POINT('Ctrl Pts',(3.9118403562932,-0.40742364545509,24.7001624032009));
#26096=CARTESIAN_POINT('Ctrl Pts',(3.91514642209276,-0.375680761212693,
24.7017854402493));
#26097=CARTESIAN_POINT('Ctrl Pts',(3.9180646415612,-0.343911574854212,24.7034084772976));
#26098=CARTESIAN_POINT('Ctrl Pts',(3.92059512956118,-0.312126304660715,
24.705031514346));
#26099=CARTESIAN_POINT('Ctrl Pts',(3.92880900465803,-0.208952434920612,
24.7102998355523));
#26100=CARTESIAN_POINT('Ctrl Pts',(3.93295088356075,-0.105450099946497,
24.7155681567587));
#26101=CARTESIAN_POINT('Ctrl Pts',(3.93299956579126,-0.00184810329566231,
24.7208364779651));
#26102=CARTESIAN_POINT('',(3.93141232006596,-0.00268530749238849,25.9708359449846));
#26103=CARTESIAN_POINT('Ctrl Pts',(3.93846800795475,-0.0018173926281477,
24.7208381679678));
#26104=CARTESIAN_POINT('Ctrl Pts',(3.93147080551259,1.20025348547732,24.7818802628817));
#26105=CARTESIAN_POINT('Ctrl Pts',(2.69981664849856,3.72052139417293,24.90923333725));
#26106=CARTESIAN_POINT('Ctrl Pts',(-1.59375568300688,4.37084433553035,25.1028973910729));
#26107=CARTESIAN_POINT('Ctrl Pts',(-4.53899345815125,1.02072316002629,25.3018303294362));
#26108=CARTESIAN_POINT('Ctrl Pts',(-3.3115139775936,-3.26775344216146,25.5007632677998));
#26109=CARTESIAN_POINT('Ctrl Pts',(0.960255309548966,-4.5521694962993,25.6996962061631));
#26110=CARTESIAN_POINT('Ctrl Pts',(3.62962046299946,-2.2676433969507,25.8563867650922));
#26111=CARTESIAN_POINT('Ctrl Pts',(3.93139694366218,-0.479785797299594,
25.9467663445668));
#26112=CARTESIAN_POINT('Ctrl Pts',(3.92843397312147,-0.0027031107579956,
25.9708349445869));
#26113=CARTESIAN_POINT('',(3.93299899378077,0.00281334665823111,27.2208364780115));
#26114=CARTESIAN_POINT('Ctrl Pts',(3.93299908974997,-0.00267582247178204,
25.9708364779651));
#26115=CARTESIAN_POINT('Ctrl Pts',(3.93307847500203,0.114006852631101,25.9767162588663));
#26116=CARTESIAN_POINT('Ctrl Pts',(3.92796099030741,0.230722709585052,25.9825960397676));
#26117=CARTESIAN_POINT('Ctrl Pts',(3.91766444130927,0.346978854256137,25.9884758206688));
#26118=CARTESIAN_POINT('Ctrl Pts',(3.90736771657427,0.463236983134719,25.9943557019235));
#26119=CARTESIAN_POINT('Ctrl Pts',(3.89189178715577,0.579034978138806,26.0002355831782));
#26120=CARTESIAN_POINT('Ctrl Pts',(3.8713063936447,0.693884577235768,26.0061154644329));
#26121=CARTESIAN_POINT('Ctrl Pts',(3.85071584754484,0.808762923548909,26.0119968174403));
#26122=CARTESIAN_POINT('Ctrl Pts',(3.82501336480267,0.922692000596265,26.0178781704478));
#26123=CARTESIAN_POINT('Ctrl Pts',(3.79431978480095,1.03519388071417,26.0237595234553));
#26124=CARTESIAN_POINT('Ctrl Pts',(3.7622230779227,1.15283867383357,26.0299097367415));
#26125=CARTESIAN_POINT('Ctrl Pts',(3.72466825839089,1.26892221175978,26.0360599500277));
#26126=CARTESIAN_POINT('Ctrl Pts',(3.68185120842645,1.38291745198644,26.042210163314));
#26127=CARTESIAN_POINT('Ctrl Pts',(3.64083112684314,1.49212848025882,26.0481022612274));
#26128=CARTESIAN_POINT('Ctrl Pts',(3.59498179423383,1.59942259743108,26.0539943591409));
#26129=CARTESIAN_POINT('Ctrl Pts',(3.54452368503031,1.70435936535085,26.0598864570543));
#26130=CARTESIAN_POINT('Ctrl Pts',(3.49402528304427,1.8093799294024,26.0657832600395));
#26131=CARTESIAN_POINT('Ctrl Pts',(3.43891096727444,1.91203903764287,26.0716800630246));
#26132=CARTESIAN_POINT('Ctrl Pts',(3.37944587868953,2.01192309818451,26.0775768660097));
#26133=CARTESIAN_POINT('Ctrl Pts',(3.31988876348354,2.11196173669468,26.0834827947334));
#26134=CARTESIAN_POINT('Ctrl Pts',(3.25596766160649,2.20921641858616,26.0893887234571));
#26135=CARTESIAN_POINT('Ctrl Pts',(3.18798953366984,2.30330452463663,26.0952946521808));
#26136=CARTESIAN_POINT('Ctrl Pts',(3.17929004416549,2.31534543420437,26.0960504624172));
#26137=CARTESIAN_POINT('Ctrl Pts',(3.17052416165146,2.32733453073281,26.0968062726536));
#26138=CARTESIAN_POINT('Ctrl Pts',(3.16169257377295,2.33927105504022,26.09756208289));
#26139=CARTESIAN_POINT('Ctrl Pts',(3.09307723047327,2.43200961173293,26.103434206856));
#26140=CARTESIAN_POINT('Ctrl Pts',(3.02026309303068,2.52188215266156,26.1093063308221));
#26141=CARTESIAN_POINT('Ctrl Pts',(2.94351803671329,2.60848434297458,26.1151784547881));
#26142=CARTESIAN_POINT('Ctrl Pts',(2.86687248188506,2.69497425182852,26.1210429654288));
#26143=CARTESIAN_POINT('Ctrl Pts',(2.78630641495341,2.77820193549206,26.1269074760696));
#26144=CARTESIAN_POINT('Ctrl Pts',(2.70213006103127,2.85779322787202,26.1327719867103));
#26145=CARTESIAN_POINT('Ctrl Pts',(2.61804032374003,2.93730262160379,26.1386304628279));
#26146=CARTESIAN_POINT('Ctrl Pts',(2.53034798725404,3.01318278436977,26.1444889389455));
#26147=CARTESIAN_POINT('Ctrl Pts',(2.43940203736505,3.08509427734376,26.1503474150631));
#26148=CARTESIAN_POINT('Ctrl Pts',(2.34486996820184,3.15984133574213,26.1564368986544));
#26149=CARTESIAN_POINT('Ctrl Pts',(2.24682272007359,3.23029996503684,26.1625263822456));
#26150=CARTESIAN_POINT('Ctrl Pts',(2.14569287915421,3.29613274434555,26.1686158658369));
#26151=CARTESIAN_POINT('Ctrl Pts',(2.04851223718516,3.35939470241515,26.1744675503573));
#26152=CARTESIAN_POINT('Ctrl Pts',(1.94848561891036,3.41838507004291,26.1803192348777));
#26153=CARTESIAN_POINT('Ctrl Pts',(1.84602808994577,3.4728474327461,26.1861709193981));
#26154=CARTESIAN_POINT('Ctrl Pts',(1.74358618798152,3.5273014887551,26.1920217114094));
#26155=CARTESIAN_POINT('Ctrl Pts',(1.63871447747145,3.57722871901727,26.1978725034208));
#26156=CARTESIAN_POINT('Ctrl Pts',(1.53185315801943,3.62241837758505,26.2037232954321));
#26157=CARTESIAN_POINT('Ctrl Pts',(1.42498225433505,3.6676120891459,26.2095746121922));
#26158=CARTESIAN_POINT('Ctrl Pts',(1.31612176776525,3.70806722331031,26.2154259289523));
#26159=CARTESIAN_POINT('Ctrl Pts',(1.20573176459576,3.74362122975132,26.2212772457125));
#26160=CARTESIAN_POINT('Ctrl Pts',(1.09530512312868,3.77918703652054,26.227130504517));
#26161=CARTESIAN_POINT('Ctrl Pts',(0.983348348942157,3.80984835435143,26.2329837633215));
#26162=CARTESIAN_POINT('Ctrl Pts',(0.870335852415266,3.8354927328833,26.238837022126));
#26163=CARTESIAN_POINT('Ctrl Pts',(0.757194782129486,3.86116628689792,26.2446969401541));
#26164=CARTESIAN_POINT('Ctrl Pts',(0.642995995563217,3.88181141756269,26.2505568581822));
#26165=CARTESIAN_POINT('Ctrl Pts',(0.528223361667081,3.897366941948,26.2564167762103));
#26166=CARTESIAN_POINT('Ctrl Pts',(0.413373448071933,3.91293294031306,26.262280639889));
#26167=CARTESIAN_POINT('Ctrl Pts',(0.297949328490852,3.92340247136169,26.2681445035676));
#26168=CARTESIAN_POINT('Ctrl Pts',(0.182437499127316,3.92876641694466,26.2740083672462));
#26169=CARTESIAN_POINT('Ctrl Pts',(0.0667552620432346,3.93413827563701,
26.2798808815336));
#26170=CARTESIAN_POINT('Ctrl Pts',(-0.0490145312038706,3.93438951556415,
26.285753395821));
#26171=CARTESIAN_POINT('Ctrl Pts',(-0.164387793031487,3.9295630359497,26.2916259101084));
#26172=CARTESIAN_POINT('Ctrl Pts',(-0.196274489116354,3.92822910045904,
26.2932489471568));
#26173=CARTESIAN_POINT('Ctrl Pts',(-0.228130943146756,3.92650760594574,
26.2948719842051));
#26174=CARTESIAN_POINT('Ctrl Pts',(-0.259947061604304,3.92440014845113,
26.2964950212535));
#26175=CARTESIAN_POINT('Ctrl Pts',(-0.375057306247053,3.9167753984961,26.3023671452195));
#26176=CARTESIAN_POINT('Ctrl Pts',(-0.490024774287691,3.90406896245705,
26.3082392691855));
#26177=CARTESIAN_POINT('Ctrl Pts',(-0.60436449568115,3.88628776036465,26.3141113931516));
#26178=CARTESIAN_POINT('Ctrl Pts',(-0.718555973355574,3.86852961195381,
26.3199759037923));
#26179=CARTESIAN_POINT('Ctrl Pts',(-0.832120918180024,3.84570984473732,
26.325840414433));
#26180=CARTESIAN_POINT('Ctrl Pts',(-0.944576861721489,3.8178873152963,26.3317049250737));
#26181=CARTESIAN_POINT('Ctrl Pts',(-1.0569170892158,3.79009341496129,26.3375634011913));
#26182=CARTESIAN_POINT('Ctrl Pts',(-1.16815018633492,3.75730709029601,26.3434218773089));
#26183=CARTESIAN_POINT('Ctrl Pts',(-1.27780196137539,3.7196385775375,26.3492803534266));
#26184=CARTESIAN_POINT('Ctrl Pts',(-1.39177745115417,3.68048474542393,26.3553698370178));
#26185=CARTESIAN_POINT('Ctrl Pts',(-1.50404389635785,3.63605585179664,26.3614593206091));
#26186=CARTESIAN_POINT('Ctrl Pts',(-1.61408362998824,3.58653356814125,26.3675488042003));
#26187=CARTESIAN_POINT('Ctrl Pts',(-1.71982622642744,3.53894516818284,26.3734004887207));
#26188=CARTESIAN_POINT('Ctrl Pts',(-1.82351234490506,3.48665390054298,26.3792521732412));
#26189=CARTESIAN_POINT('Ctrl Pts',(-1.92470194778854,3.42987046580173,26.3851038577616));
#26190=CARTESIAN_POINT('Ctrl Pts',(-2.02587611705805,3.37309569176857,26.3909546497729));
#26191=CARTESIAN_POINT('Ctrl Pts',(-2.12455416740189,3.31183031519004,26.3968054417842));
#26192=CARTESIAN_POINT('Ctrl Pts',(-2.22032090750913,3.24633086232408,26.4026562337955));
#26193=CARTESIAN_POINT('Ctrl Pts',(-2.31609623679267,3.18082553490974,26.4085075505556));
#26194=CARTESIAN_POINT('Ctrl Pts',(-2.40895939552027,3.11108560970418,26.4143588673158));
#26195=CARTESIAN_POINT('Ctrl Pts',(-2.4985250112749,3.03741037201656,26.4202101840759));
#26196=CARTESIAN_POINT('Ctrl Pts',(-2.5881203537406,2.96371068161362,26.4260634428805));
#26197=CARTESIAN_POINT('Ctrl Pts',(-2.67441565788543,2.88607334407477,26.431916701685));
#26198=CARTESIAN_POINT('Ctrl Pts',(-2.75705995670055,2.80483678583235,26.4377699604895));
#26199=CARTESIAN_POINT('Ctrl Pts',(-2.8397982795255,2.72350780515958,26.4436298785177));
#26200=CARTESIAN_POINT('Ctrl Pts',(-2.91887701128125,2.63857172061785,26.4494897965458));
#26201=CARTESIAN_POINT('Ctrl Pts',(-2.99398321260144,2.55040261971728,26.4553497145739));
#26202=CARTESIAN_POINT('Ctrl Pts',(-3.0691399850766,2.46217415203758,26.4612135782526));
#26203=CARTESIAN_POINT('Ctrl Pts',(-3.14031864775177,2.37070865886504,26.4670774419312));
#26204=CARTESIAN_POINT('Ctrl Pts',(-3.20724865111373,2.27641057147632,26.4729413056098));
#26205=CARTESIAN_POINT('Ctrl Pts',(-3.27427739232229,2.18197337173709,26.4788138198972));
#26206=CARTESIAN_POINT('Ctrl Pts',(-3.3370447415629,2.08469558383415,26.4846863341846));
#26207=CARTESIAN_POINT('Ctrl Pts',(-3.39532522040777,1.98500771979932,26.490558848472));
#26208=CARTESIAN_POINT('Ctrl Pts',(-3.41143269528615,1.95745613138677,26.4921818855203));
#26209=CARTESIAN_POINT('Ctrl Pts',(-3.42719772057195,1.92972057326369,26.4938049225686));
#26210=CARTESIAN_POINT('Ctrl Pts',(-3.44261618523127,1.90181040095581,26.4954279596169));
#26211=CARTESIAN_POINT('Ctrl Pts',(-3.49839996166515,1.80083181154012,26.5013000835829));
#26212=CARTESIAN_POINT('Ctrl Pts',(-3.54983064592923,1.69722748276648,26.507172207549));
#26213=CARTESIAN_POINT('Ctrl Pts',(-3.59665200836169,1.59140922793222,26.513044331515));
#26214=CARTESIAN_POINT('Ctrl Pts',(-3.64341266596814,1.48572816856631,26.5189088421557));
#26215=CARTESIAN_POINT('Ctrl Pts',(-3.68557572025949,1.37783926588556,26.5247733527965));
#26216=CARTESIAN_POINT('Ctrl Pts',(-3.72292999489956,1.26818029202363,26.5306378634372));
#26217=CARTESIAN_POINT('Ctrl Pts',(-3.76024583236257,1.15863415615509,26.5364963395548));
#26218=CARTESIAN_POINT('Ctrl Pts',(-3.7927625998516,1.04732196090309,26.5423548156724));
#26219=CARTESIAN_POINT('Ctrl Pts',(-3.8203168263334,0.934702276895635,26.54821329179));
#26220=CARTESIAN_POINT('Ctrl Pts',(-3.84895755246465,0.817641849567875,
26.5543027753813));
#26221=CARTESIAN_POINT('Ctrl Pts',(-3.87223614290353,0.699169116271193,
26.5603922589725));
#26222=CARTESIAN_POINT('Ctrl Pts',(-3.89002574344495,0.579817829439167,
26.5664817425638));
#26223=CARTESIAN_POINT('Ctrl Pts',(-3.90712064624784,0.465127303193612,
26.5723334270842));
#26224=CARTESIAN_POINT('Ctrl Pts',(-3.91914714633136,0.349625999598826,
26.5781851116046));
#26225=CARTESIAN_POINT('Ctrl Pts',(-3.92604476263612,0.233798036299546,
26.584036796125));
#26226=CARTESIAN_POINT('Ctrl Pts',(-3.93294132690444,0.117987739282589,
26.5898875881363));
#26227=CARTESIAN_POINT('Ctrl Pts',(-3.93471053821578,0.00185129419202212,
26.5957383801477));
#26228=CARTESIAN_POINT('Ctrl Pts',(-3.93134390080584,-0.114123326260163,
26.601589172159));
#26229=CARTESIAN_POINT('Ctrl Pts',(-3.92797696144723,-0.230108348303019,
26.6074404889191));
#26230=CARTESIAN_POINT('Ctrl Pts',(-3.91947326968066,-0.34593110359222,
26.6132918056792));
#26231=CARTESIAN_POINT('Ctrl Pts',(-3.90587642156723,-0.461105605523471,
26.6191431224393));
#26232=CARTESIAN_POINT('Ctrl Pts',(-3.89227506067765,-0.576318333721664,
26.6249963812439));
#26233=CARTESIAN_POINT('Ctrl Pts',(-3.87357723061026,-0.690881970396768,
26.6308496400484));
#26234=CARTESIAN_POINT('Ctrl Pts',(-3.84987805328819,-0.804318329276353,
26.6367028988529));
#26235=CARTESIAN_POINT('Ctrl Pts',(-3.82615191352923,-0.917883744140712,
26.642562816881));
#26236=CARTESIAN_POINT('Ctrl Pts',(-3.79741315400567,-1.03031891645989,
26.6484227349091));
#26237=CARTESIAN_POINT('Ctrl Pts',(-3.76380745151309,-1.14115838862735,
26.6542826529373));
#26238=CARTESIAN_POINT('Ctrl Pts',(-3.7301791213393,-1.25207249218336,26.6601465166159));
#26239=CARTESIAN_POINT('Ctrl Pts',(-3.6916774599466,-1.36138836720362,26.6660103802945));
#26240=CARTESIAN_POINT('Ctrl Pts',(-3.64849658190559,-1.46865982849101,
26.6718742439732));
#26241=CARTESIAN_POINT('Ctrl Pts',(-3.60525200168754,-1.57608954097494,
26.6777467582606));
#26242=CARTESIAN_POINT('Ctrl Pts',(-3.5573145983183,-1.68146844544931,26.683619272548));
#26243=CARTESIAN_POINT('Ctrl Pts',(-3.5049247858653,-1.78437418873596,26.6894917868354));
#26244=CARTESIAN_POINT('Ctrl Pts',(-3.49044536488725,-1.81281512998656,
26.6911148238837));
#26245=CARTESIAN_POINT('Ctrl Pts',(-3.47562610224084,-1.84106732744702,
26.692737860932));
#26246=CARTESIAN_POINT('Ctrl Pts',(-3.46047264866876,-1.8691222666844,26.6943608979804));
#26247=CARTESIAN_POINT('Ctrl Pts',(-3.4056476784195,-1.9706246207001,26.7002330219464));
#26248=CARTESIAN_POINT('Ctrl Pts',(-3.34626111779163,-2.06988291325671,
26.7061051459124));
#26249=CARTESIAN_POINT('Ctrl Pts',(-3.28252103059585,-2.16645901962071,
26.7119772698785));
#26250=CARTESIAN_POINT('Ctrl Pts',(-3.2188635836887,-2.26290991314527,26.7178417805192));
#26251=CARTESIAN_POINT('Ctrl Pts',(-3.15086406056417,-2.35668519412911,
26.7237062911599));
#26252=CARTESIAN_POINT('Ctrl Pts',(-3.07877671234571,-2.44737062079239,
26.7295708018006));
#26253=CARTESIAN_POINT('Ctrl Pts',(-3.00676354129123,-2.53796273305405,
26.7354292779182));
#26254=CARTESIAN_POINT('Ctrl Pts',(-2.93067116743927,-2.62547099335779,
26.7412877540358));
#26255=CARTESIAN_POINT('Ctrl Pts',(-2.85079712008848,-2.70951006274109,
26.7471462301535));
#26256=CARTESIAN_POINT('Ctrl Pts',(-2.76777353324691,-2.79686290395104,
26.7532357137447));
#26257=CARTESIAN_POINT('Ctrl Pts',(-2.6806641552376,-2.88046695630763,26.759325197336));
#26258=CARTESIAN_POINT('Ctrl Pts',(-2.58984956229417,-2.95992706746039,
26.7654146809272));
#26259=CARTESIAN_POINT('Ctrl Pts',(-2.50258134984409,-3.03628419946566,
26.7712663654476));
#26260=CARTESIAN_POINT('Ctrl Pts',(-2.41189221550556,-3.10881466719656,
26.777118049968));
#26261=CARTESIAN_POINT('Ctrl Pts',(-2.31815683530432,-3.17720598748836,
26.7829697344884));
#26262=CARTESIAN_POINT('Ctrl Pts',(-2.22443575178617,-3.24558687661714,
26.7888205264998));
#26263=CARTESIAN_POINT('Ctrl Pts',(-2.127669680089,-3.30982962994569,26.7946713185111));
#26264=CARTESIAN_POINT('Ctrl Pts',(-2.02826463018977,-3.36966342383348,
26.8005221105224));
#26265=CARTESIAN_POINT('Ctrl Pts',(-1.9288506647999,-3.42950258412498,26.8063734272825));
#26266=CARTESIAN_POINT('Ctrl Pts',(-1.8267976049172,-3.48493178567996,26.8122247440426));
#26267=CARTESIAN_POINT('Ctrl Pts',(-1.72253793702434,-3.5357251102867,26.8180760608027));
#26268=CARTESIAN_POINT('Ctrl Pts',(-1.61824366548384,-3.58653529313157,
26.8239293196072));
#26269=CARTESIAN_POINT('Ctrl Pts',(-1.51174170111969,-3.63270635857308,
26.8297825784117));
#26270=CARTESIAN_POINT('Ctrl Pts',(-1.403485808772,-3.674059959306,26.8356358372163));
#26271=CARTESIAN_POINT('Ctrl Pts',(-1.29510675423073,-3.71546060782604,
26.8414957552444));
#26272=CARTESIAN_POINT('Ctrl Pts',(-1.18497017529506,-3.75203270448054,
26.8473556732725));
#26273=CARTESIAN_POINT('Ctrl Pts',(-1.07354644358413,-3.78364731885358,
26.8532155913006));
#26274=CARTESIAN_POINT('Ctrl Pts',(-0.96204768708606,-3.81528322025118,
26.8590794549792));
#26275=CARTESIAN_POINT('Ctrl Pts',(-0.849260453424433,-3.84195489782017,
26.8649433186578));
#26276=CARTESIAN_POINT('Ctrl Pts',(-0.735665070849243,-3.86358459251669,
26.8708071823365));
#26277=CARTESIAN_POINT('Ctrl Pts',(-0.621902107773086,-3.88524619621331,
26.8766796966238));
#26278=CARTESIAN_POINT('Ctrl Pts',(-0.50732902395214,-3.90185091282406,
26.8825522109112));
#26279=CARTESIAN_POINT('Ctrl Pts',(-0.392431112207346,-3.91337281921512,
26.8884247251986));
#26280=CARTESIAN_POINT('Ctrl Pts',(-0.360675792693863,-3.91655722712381,
26.890047762247));
#26281=CARTESIAN_POINT('Ctrl Pts',(-0.328895657422063,-3.91935369076328,
26.8916707992954));
#26282=CARTESIAN_POINT('Ctrl Pts',(-0.297100924157858,-3.92176236415015,
26.8932938363438));
#26283=CARTESIAN_POINT('Ctrl Pts',(-0.182068050828945,-3.93047690873525,
26.8991659603098));
#26284=CARTESIAN_POINT('Ctrl Pts',(-0.0664585796196782,-3.93414056691308,
26.9050380842759));
#26285=CARTESIAN_POINT('Ctrl Pts',(0.0492464061907849,-3.93269167256693,
26.9109102082419));
#26286=CARTESIAN_POINT('Ctrl Pts',(0.164801378189231,-3.93124465674108,
26.9167747188826));
#26287=CARTESIAN_POINT('Ctrl Pts',(0.280451208963498,-3.9246982752529,26.9226392295233));
#26288=CARTESIAN_POINT('Ctrl Pts',(0.395709954140458,-3.91304263102182,
26.928503740164));
#26289=CARTESIAN_POINT('Ctrl Pts',(0.510850099215764,-3.90139898033264,
26.9343622162816));
#26290=CARTESIAN_POINT('Ctrl Pts',(0.625599550294334,-3.88465656542435,
26.9402206923992));
#26291=CARTESIAN_POINT('Ctrl Pts',(0.739473297778224,-3.86285752285442,
26.9460791685168));
#26292=CARTESIAN_POINT('Ctrl Pts',(0.857837237966352,-3.84019891516022,
26.9521686521081));
#26293=CARTESIAN_POINT('Ctrl Pts',(0.975254538461258,-3.8120767023719,26.9582581356994));
#26294=CARTESIAN_POINT('Ctrl Pts',(1.09118705804687,-3.77859759756858,26.9643476192907));
#26295=CARTESIAN_POINT('Ctrl Pts',(1.20259232256616,-3.74642587784908,26.9701993038111));
#26296=CARTESIAN_POINT('Ctrl Pts',(1.31262615914816,-3.70930792204054,26.9760509883315));
#26297=CARTESIAN_POINT('Ctrl Pts',(1.42082317605036,-3.6673901486477,26.9819026728519));
#26298=CARTESIAN_POINT('Ctrl Pts',(1.52900369055571,-3.62547876862642,26.9877534648632));
#26299=CARTESIAN_POINT('Ctrl Pts',(1.63534755702998,-3.57876917592524,26.9936042568745));
#26300=CARTESIAN_POINT('Ctrl Pts',(1.73940750656672,-3.52745666537512,26.9994550488859));
#26301=CARTESIAN_POINT('Ctrl Pts',(1.84347678908511,-3.47613955268247,27.005306365646));
#26302=CARTESIAN_POINT('Ctrl Pts',(1.9452613766542,-3.42021888432176,27.0111576824061));
#26303=CARTESIAN_POINT('Ctrl Pts',(2.04433747915318,-3.35993649810969,27.0170089991663));
#26304=CARTESIAN_POINT('Ctrl Pts',(2.14344646488121,-3.29963410425235,27.0228622579708));
#26305=CARTESIAN_POINT('Ctrl Pts',(2.23984482506121,-3.23496732876364,27.0287155167753));
#26306=CARTESIAN_POINT('Ctrl Pts',(2.33313730000996,-3.16622161879143,27.0345687755799));
#26307=CARTESIAN_POINT('Ctrl Pts',(2.42653591334601,-3.09739769716502,27.040428693608));
#26308=CARTESIAN_POINT('Ctrl Pts',(2.51682125556585,-3.02448582396451,27.0462886116361));
#26309=CARTESIAN_POINT('Ctrl Pts',(2.60363067498782,-2.94781212228027,27.0521485296642));
#26310=CARTESIAN_POINT('Ctrl Pts',(2.6904985456762,-2.87108679399842,27.0580123933428));
#26311=CARTESIAN_POINT('Ctrl Pts',(2.77388553657727,-2.79059488005739,27.0638762570215));
#26312=CARTESIAN_POINT('Ctrl Pts',(2.85346667369858,-2.70669853180799,27.0697401207001));
#26313=CARTESIAN_POINT('Ctrl Pts',(2.9331652121309,-2.62267841627367,27.0756126349875));
#26314=CARTESIAN_POINT('Ctrl Pts',(3.00904642122963,-2.53524415379178,27.0814851492749));
#26315=CARTESIAN_POINT('Ctrl Pts',(3.08082626130985,-2.44479008252724,27.0873576635623));
#26316=CARTESIAN_POINT('Ctrl Pts',(3.10066467022153,-2.41979051647267,27.0889807006106));
#26317=CARTESIAN_POINT('Ctrl Pts',(3.12019005574241,-2.39456044459457,27.090603737659));
#26318=CARTESIAN_POINT('Ctrl Pts',(3.13939702632185,-2.36910854777097,27.0922267747073));
#26319=CARTESIAN_POINT('Ctrl Pts',(3.20911987562503,-2.27671611350491,27.098118529842));
#26320=CARTESIAN_POINT('Ctrl Pts',(3.27487913500775,-2.1810861430357,27.1040102849767));
#26321=CARTESIAN_POINT('Ctrl Pts',(3.33636043504248,-2.08259166604573,27.1099020401115));
#26322=CARTESIAN_POINT('Ctrl Pts',(3.39776198835946,-1.98422494515806,27.1157861531154));
#26323=CARTESIAN_POINT('Ctrl Pts',(3.45489640044684,-1.88300144883806,27.1216702661194));
#26324=CARTESIAN_POINT('Ctrl Pts',(3.50749003621119,-1.77932645848906,27.1275543791234));
#26325=CARTESIAN_POINT('Ctrl Pts',(3.5600278986247,-1.6757614111308,27.1334322522716));
#26326=CARTESIAN_POINT('Ctrl Pts',(3.60803437707639,-1.56975040247509,27.1393101254199));
#26327=CARTESIAN_POINT('Ctrl Pts',(3.65127995366219,-1.46172627395988,27.1451879985681));
#26328=CARTESIAN_POINT('Ctrl Pts',(3.69448990082282,-1.35379114501196,27.151061029019));
#26329=CARTESIAN_POINT('Ctrl Pts',(3.73294659751401,-1.24384657418048,27.1569340594698));
#26330=CARTESIAN_POINT('Ctrl Pts',(3.76646746973821,-1.13234791446968,27.1628070899207));
#26331=CARTESIAN_POINT('Ctrl Pts',(3.79996911840911,-1.02091319702189,27.1686767523054));
#26332=CARTESIAN_POINT('Ctrl Pts',(3.82854045758789,-0.907926555425226,
27.1745464146902));
#26333=CARTESIAN_POINT('Ctrl Pts',(3.85204808511485,-0.793860535587355,
27.1804160770749));
#26334=CARTESIAN_POINT('Ctrl Pts',(3.87554802275477,-0.679831829374881,
27.1862838193577));
#26335=CARTESIAN_POINT('Ctrl Pts',(3.8939874643854,-0.564724848579951,27.1921515616405));
#26336=CARTESIAN_POINT('Ctrl Pts',(3.90728379265852,-0.449023789601447,
27.1980193039234));
#26337=CARTESIAN_POINT('Ctrl Pts',(3.92058067173715,-0.333317937662134,
27.2038872892797));
#26338=CARTESIAN_POINT('Ctrl Pts',(3.92873396285781,-0.217018364804437,
27.209755274636));
#26339=CARTESIAN_POINT('Ctrl Pts',(3.93171279971712,-0.100615409061179,
27.2156232599923));
#26340=CARTESIAN_POINT('Ctrl Pts',(3.93259494949029,-0.0661439539747947,
27.2173609993165));
#26341=CARTESIAN_POINT('Ctrl Pts',(3.93302365566106,-0.0316634505085527,
27.2190987386408));
#26342=CARTESIAN_POINT('Ctrl Pts',(3.93299899378143,0.00281334573800123,
27.2208364779651));
#26343=CARTESIAN_POINT('',(3.93453844469968,0.00164832279441522,28.470836477965));
#26344=CARTESIAN_POINT('Ctrl Pts',(3.93299899378077,0.00281334665823557,
27.2208364780115));
#26345=CARTESIAN_POINT('Ctrl Pts',(3.93290389767504,0.13575568673146,27.2275371914582));
#26346=CARTESIAN_POINT('Ctrl Pts',(3.92606429430853,0.268428158309364,27.2342379049049));
#26347=CARTESIAN_POINT('Ctrl Pts',(3.91258595467795,0.400200134004008,27.2409386183516));
#26348=CARTESIAN_POINT('Ctrl Pts',(3.89903939087984,0.532639108275039,27.247673249225));
#26349=CARTESIAN_POINT('Ctrl Pts',(3.87878683003275,0.664168293236512,27.2544078800984));
#26350=CARTESIAN_POINT('Ctrl Pts',(3.85198507497447,0.794166218227581,27.2611425109719));
#26351=CARTESIAN_POINT('Ctrl Pts',(3.82501742566897,0.9249687885809,27.2679188270453));
#26352=CARTESIAN_POINT('Ctrl Pts',(3.79141935239508,1.05422093329518,27.2746951431186));
#26353=CARTESIAN_POINT('Ctrl Pts',(3.75139889804151,1.18131084299305,27.281471459192));
#26354=CARTESIAN_POINT('Ctrl Pts',(3.73232617878847,1.24187862531122,27.2847008771516));
#26355=CARTESIAN_POINT('Ctrl Pts',(3.71179548391274,1.30195563851191,27.2879302951111));
#26356=CARTESIAN_POINT('Ctrl Pts',(3.68983306351289,1.36147749280225,27.2911597130706));
#26357=CARTESIAN_POINT('Ctrl Pts',(3.64989829607238,1.46970743128063,27.2970318370366));
#26358=CARTESIAN_POINT('Ctrl Pts',(3.60513065091982,1.57636028015,27.3029039610027));
#26359=CARTESIAN_POINT('Ctrl Pts',(3.55567420649342,1.68097291390355,27.3087760849687));
#26360=CARTESIAN_POINT('Ctrl Pts',(3.50628188332928,1.78544991530014,27.3146405956094));
#26361=CARTESIAN_POINT('Ctrl Pts',(3.45221302511836,1.88789159158712,27.3205051062501));
#26362=CARTESIAN_POINT('Ctrl Pts',(3.39366080852772,1.98785193529673,27.3263696168908));
#26363=CARTESIAN_POINT('Ctrl Pts',(3.33516884158535,2.08770942080729,27.3322280930084));
#26364=CARTESIAN_POINT('Ctrl Pts',(3.27220290009074,2.18509029773616,27.338086569126));
#26365=CARTESIAN_POINT('Ctrl Pts',(3.20500308818995,2.27957105717125,27.3439450452436));
#26366=CARTESIAN_POINT('Ctrl Pts',(3.13515349869065,2.37777731810346,27.3500345288349));
#26367=CARTESIAN_POINT('Ctrl Pts',(3.06072946983643,2.47284963393061,27.3561240124261));
#26368=CARTESIAN_POINT('Ctrl Pts',(2.98205193327776,2.56434304788466,27.3622134960174));
#26369=CARTESIAN_POINT('Ctrl Pts',(2.90644681572012,2.65226357285671,27.3680651805378));
#26370=CARTESIAN_POINT('Ctrl Pts',(2.82691445693365,2.73687912545882,27.3739168650582));
#26371=CARTESIAN_POINT('Ctrl Pts',(2.74378162707361,2.81782742248941,27.3797685495786));
#26372=CARTESIAN_POINT('Ctrl Pts',(2.66066147677713,2.89876337314518,27.3856193415899));
#26373=CARTESIAN_POINT('Ctrl Pts',(2.57394224340042,2.97603289203518,27.3914701336012));
#26374=CARTESIAN_POINT('Ctrl Pts',(2.48398760243081,3.04931051074994,27.3973209256125));
#26375=CARTESIAN_POINT('Ctrl Pts',(2.39402489356355,3.12259470162508,27.4031722423727));
#26376=CARTESIAN_POINT('Ctrl Pts',(2.3008265207982,3.19188601948212,27.4090235591328));
#26377=CARTESIAN_POINT('Ctrl Pts',(2.20478871481325,3.25689971031227,27.4148748758929));
#26378=CARTESIAN_POINT('Ctrl Pts',(2.10871903400574,3.32193497910162,27.4207281346974));
#26379=CARTESIAN_POINT('Ctrl Pts',(2.00980838823359,3.38268956617475,27.426581393502));
#26380=CARTESIAN_POINT('Ctrl Pts',(1.90848079393706,3.43892280506169,27.4324346523065));
#26381=CARTESIAN_POINT('Ctrl Pts',(1.80703791973774,3.49522002022634,27.4382945703346));
#26382=CARTESIAN_POINT('Ctrl Pts',(1.70317297027915,3.54698541935836,27.4441544883627));
#26383=CARTESIAN_POINT('Ctrl Pts',(1.59733338384377,3.59402491099578,27.4500144063908));
#26384=CARTESIAN_POINT('Ctrl Pts',(1.49142253258587,3.64109607566911,27.4558782700695));
#26385=CARTESIAN_POINT('Ctrl Pts',(1.38353478079886,3.68343484603094,27.4617421337481));
#26386=CARTESIAN_POINT('Ctrl Pts',(1.27413465303661,3.72089638204711,27.4676059974267));
#26387=CARTESIAN_POINT('Ctrl Pts',(1.16457313378301,3.75841318283573,27.4734785117141));
#26388=CARTESIAN_POINT('Ctrl Pts',(1.05349518082869,3.79103827314113,27.4793510260015));
#26389=CARTESIAN_POINT('Ctrl Pts',(0.941377556897401,3.81867742750941,27.4852235402889));
#26390=CARTESIAN_POINT('Ctrl Pts',(0.910390649328914,3.82631629722186,27.4868465773373));
#26391=CARTESIAN_POINT('Ctrl Pts',(0.879324366011928,3.83357461986963,27.4884696143857));
#26392=CARTESIAN_POINT('Ctrl Pts',(0.848188843983882,3.84045110435497,27.4900926514341));
#26393=CARTESIAN_POINT('Ctrl Pts',(0.735540987129564,3.86533012322183,27.4959647754001));
#26394=CARTESIAN_POINT('Ctrl Pts',(0.621608724895579,3.8852903799034,27.5018368993662));
#26395=CARTESIAN_POINT('Ctrl Pts',(0.506859602906102,3.90020285920385,27.5077090233322));
#26396=CARTESIAN_POINT('Ctrl Pts',(0.392259255431717,3.91509600417878,27.5135735339729));
#26397=CARTESIAN_POINT('Ctrl Pts',(0.276844560493442,3.92495433370982,27.5194380446137));
#26398=CARTESIAN_POINT('Ctrl Pts',(0.161095189998294,3.92969939559751,27.5253025552544));
#26399=CARTESIAN_POINT('Ctrl Pts',(0.0454649244538145,3.93443957486372,
27.531161031372));
#26400=CARTESIAN_POINT('Ctrl Pts',(-0.070498921085112,3.93407693503176,
27.5370195074896));
#26401=CARTESIAN_POINT('Ctrl Pts',(-0.186310248779996,3.9285846676888,27.5428779836072));
#26402=CARTESIAN_POINT('Ctrl Pts',(-0.306688170533229,3.92287583296928,
27.5489674671985));
#26403=CARTESIAN_POINT('Ctrl Pts',(-0.426900847772791,3.91162445356488,
27.5550569507898));
#26404=CARTESIAN_POINT('Ctrl Pts',(-0.546400460578536,3.89486014340433,
27.561146434381));
#26405=CARTESIAN_POINT('Ctrl Pts',(-0.661233520553275,3.8787504925954,27.5669981189014));
#26406=CARTESIAN_POINT('Ctrl Pts',(-0.775407714481389,3.85755046247169,
27.5728498034218));
#26407=CARTESIAN_POINT('Ctrl Pts',(-0.888441632615616,3.83133925219828,
27.5787014879423));
#26408=CARTESIAN_POINT('Ctrl Pts',(-1.00145831062031,3.8051320397042,27.5845522799536));
#26409=CARTESIAN_POINT('Ctrl Pts',(-1.11333465601668,3.77391526011764,27.5904030719649));
#26410=CARTESIAN_POINT('Ctrl Pts',(-1.22360029485032,3.73781905908274,27.5962538639762));
#26411=CARTESIAN_POINT('Ctrl Pts',(-1.33387582324482,3.70171962063336,27.6021051807364));
#26412=CARTESIAN_POINT('Ctrl Pts',(-1.44253996497987,3.66074001939631,27.6079564974965));
#26413=CARTESIAN_POINT('Ctrl Pts',(-1.54913901377649,3.615059794249,27.6138078142567));
#26414=CARTESIAN_POINT('Ctrl Pts',(-1.65577344265825,3.56936440789458,27.6196610730612));
#26415=CARTESIAN_POINT('Ctrl Pts',(-1.76034103593322,3.51896545816114,27.6255143318657));
#26416=CARTESIAN_POINT('Ctrl Pts',(-1.86241017044761,3.46408968662956,27.6313675906703));
#26417=CARTESIAN_POINT('Ctrl Pts',(-1.9645954285115,3.40915148320413,27.6372275086984));
#26418=CARTESIAN_POINT('Ctrl Pts',(-2.0642761899507,3.34972648785435,27.6430874267265));
#26419=CARTESIAN_POINT('Ctrl Pts',(-2.16104736583126,3.28608631697857,27.6489473447546));
#26420=CARTESIAN_POINT('Ctrl Pts',(-2.25788370051402,3.22240329535443,27.6548112084333));
#26421=CARTESIAN_POINT('Ctrl Pts',(-2.35180621446453,3.1544996884199,27.6606750721119));
#26422=CARTESIAN_POINT('Ctrl Pts',(-2.4424420284316,3.08268810257394,27.6665389357906));
#26423=CARTESIAN_POINT('Ctrl Pts',(-2.53321155201563,3.01077057737337,27.672411450078));
#26424=CARTESIAN_POINT('Ctrl Pts',(-2.62068438737155,2.93493383677337,27.6782839643654));
#26425=CARTESIAN_POINT('Ctrl Pts',(-2.70452363160501,2.85552813435449,27.6841564786528));
#26426=CARTESIAN_POINT('Ctrl Pts',(-2.72769500128213,2.83358210058424,27.685779515701));
#26427=CARTESIAN_POINT('Ctrl Pts',(-2.75058905325276,2.81136364899612,27.6874025527493));
#26428=CARTESIAN_POINT('Ctrl Pts',(-2.77319922360805,2.78888061167554,27.6890255897975));
#26429=CARTESIAN_POINT('Ctrl Pts',(-2.85500248457678,2.70753731614063,27.6948977137635));
#26430=CARTESIAN_POINT('Ctrl Pts',(-2.93336091890663,2.62245542621175,27.7007698377296));
#26431=CARTESIAN_POINT('Ctrl Pts',(-3.00791333059858,2.53395864125825,27.7066419616956));
#26432=CARTESIAN_POINT('Ctrl Pts',(-3.08236908360846,2.44557659414363,27.7125064723363));
#26433=CARTESIAN_POINT('Ctrl Pts',(-3.15302836318535,2.35378876990502,27.718370982977));
#26434=CARTESIAN_POINT('Ctrl Pts',(-3.21956596674014,2.25895639307372,27.7242354936178));
#26435=CARTESIAN_POINT('Ctrl Pts',(-3.28603510376284,2.16422159781471,27.7300939697354));
#26436=CARTESIAN_POINT('Ctrl Pts',(-3.34839076462158,2.06644881766277,27.735952445853));
#26437=CARTESIAN_POINT('Ctrl Pts',(-3.40634772973127,1.96603258979973,27.7418109219706));
#26438=CARTESIAN_POINT('Ctrl Pts',(-3.46659001474695,1.86165681705737,27.7479004055619));
#26439=CARTESIAN_POINT('Ctrl Pts',(-3.52207928141067,1.75442518649659,27.7539898891531));
#26440=CARTESIAN_POINT('Ctrl Pts',(-3.57254443486776,1.644814658524,27.7600793727444));
#26441=CARTESIAN_POINT('Ctrl Pts',(-3.62103888482874,1.53948450692773,27.7659310572648));
#26442=CARTESIAN_POINT('Ctrl Pts',(-3.66489406001013,1.43195817784432,27.7717827417852));
#26443=CARTESIAN_POINT('Ctrl Pts',(-3.70391647323494,1.32268354465414,27.7776344263056));
#26444=CARTESIAN_POINT('Ctrl Pts',(-3.7429329346935,1.21342557822086,27.7834852183169));
#26445=CARTESIAN_POINT('Ctrl Pts',(-3.77711796078971,1.10242022709867,27.7893360103283));
#26446=CARTESIAN_POINT('Ctrl Pts',(-3.80632689601003,0.990133607504907,
27.7951868023396));
#26447=CARTESIAN_POINT('Ctrl Pts',(-3.83553845093623,0.877836917091518,
27.8010381190997));
#26448=CARTESIAN_POINT('Ctrl Pts',(-3.85977292370389,0.764259129887349,
27.8068894358599));
#26449=CARTESIAN_POINT('Ctrl Pts',(-3.87893622667187,0.649879026752366,
27.81274075262));
#26450=CARTESIAN_POINT('Ctrl Pts',(-3.89810588991509,0.535460961010476,
27.8185940114245));
#26451=CARTESIAN_POINT('Ctrl Pts',(-3.91220096831981,0.420240457356516,
27.8244472702291));
#26452=CARTESIAN_POINT('Ctrl Pts',(-3.92117902514,0.304703220859408,27.8303005290336));
#26453=CARTESIAN_POINT('Ctrl Pts',(-3.93016729625104,0.189034538219762,
27.8361604470617));
#26454=CARTESIAN_POINT('Ctrl Pts',(-3.93402689395027,0.0730488159131875,
27.8420203650898));
#26455=CARTESIAN_POINT('Ctrl Pts',(-3.93276747874505,-0.0427663199875365,
27.847880283118));
#26456=CARTESIAN_POINT('Ctrl Pts',(-3.93150721553953,-0.158659437533726,
27.8537441467966));
#26457=CARTESIAN_POINT('Ctrl Pts',(-3.92512109894429,-0.274381328186647,
27.8596080104752));
#26458=CARTESIAN_POINT('Ctrl Pts',(-3.91367068459627,-0.389449319593444,
27.8654718741539));
#26459=CARTESIAN_POINT('Ctrl Pts',(-3.90220337813408,-0.504687063953107,
27.8713443884413));
#26460=CARTESIAN_POINT('Ctrl Pts',(-3.88565692194286,-0.619268576150767,
27.8772169027287));
#26461=CARTESIAN_POINT('Ctrl Pts',(-3.86414398931519,-0.732721113275251,
27.8830894170161));
#26462=CARTESIAN_POINT('Ctrl Pts',(-3.85819827595229,-0.764076962229491,
27.8847124540644));
#26463=CARTESIAN_POINT('Ctrl Pts',(-3.85187349085219,-0.795346664820355,
27.8863354911127));
#26464=CARTESIAN_POINT('Ctrl Pts',(-3.84517267746582,-0.826520465850875,
27.887958528161));
#26465=CARTESIAN_POINT('Ctrl Pts',(-3.82092923402807,-0.93930681557368,
27.893830652127));
#26466=CARTESIAN_POINT('Ctrl Pts',(-3.79167857667318,-1.05121468513039,
27.899702776093));
#26467=CARTESIAN_POINT('Ctrl Pts',(-3.75749790814601,-1.16176523888363,
27.905574900059));
#26468=CARTESIAN_POINT('Ctrl Pts',(-3.72336155553428,-1.27217246164886,
27.9114394106997));
#26469=CARTESIAN_POINT('Ctrl Pts',(-3.68430802382435,-1.38122547687397,
27.9173039213404));
#26470=CARTESIAN_POINT('Ctrl Pts',(-3.64046553995892,-1.4884554586455,27.9231684319811));
#26471=CARTESIAN_POINT('Ctrl Pts',(-3.59666816957323,-1.59557510183257,
27.9290269080987));
#26472=CARTESIAN_POINT('Ctrl Pts',(-3.548091804144,-1.70087506242788,27.9348853842163));
#26473=CARTESIAN_POINT('Ctrl Pts',(-3.49491430599666,-1.80390215747415,
27.9407438603339));
#26474=CARTESIAN_POINT('Ctrl Pts',(-3.43963994865642,-1.91099174735172,
27.9468333439252));
#26475=CARTESIAN_POINT('Ctrl Pts',(-3.37939427043638,-2.01562510514671,
27.9529228275164));
#26476=CARTESIAN_POINT('Ctrl Pts',(-3.31443212027581,-2.1173163958379,27.9590123111077));
#26477=CARTESIAN_POINT('Ctrl Pts',(-3.25200679260917,-2.21503656252804,
27.9648639956281));
#26478=CARTESIAN_POINT('Ctrl Pts',(-3.18522668775894,-2.31003974896123,
27.9707156801485));
#26479=CARTESIAN_POINT('Ctrl Pts',(-3.11436411475705,-2.40192113957006,
27.9765673646689));
#26480=CARTESIAN_POINT('Ctrl Pts',(-3.04351234983792,-2.49378851626954,
27.9824181566802));
#26481=CARTESIAN_POINT('Ctrl Pts',(-2.96857960722595,-2.58253471659117,
27.9882689486915));
#26482=CARTESIAN_POINT('Ctrl Pts',(-2.88987993231758,-2.66778615649533,
27.9941197407028));
#26483=CARTESIAN_POINT('Ctrl Pts',(-2.81117319895261,-2.75304524247413,
27.9999710574629));
#26484=CARTESIAN_POINT('Ctrl Pts',(-2.72869914211331,-2.83480864116148,
28.005822374223));
#26485=CARTESIAN_POINT('Ctrl Pts',(-2.64280978799126,-2.91273847512914,
28.0116736909831));
#26486=CARTESIAN_POINT('Ctrl Pts',(-2.55689192730466,-2.99069417390698,
28.0175269497876));
#26487=CARTESIAN_POINT('Ctrl Pts',(-2.46755682138669,-3.06481350032096,
28.0233802085921));
#26488=CARTESIAN_POINT('Ctrl Pts',(-2.37519023219202,-3.13479829668507,
28.0292334673966));
#26489=CARTESIAN_POINT('Ctrl Pts',(-2.2827185579857,-3.20486271440584,28.0350933854247));
#26490=CARTESIAN_POINT('Ctrl Pts',(-2.18720884628985,-3.27078296353361,
28.0409533034528));
#26491=CARTESIAN_POINT('Ctrl Pts',(-2.08907662610493,-3.33230368517967,
28.0468132214809));
#26492=CARTESIAN_POINT('Ctrl Pts',(-1.99087833068777,-3.39386583048825,
28.0526770851595));
#26493=CARTESIAN_POINT('Ctrl Pts',(-1.89005436947373,-3.45102234635887,
28.0585409488382));
#26494=CARTESIAN_POINT('Ctrl Pts',(-1.78704414461185,-3.50356421736615,
28.0644048125168));
#26495=CARTESIAN_POINT('Ctrl Pts',(-1.68388195490171,-3.55618360026573,
28.0702773268041));
#26496=CARTESIAN_POINT('Ctrl Pts',(-1.578527439325,-3.60417458064231,28.0761498410915));
#26497=CARTESIAN_POINT('Ctrl Pts',(-1.47143926629275,-3.64737652095473,
28.0820223553789));
#26498=CARTESIAN_POINT('Ctrl Pts',(-1.44184239112471,-3.65931661105281,
28.0836453924274));
#26499=CARTESIAN_POINT('Ctrl Pts',(-1.41211317255464,-3.6708911853484,28.0852684294759));
#26500=CARTESIAN_POINT('Ctrl Pts',(-1.38226146353499,-3.68209753352978,
28.0868914665243));
#26501=CARTESIAN_POINT('Ctrl Pts',(-1.27425842310814,-3.72264193502029,
28.0927635904904));
#26502=CARTESIAN_POINT('Ctrl Pts',(-1.16428893593136,-3.75849837258234,
28.0986357144564));
#26503=CARTESIAN_POINT('Ctrl Pts',(-1.05279763066019,-3.78947307008195,
28.1045078384225));
#26504=CARTESIAN_POINT('Ctrl Pts',(-0.941450876080078,-3.82040760827121,
28.1103723490632));
#26505=CARTESIAN_POINT('Ctrl Pts',(-0.828586621764973,-3.84647288338478,
28.116236859704));
#26506=CARTESIAN_POINT('Ctrl Pts',(-0.714668644579877,-3.86752346191388,
28.1221013703447));
#26507=CARTESIAN_POINT('Ctrl Pts',(-0.600867887860008,-3.8885523796071,
28.1279598464623));
#26508=CARTESIAN_POINT('Ctrl Pts',(-0.48601596901778,-3.90457678967679,
28.1338183225799));
#26509=CARTESIAN_POINT('Ctrl Pts',(-0.370590322647342,-3.91550147653658,
28.1396767986976));
#26510=CARTESIAN_POINT('Ctrl Pts',(-0.250613290144082,-3.92685693827043,
28.1457662822888));
#26511=CARTESIAN_POINT('Ctrl Pts',(-0.130016792046849,-3.93270210330527,
28.1518557658801));
#26512=CARTESIAN_POINT('Ctrl Pts',(-0.00934733730404496,-3.93298889234197,
28.1579452494714));
#26513=CARTESIAN_POINT('Ctrl Pts',(0.106609881370335,-3.93326448204371,
28.1637969339918));
#26514=CARTESIAN_POINT('Ctrl Pts',(0.222634013232644,-3.92840766600728,
28.1696486185122));
#26515=CARTESIAN_POINT('Ctrl Pts',(0.338237287969133,-3.91842883526386,
28.1755003030326));
#26516=CARTESIAN_POINT('Ctrl Pts',(0.453822930693283,-3.90845152650905,
28.181351095044));
#26517=CARTESIAN_POINT('Ctrl Pts',(0.568987432153757,-3.89335379189814,
28.1872018870553));
#26518=CARTESIAN_POINT('Ctrl Pts',(0.683246749400239,-3.87319801706987,
28.1930526790666));
#26519=CARTESIAN_POINT('Ctrl Pts',(0.797516314394701,-3.85304043450018,
28.1989039958268));
#26520=CARTESIAN_POINT('Ctrl Pts',(0.910880126636748,-3.8278239817254,28.2047553125869));
#26521=CARTESIAN_POINT('Ctrl Pts',(1.02286366537529,-3.79766229699996,28.2106066293471));
#26522=CARTESIAN_POINT('Ctrl Pts',(1.13488437130418,-3.76749060165073,28.2164598881516));
#26523=CARTESIAN_POINT('Ctrl Pts',(1.24552349382999,-3.73237051816125,28.2223131469562));
#26524=CARTESIAN_POINT('Ctrl Pts',(1.35432170501045,-3.69246553394037,28.2281664057607));
#26525=CARTESIAN_POINT('Ctrl Pts',(1.46324369537758,-3.65251515001635,28.2340263237889));
#26526=CARTESIAN_POINT('Ctrl Pts',(1.57032020568019,-3.60776914220727,28.239886241817));
#26527=CARTESIAN_POINT('Ctrl Pts',(1.6751118361179,-3.5584391713921,28.2457461598451));
#26528=CARTESIAN_POINT('Ctrl Pts',(1.77997402575952,-3.50907598529577,28.2516100235238));
#26529=CARTESIAN_POINT('Ctrl Pts',(1.88254790713922,-3.4551228823243,28.2574738872025));
#26530=CARTESIAN_POINT('Ctrl Pts',(1.98242017598273,-3.39683665280752,28.2633377508811));
#26531=CARTESIAN_POINT('Ctrl Pts',(2.08243978043466,-3.33846443708869,28.2692102651685));
#26532=CARTESIAN_POINT('Ctrl Pts',(2.17974947178649,-3.27574655990002,28.2750827794559));
#26533=CARTESIAN_POINT('Ctrl Pts',(2.27396624245754,-3.2089821638899,28.2809552937433));
#26534=CARTESIAN_POINT('Ctrl Pts',(2.3000057379576,-3.19052991619465,28.2825783307915));
#26535=CARTESIAN_POINT('Ctrl Pts',(2.32580918463529,-3.17176880359157,28.2842013678397));
#26536=CARTESIAN_POINT('Ctrl Pts',(2.35136897790047,-3.15270565225606,28.2858244048879));
#26537=CARTESIAN_POINT('Ctrl Pts',(2.44292642898942,-3.08441974994477,28.2916382678411));
#26538=CARTESIAN_POINT('Ctrl Pts',(2.53167513435791,-3.01201639839188,28.2974521307943));
#26539=CARTESIAN_POINT('Ctrl Pts',(2.61721613342261,-2.9357569230017,28.3032659937476));
#26540=CARTESIAN_POINT('Ctrl Pts',(2.70264584827739,-2.85959665706149,28.3090722931797));
#26541=CARTESIAN_POINT('Ctrl Pts',(2.7848758397571,-2.77959051754744,28.3148785926119));
#26542=CARTESIAN_POINT('Ctrl Pts',(2.86353708680282,-2.69604234990937,28.3206848920441));
#26543=CARTESIAN_POINT('Ctrl Pts',(2.94211808810384,-2.61257941337533,28.3264852682188));
#26544=CARTESIAN_POINT('Ctrl Pts',(3.01713729567528,-2.52558193867496,28.3322856443934));
#26545=CARTESIAN_POINT('Ctrl Pts',(3.08826029700842,-2.43539264553408,28.3380860205681));
#26546=CARTESIAN_POINT('Ctrl Pts',(3.15933189784284,-2.34526853207572,28.3438822048186));
#26547=CARTESIAN_POINT('Ctrl Pts',(3.22651263113738,-2.25195751782776,28.3496783890691));
#26548=CARTESIAN_POINT('Ctrl Pts',(3.28950689367905,-2.15583705238545,28.3554745733197));
#26549=CARTESIAN_POINT('Ctrl Pts',(3.35247760017397,-2.0597525301876,28.3612685901476));
#26550=CARTESIAN_POINT('Ctrl Pts',(3.41126471568405,-1.96086099736457,28.3670626069755));
#26551=CARTESIAN_POINT('Ctrl Pts',(3.46561510510418,-1.85957009635929,28.3728566238034));
#26552=CARTESIAN_POINT('Ctrl Pts',(3.51995897317413,-1.75829134896402,28.3786499454236));
#26553=CARTESIAN_POINT('Ctrl Pts',(3.56986697404504,-1.65461417805031,28.3844432670438));
#26554=CARTESIAN_POINT('Ctrl Pts',(3.6151316267666,-1.54897137518803,28.3902365886639));
#26555=CARTESIAN_POINT('Ctrl Pts',(3.66040234371183,-1.4433144190837,28.3960306864305));
#26556=CARTESIAN_POINT('Ctrl Pts',(3.70102831075177,-1.33569169633608,28.4018247841971));
#26557=CARTESIAN_POINT('Ctrl Pts',(3.73685027231346,-1.2265557640445,28.4076188819637));
#26558=CARTESIAN_POINT('Ctrl Pts',(3.77270662462591,-1.11731505617719,28.4134185423338));
#26559=CARTESIAN_POINT('Ctrl Pts',(3.80374963117829,-1.00655864017171,28.419218202704));
#26560=CARTESIAN_POINT('Ctrl Pts',(3.82987000929517,-0.894753995186079,
28.4250178630742));
#26561=CARTESIAN_POINT('Ctrl Pts',(3.8560039587028,-0.7828912601782,28.4308205367575));
#26562=CARTESIAN_POINT('Ctrl Pts',(3.87721010983761,-0.669979626732484,
28.4366232104407));
#26563=CARTESIAN_POINT('Ctrl Pts',(3.89343070412677,-0.556494700929754,
28.442425884124));
#26564=CARTESIAN_POINT('Ctrl Pts',(3.90967540972263,-0.442841084029651,
28.4482371832646));
#26565=CARTESIAN_POINT('Ctrl Pts',(3.92091971988341,-0.328612893091065,
28.4540484824053));
#26566=CARTESIAN_POINT('Ctrl Pts',(3.92715791049324,-0.214288931236205,
28.4598597815459));
#26567=CARTESIAN_POINT('Ctrl Pts',(3.93108558787204,-0.142308501827107,
28.4635186803523));
#26568=CARTESIAN_POINT('Ctrl Pts',(3.93302979224588,-0.0702901060402026,
28.4671775791586));
#26569=CARTESIAN_POINT('Ctrl Pts',(3.93299965486354,0.0016476781387844,
28.470836477965));
#26570=CARTESIAN_POINT('',(3.93378334737471,-0.00358749909980301,29.7208364779651));
#26571=CARTESIAN_POINT('Ctrl Pts',(3.93869061149251,0.00165006228972526,
28.470836477965));
#26572=CARTESIAN_POINT('Ctrl Pts',(3.93917274253189,0.0930152245985141,
28.4754767663938));
#26573=CARTESIAN_POINT('Ctrl Pts',(3.89479594559616,1.48953671629816,28.5464280342761));
#26574=CARTESIAN_POINT('Ctrl Pts',(2.23403159274154,4.08086268149356,28.6836902816154));
#26575=CARTESIAN_POINT('Ctrl Pts',(-2.22665458802441,4.08489249897418,28.8826232199778));
#26576=CARTESIAN_POINT('Ctrl Pts',(-4.64036711535831,0.333662130402121,
29.0815561583418));
#26577=CARTESIAN_POINT('Ctrl Pts',(-2.78816912451703,-3.72430534672374,
29.280489096705));
#26578=CARTESIAN_POINT('Ctrl Pts',(1.62720537780082,-4.35850204095535,29.4794220350685));
#26579=CARTESIAN_POINT('Ctrl Pts',(3.78133859306296,-1.8700370989607,29.6262044954885));
#26580=CARTESIAN_POINT('Ctrl Pts',(3.93638707710448,-0.283307213321637,
29.706675976454));
#26581=CARTESIAN_POINT('Ctrl Pts',(3.93378334737471,-0.00358749909980301,
29.7208364779651));
#26582=CARTESIAN_POINT('',(3.92648812541355,-6.39030992054769E-5,30.9708364779651));
#26583=CARTESIAN_POINT('Ctrl Pts',(3.93378334737471,-0.00358749909980301,
29.7208364779651));
#26584=CARTESIAN_POINT('Ctrl Pts',(3.92419429788116,1.02656787890612,29.7729869559085));
#26585=CARTESIAN_POINT('Ctrl Pts',(2.98160786092303,3.38213034827263,29.8914484133063));
#26586=CARTESIAN_POINT('Ctrl Pts',(-0.995113215119353,4.54467678406942,
30.0762208501589));
#26587=CARTESIAN_POINT('Ctrl Pts',(-4.36178824789613,1.61837593378662,30.2751537885222));
#26588=CARTESIAN_POINT('Ctrl Pts',(-3.7186515778127,-2.79570524651421,30.4740867268857));
#26589=CARTESIAN_POINT('Ctrl Pts',(0.343058339789779,-4.63968192423417,
30.6730196652491));
#26590=CARTESIAN_POINT('Ctrl Pts',(3.46134686146429,-2.6242923161433,30.8386029156089));
#26591=CARTESIAN_POINT('Ctrl Pts',(3.92658248875702,-0.654225497905084,
30.9378751865142));
#26592=CARTESIAN_POINT('Ctrl Pts',(3.92648812541355,-6.39030992054769E-5,
30.9708364779651));
#26593=CARTESIAN_POINT('',(3.93354801992752,0.00360815564889333,32.2208364779651));
#26594=CARTESIAN_POINT('Ctrl Pts',(3.92648812541355,-6.39030992054769E-5,
30.9708364779651));
#26595=CARTESIAN_POINT('Ctrl Pts',(3.9263926501477,0.661805948792916,31.0041861659687));
#26596=CARTESIAN_POINT('Ctrl Pts',(3.45325931545757,2.63983545764988,31.103846833427));
#26597=CARTESIAN_POINT('Ctrl Pts',(0.315878541481514,4.6416115875405,31.2698184803395));
#26598=CARTESIAN_POINT('Ctrl Pts',(-3.73496181963207,2.77387771692204,31.4687514187028));
#26599=CARTESIAN_POINT('Ctrl Pts',(-4.35223485401481,-1.64389450940807,
31.6676843570663));
#26600=CARTESIAN_POINT('Ctrl Pts',(-0.968478663821196,-4.55042706350403,
31.8666172954298));
#26601=CARTESIAN_POINT('Ctrl Pts',(2.99302062995904,-3.36710213391904,32.0510013357293));
#26602=CARTESIAN_POINT('Ctrl Pts',(3.92403177335956,-1.01903183245315,32.1690743965744));
#26603=CARTESIAN_POINT('Ctrl Pts',(3.93354801992752,0.00360815564889333,
32.2208364779651));
#26604=CARTESIAN_POINT('',(3.93449192545046,-0.00152063529977577,33.4708364779651));
#26605=CARTESIAN_POINT('Ctrl Pts',(3.93354801992752,0.00360815564889333,
32.2208364779651));
#26606=CARTESIAN_POINT('Ctrl Pts',(3.93622277522228,0.291044142440767,32.2353853760289));
#26607=CARTESIAN_POINT('Ctrl Pts',(3.77605966658974,1.88560059886485,32.3162452535476));
#26608=CARTESIAN_POINT('Ctrl Pts',(1.60165038246052,4.36795758162834,32.4634161105198));
#26609=CARTESIAN_POINT('Ctrl Pts',(-2.80993399564309,3.7079115850692,32.6623490488836));
#26610=CARTESIAN_POINT('Ctrl Pts',(-4.63833331760885,-0.360834335010101,
32.8612819872469));
#26611=CARTESIAN_POINT('Ctrl Pts',(-2.20269180088781,-4.09786361569582,
33.0602149256104));
#26612=CARTESIAN_POINT('Ctrl Pts',(2.25789427045762,-4.06770830394701,33.2591478639738));
#26613=CARTESIAN_POINT('Ctrl Pts',(3.8987968700746,-1.47405973851723,33.3960217147587));
#26614=CARTESIAN_POINT('Ctrl Pts',(3.93922925932993,-0.0852329913937091,
33.4665845860891));
#26615=CARTESIAN_POINT('Ctrl Pts',(3.93881695897552,-0.00152230687485492,
33.4708364779651));
#26616=CARTESIAN_POINT('',(3.93299893535526,-0.0028938718737489,34.7208364779192));
#26617=CARTESIAN_POINT('Ctrl Pts',(3.93299970625754,-0.00152005857443918,
33.4708364779651));
#26618=CARTESIAN_POINT('Ctrl Pts',(3.9330438950136,0.112813933216348,33.4766524118655));
#26619=CARTESIAN_POINT('Ctrl Pts',(3.92809825171672,0.227351778088693,33.4824683457659));
#26620=CARTESIAN_POINT('Ctrl Pts',(3.91813566485521,0.341616615213035,33.4882842796663));
#26621=CARTESIAN_POINT('Ctrl Pts',(3.90818549564635,0.455739029382667,33.4940929644206));
#26622=CARTESIAN_POINT('Ctrl Pts',(3.89323084998174,0.569588695816249,33.499901649175));
#26623=CARTESIAN_POINT('Ctrl Pts',(3.87329661328719,0.682687589969195,33.5057103339293));
#26624=CARTESIAN_POINT('Ctrl Pts',(3.85338164164078,0.795677181936531,33.5115134049954));
#26625=CARTESIAN_POINT('Ctrl Pts',(3.8284967206146,0.907917031182888,33.5173164760614));
#26626=CARTESIAN_POINT('Ctrl Pts',(3.79871857100013,1.01893386357445,33.5231195471275));
#26627=CARTESIAN_POINT('Ctrl Pts',(3.76895950630716,1.12987954488512,33.5289188989847));
#26628=CARTESIAN_POINT('Ctrl Pts',(3.73431355699685,1.23960336145571,33.534718250842));
#26629=CARTESIAN_POINT('Ctrl Pts',(3.69490845196252,1.34764258303748,33.5405176026993));
#26630=CARTESIAN_POINT('Ctrl Pts',(3.65551615023596,1.45564670106085,33.5463150702604));
#26631=CARTESIAN_POINT('Ctrl Pts',(3.61136791005949,1.56196691584907,33.5521125378216));
#26632=CARTESIAN_POINT('Ctrl Pts',(3.56264098550639,1.666156717836,33.5579100053827));
#26633=CARTESIAN_POINT('Ctrl Pts',(3.51391755067153,1.77033905797193,33.5637070577416));
#26634=CARTESIAN_POINT('Ctrl Pts',(3.46061626229255,1.87239090655358,33.5695041101005));
#26635=CARTESIAN_POINT('Ctrl Pts',(3.40296173666513,1.97188752691249,33.5753011624594));
#26636=CARTESIAN_POINT('Ctrl Pts',(3.34529673573918,2.0714022248948,33.5810992680895));
#26637=CARTESIAN_POINT('Ctrl Pts',(3.28327713764424,2.16836040724858,33.5868973737197));
#26638=CARTESIAN_POINT('Ctrl Pts',(3.21717212097101,2.26236437030972,33.5926954793498));
#26639=CARTESIAN_POINT('Ctrl Pts',(3.15099797860989,2.35646663284854,33.5984996480303));
#26640=CARTESIAN_POINT('Ctrl Pts',(3.08073013102971,2.44760816254515,33.6043038167107));
#26641=CARTESIAN_POINT('Ctrl Pts',(3.0066795021211,2.53542252327395,33.6101079853911));
#26642=CARTESIAN_POINT('Ctrl Pts',(2.93258748986793,2.62328595923682,33.615915397743));
#26643=CARTESIAN_POINT('Ctrl Pts',(2.85470877348838,2.70781821477734,33.6217228100949));
#26644=CARTESIAN_POINT('Ctrl Pts',(2.77339144552847,2.78868945740996,33.6275302224468));
#26645=CARTESIAN_POINT('Ctrl Pts',(2.69194533307536,2.86968877805817,33.6333468321577));
#26646=CARTESIAN_POINT('Ctrl Pts',(2.60705004603519,2.94701522419906,33.6391634418686));
#26647=CARTESIAN_POINT('Ctrl Pts',(2.51908725535366,3.02037885039522,33.6449800515795));
#26648=CARTESIAN_POINT('Ctrl Pts',(2.45842666840782,3.07097161343802,33.6489912812865));
#26649=CARTESIAN_POINT('Ctrl Pts',(2.39630793521481,3.11968064274633,33.6530025109936));
#26650=CARTESIAN_POINT('Ctrl Pts',(2.33286372890622,3.16642319066068,33.6570137407007));
#26651=CARTESIAN_POINT('Ctrl Pts',(2.23998641407312,3.23485059469543,33.6628858646667));
#26652=CARTESIAN_POINT('Ctrl Pts',(2.14394017682272,3.2993028447297,33.6687579886327));
#26653=CARTESIAN_POINT('Ctrl Pts',(2.04510005975058,3.35947239095787,33.6746301125987));
#26654=CARTESIAN_POINT('Ctrl Pts',(1.94638809085282,3.4195639261746,33.6804946232394));
#26655=CARTESIAN_POINT('Ctrl Pts',(1.8448897954779,3.47538358673165,33.6863591338801));
#26656=CARTESIAN_POINT('Ctrl Pts',(1.74101180716422,3.52666512264983,33.6922236445208));
#26657=CARTESIAN_POINT('Ctrl Pts',(1.63724070826689,3.57789389037783,33.6980821206385));
#26658=CARTESIAN_POINT('Ctrl Pts',(1.53109515544159,3.62459363979002,33.7039405967561));
#26659=CARTESIAN_POINT('Ctrl Pts',(1.42300860101261,3.66654272052626,33.7097990728737));
#26660=CARTESIAN_POINT('Ctrl Pts',(1.31066005056724,3.71014590908317,33.7158885564649));
#26661=CARTESIAN_POINT('Ctrl Pts',(1.19621466552446,3.74861583435007,33.7219780400562));
#26662=CARTESIAN_POINT('Ctrl Pts',(1.08018519929194,3.78175738714564,33.7280675236475));
#26663=CARTESIAN_POINT('Ctrl Pts',(0.968686773967879,3.8136047365258,33.7339192081679));
#26664=CARTESIAN_POINT('Ctrl Pts',(0.855726099958207,3.840531933996,33.7397708926883));
#26665=CARTESIAN_POINT('Ctrl Pts',(0.741775337649826,3.86241612833916,33.7456225772087));
#26666=CARTESIAN_POINT('Ctrl Pts',(0.627841955309791,3.88429698486697,33.75147336922));
#26667=CARTESIAN_POINT('Ctrl Pts',(0.512919190807531,3.90113628966456,33.7573241612313));
#26668=CARTESIAN_POINT('Ctrl Pts',(0.397489779361355,3.91286223566627,33.7631749532426));
#26669=CARTESIAN_POINT('Ctrl Pts',(0.282050015223007,3.92458923335063,33.7690262700028));
#26670=CARTESIAN_POINT('Ctrl Pts',(0.166103925129751,3.93120191878137,33.7748775867629));
#26671=CARTESIAN_POINT('Ctrl Pts',(0.0501390412784461,3.93268039338816,
33.780728903523));
#26672=CARTESIAN_POINT('Ctrl Pts',(-0.0658643311663984,3.93415935869875,
33.7865821623276));
#26673=CARTESIAN_POINT('Ctrl Pts',(-0.181886096611841,3.93050071954973,
33.7924354211321));
#26674=CARTESIAN_POINT('Ctrl Pts',(-0.297439764363639,3.92173667991303,
33.7982886799366));
#26675=CARTESIAN_POINT('Ctrl Pts',(-0.413124896951639,3.91296266947179,
33.8041485979647));
#26676=CARTESIAN_POINT('Ctrl Pts',(-0.528340456410724,3.89907169643622,
33.8100085159929));
#26677=CARTESIAN_POINT('Ctrl Pts',(-0.642606006254656,3.88014774470321,
33.815868434021));
#26678=CARTESIAN_POINT('Ctrl Pts',(-0.756948494363085,3.86121105093198,
33.8217322976996));
#26679=CARTESIAN_POINT('Ctrl Pts',(-0.870339295668422,3.83723471591854,
33.8275961613782));
#26680=CARTESIAN_POINT('Ctrl Pts',(-0.982310791191115,3.80835325429633,
33.8334600250568));
#26681=CARTESIAN_POINT('Ctrl Pts',(-1.09444747159112,3.77942918557424,33.8393325393442));
#26682=CARTESIAN_POINT('Ctrl Pts',(-1.20516027346493,3.74558566845188,33.8452050536316));
#26683=CARTESIAN_POINT('Ctrl Pts',(-1.31399919406462,3.7070062203883,33.851077567919));
#26684=CARTESIAN_POINT('Ctrl Pts',(-1.34407993832424,3.69634368804707,33.8527006049674));
#26685=CARTESIAN_POINT('Ctrl Pts',(-1.37401768016128,3.68531967695817,33.8543236420158));
#26686=CARTESIAN_POINT('Ctrl Pts',(-1.40380324329395,3.67393868404433,33.8559466790642));
#26687=CARTESIAN_POINT('Ctrl Pts',(-1.51156696888908,3.63276242050001,33.8618188030302));
#26688=CARTESIAN_POINT('Ctrl Pts',(-1.61769815373918,3.5867717276717,33.8676909269962));
#26689=CARTESIAN_POINT('Ctrl Pts',(-1.72173535916121,3.53611599824073,33.8735630509623));
#26690=CARTESIAN_POINT('Ctrl Pts',(-1.82563767828081,3.4855259449687,33.879427561603));
#26691=CARTESIAN_POINT('Ctrl Pts',(-1.92745104863631,3.43028306229867,33.8852920722437));
#26692=CARTESIAN_POINT('Ctrl Pts',(-2.02673171285118,3.37058564111985,33.8911565828845));
#26693=CARTESIAN_POINT('Ctrl Pts',(-2.12591021824992,3.31094964799374,33.8970150590021));
#26694=CARTESIAN_POINT('Ctrl Pts',(-2.22256084906142,3.24686844526265,33.9028735351197));
#26695=CARTESIAN_POINT('Ctrl Pts',(-2.31626288442334,3.17858698956673,33.9087320112373));
#26696=CARTESIAN_POINT('Ctrl Pts',(-2.41365971516066,3.10761310562465,33.9148214948285));
#26697=CARTESIAN_POINT('Ctrl Pts',(-2.50787022334738,3.03210111018802,33.9209109784198));
#26698=CARTESIAN_POINT('Ctrl Pts',(-2.59845317081807,2.95237702861025,33.9270004620111));
#26699=CARTESIAN_POINT('Ctrl Pts',(-2.6854987837315,2.87576623443023,33.9328521465315));
#26700=CARTESIAN_POINT('Ctrl Pts',(-2.76919449786096,2.79526645012768,33.9387038310519));
#26701=CARTESIAN_POINT('Ctrl Pts',(-2.84918181026032,2.71120858881823,33.9445555155723));
#26702=CARTESIAN_POINT('Ctrl Pts',(-2.92915692285575,2.6271635481599,33.9504063075836));
#26703=CARTESIAN_POINT('Ctrl Pts',(-3.0054244734278,2.53956180892644,33.9562570995949));
#26704=CARTESIAN_POINT('Ctrl Pts',(-3.07766319562749,2.44877076393034,33.9621078916063));
#26705=CARTESIAN_POINT('Ctrl Pts',(-3.14990839681041,2.35797157602085,33.9679592083664));
#26706=CARTESIAN_POINT('Ctrl Pts',(-3.21812379389611,2.26398283724358,33.9738105251265));
#26707=CARTESIAN_POINT('Ctrl Pts',(-3.28202920647759,2.16720402542725,33.9796618418866));
#26708=CARTESIAN_POINT('Ctrl Pts',(-3.34595582918186,2.07039309284995,33.9855151006911));
#26709=CARTESIAN_POINT('Ctrl Pts',(-3.40556939528662,1.97079059070432,33.9913683594956));
#26710=CARTESIAN_POINT('Ctrl Pts',(-3.46063412841611,1.86882327394585,33.9972216183001));
#26711=CARTESIAN_POINT('Ctrl Pts',(-3.51576150842041,1.76673994947491,34.0030815363283));
#26712=CARTESIAN_POINT('Ctrl Pts',(-3.56632952936131,1.66228680432588,34.0089414543564));
#26713=CARTESIAN_POINT('Ctrl Pts',(-3.61214925603459,1.55591347835564,34.0148013723845));
#26714=CARTESIAN_POINT('Ctrl Pts',(-3.65799983444114,1.44946852818077,34.0206652360631));
#26715=CARTESIAN_POINT('Ctrl Pts',(-3.69909560617159,1.34110120834975,34.0265290997418));
#26716=CARTESIAN_POINT('Ctrl Pts',(-3.73529708060709,1.23127767770236,34.0323929634204));
#26717=CARTESIAN_POINT('Ctrl Pts',(-3.7715519609212,1.12129213094271,34.0382654777078));
#26718=CARTESIAN_POINT('Ctrl Pts',(-3.80289802211455,1.00984648231674,34.0441379919952));
#26719=CARTESIAN_POINT('Ctrl Pts',(-3.82924652548556,0.897418546196115,
34.0500105062826));
#26720=CARTESIAN_POINT('Ctrl Pts',(-3.83652868693235,0.866345874992341,
34.0516335433309));
#26721=CARTESIAN_POINT('Ctrl Pts',(-3.84342941401099,0.835198207784189,
34.0532565803793));
#26722=CARTESIAN_POINT('Ctrl Pts',(-3.84994753223726,0.803985695780863,
34.0548796174276));
#26723=CARTESIAN_POINT('Ctrl Pts',(-3.87352998729532,0.691059290334441,
34.0607517413936));
#26724=CARTESIAN_POINT('Ctrl Pts',(-3.89217924055118,0.576905106979158,
34.0666238653597));
#26725=CARTESIAN_POINT('Ctrl Pts',(-3.90577165990679,0.461992143514322,
34.0724959893257));
#26726=CARTESIAN_POINT('Ctrl Pts',(-3.91934645642081,0.347228166988323,
34.0783604999664));
#26727=CARTESIAN_POINT('Ctrl Pts',(-3.92787740899491,0.23170777347713,34.0842250106071));
#26728=CARTESIAN_POINT('Ctrl Pts',(-3.93129158458168,0.115911505025303,
34.0900895212478));
#26729=CARTESIAN_POINT('Ctrl Pts',(-3.93470224701574,0.000234389781788094,
34.0959479973655));
#26730=CARTESIAN_POINT('Ctrl Pts',(-3.93300659291112,-0.1157176250214,34.1018064734831));
#26731=CARTESIAN_POINT('Ctrl Pts',(-3.92618340346277,-0.231458165493218,
34.1076649496007));
#26732=CARTESIAN_POINT('Ctrl Pts',(-3.91909116661625,-0.351762508789647,
34.1137544331919));
#26733=CARTESIAN_POINT('Ctrl Pts',(-3.90645865083155,-0.471837905322594,
34.1198439167832));
#26734=CARTESIAN_POINT('Ctrl Pts',(-3.88832176543053,-0.591136911788797,
34.1259334003745));
#26735=CARTESIAN_POINT('Ctrl Pts',(-3.87089313951194,-0.705777199257459,
34.1317850848949));
#26736=CARTESIAN_POINT('Ctrl Pts',(-3.84838204447286,-0.8197001488176,34.1376367694153));
#26737=CARTESIAN_POINT('Ctrl Pts',(-3.82087320819095,-0.932425292947679,
34.1434884539357));
#26738=CARTESIAN_POINT('Ctrl Pts',(-3.79336856760453,-1.04513324404301,
34.149339245947));
#26739=CARTESIAN_POINT('Ctrl Pts',(-3.760867799379,-1.15664335144015,34.1551900379583));
#26740=CARTESIAN_POINT('Ctrl Pts',(-3.72350644764521,-1.26648676832589,
34.1610408299696));
#26741=CARTESIAN_POINT('Ctrl Pts',(-3.68614174502749,-1.37634003690392,
34.1668921467298));
#26742=CARTESIAN_POINT('Ctrl Pts',(-3.64391572542909,-1.48452592639684,
34.1727434634899));
#26743=CARTESIAN_POINT('Ctrl Pts',(-3.59701313135075,-1.59059282435521,
34.17859478025));
#26744=CARTESIAN_POINT('Ctrl Pts',(-3.55009497036268,-1.6966949257785,34.1844480390545));
#26745=CARTESIAN_POINT('Ctrl Pts',(-3.49849731565263,-1.80067625932397,
34.1903012978591));
#26746=CARTESIAN_POINT('Ctrl Pts',(-3.44245185545404,-1.90210783681711,
34.1961545566636));
#26747=CARTESIAN_POINT('Ctrl Pts',(-3.3863426326125,-2.00365481251442,34.2020144746917));
#26748=CARTESIAN_POINT('Ctrl Pts',(-3.32577570422196,-2.10264588008473,
34.2078743927198));
#26749=CARTESIAN_POINT('Ctrl Pts',(-3.26102732534971,-2.19867909966928,
34.213734310748));
#26750=CARTESIAN_POINT('Ctrl Pts',(-3.19623534954079,-2.29477698116916,
34.2195981744266));
#26751=CARTESIAN_POINT('Ctrl Pts',(-3.12725656250775,-2.38791271760243,
34.2254620381052));
#26752=CARTESIAN_POINT('Ctrl Pts',(-3.05440783635046,-2.47771704785694,
34.2313259017839));
#26753=CARTESIAN_POINT('Ctrl Pts',(-2.98145164080723,-2.56765386109003,
34.2371984160713));
#26754=CARTESIAN_POINT('Ctrl Pts',(-2.90461438521196,-2.65424915139292,
34.2430709303587));
#26755=CARTESIAN_POINT('Ctrl Pts',(-2.82425017279994,-2.73717006439854,
34.2489434446461));
#26756=CARTESIAN_POINT('Ctrl Pts',(-2.80203922741655,-2.76008762701293,
34.2505664816944));
#26757=CARTESIAN_POINT('Ctrl Pts',(-2.77955907006268,-2.78272475872175,
34.2521895187427));
#26758=CARTESIAN_POINT('Ctrl Pts',(-2.75681760776031,-2.80507498608197,
34.253812555791));
#26759=CARTESIAN_POINT('Ctrl Pts',(-2.67453933447679,-2.885937777148,34.259684679757));
#26760=CARTESIAN_POINT('Ctrl Pts',(-2.58856231310679,-2.9633129929522,34.265556803723));
#26761=CARTESIAN_POINT('Ctrl Pts',(-2.49921437368522,-3.03684318237956,
34.271428927689));
#26762=CARTESIAN_POINT('Ctrl Pts',(-2.4099822756412,-3.11027803845631,34.2772934383297));
#26763=CARTESIAN_POINT('Ctrl Pts',(-2.3173882670729,-3.1798775215431,34.2831579489704));
#26764=CARTESIAN_POINT('Ctrl Pts',(-2.22179728694304,-3.24532060291931,
34.2890224596111));
#26765=CARTESIAN_POINT('Ctrl Pts',(-2.12630466898078,-3.31069634401582,
34.2948809357287));
#26766=CARTESIAN_POINT('Ctrl Pts',(-2.02782155246302,-3.37192395821575,
34.3007394118463));
#26767=CARTESIAN_POINT('Ctrl Pts',(-1.92674572718564,-3.4287227800993,34.3065978879639));
#26768=CARTESIAN_POINT('Ctrl Pts',(-1.82168434822858,-3.48776125476767,
34.3126873715551));
#26769=CARTESIAN_POINT('Ctrl Pts',(-1.71382193748083,-3.54201419621172,
34.3187768551464));
#26770=CARTESIAN_POINT('Ctrl Pts',(-1.60363854014919,-3.5912160102879,34.3248663387377));
#26771=CARTESIAN_POINT('Ctrl Pts',(-1.49775789018835,-3.6384964552533,34.3307180232581));
#26772=CARTESIAN_POINT('Ctrl Pts',(-1.38973453766546,-3.68111268626925,
34.3365697077785));
#26773=CARTESIAN_POINT('Ctrl Pts',(-1.2800185505601,-3.71887637737826,34.3424213922989));
#26774=CARTESIAN_POINT('Ctrl Pts',(-1.17031929752784,-3.75663430870344,
34.3482721843101));
#26775=CARTESIAN_POINT('Ctrl Pts',(-1.05892831402063,-3.78954103719723,
34.3541229763214));
#26776=CARTESIAN_POINT('Ctrl Pts',(-0.946313348315403,-3.8174572750458,
34.3599737683327));
#26777=CARTESIAN_POINT('Ctrl Pts',(-0.833688282341747,-3.84537601666013,
34.3658250850928));
#26778=CARTESIAN_POINT('Ctrl Pts',(-0.719839417234603,-3.86830327838563,
34.371676401853));
#26779=CARTESIAN_POINT('Ctrl Pts',(-0.60524658378432,-3.88615048252347,
34.3775277186131));
#26780=CARTESIAN_POINT('Ctrl Pts',(-0.490615717121421,-3.90400361012519,
34.3833809774176));
#26781=CARTESIAN_POINT('Ctrl Pts',(-0.375240799399043,-3.91677326392377,
34.3892342362222));
#26782=CARTESIAN_POINT('Ctrl Pts',(-0.259607991416861,-3.9244225932986,
34.3950874950267));
#26783=CARTESIAN_POINT('Ctrl Pts',(-0.143843628561474,-3.93208062527759,
34.4009474130548));
#26784=CARTESIAN_POINT('Ctrl Pts',(-0.0278212025839399,-3.93460667824842,
34.4068073310829));
#26785=CARTESIAN_POINT('Ctrl Pts',(0.0879718037122605,-3.93201601748411,
34.412667249111));
#26786=CARTESIAN_POINT('Ctrl Pts',(0.203842776753245,-3.92942361235377,
34.4185311127896));
#26787=CARTESIAN_POINT('Ctrl Pts',(0.319483611034425,-3.9217076608176,34.4243949764682));
#26788=CARTESIAN_POINT('Ctrl Pts',(0.434412373694578,-3.90893526290485,
34.4302588401468));
#26789=CARTESIAN_POINT('Ctrl Pts',(0.549510683911981,-3.89614402263432,
34.4361313544342));
#26790=CARTESIAN_POINT('Ctrl Pts',(0.663894419018809,-3.87828151180982,
34.4420038687216));
#26791=CARTESIAN_POINT('Ctrl Pts',(0.777092162551848,-3.85546583059693,
34.447876383009));
#26792=CARTESIAN_POINT('Ctrl Pts',(0.80837759202277,-3.84916006545411,34.4494994200575));
#26793=CARTESIAN_POINT('Ctrl Pts',(0.839572523282062,-3.84247624389803,
34.4511224571059));
#26794=CARTESIAN_POINT('Ctrl Pts',(0.870667236762643,-3.83541752131735,
34.4527454941544));
#26795=CARTESIAN_POINT('Ctrl Pts',(0.983167448893481,-3.80987916772566,
34.4586176181204));
#26796=CARTESIAN_POINT('Ctrl Pts',(1.09473167951738,-3.77934402944444,34.4644897420864));
#26797=CARTESIAN_POINT('Ctrl Pts',(1.20488201210318,-3.74389480847288,34.4703618660525));
#26798=CARTESIAN_POINT('Ctrl Pts',(1.31488953259553,-3.70849154812023,34.4762263766932));
#26799=CARTESIAN_POINT('Ctrl Pts',(1.42348641061621,-3.66818700057308,34.4820908873339));
#26800=CARTESIAN_POINT('Ctrl Pts',(1.53020532523458,-3.62311477359243,34.4879553979747));
#26801=CARTESIAN_POINT('Ctrl Pts',(1.63681442715162,-3.5780889254849,34.4938138740923));
#26802=CARTESIAN_POINT('Ctrl Pts',(1.7415490307667,-3.5283053158788,34.4996723502099));
#26803=CARTESIAN_POINT('Ctrl Pts',(1.84395802764502,-3.47394700481793,34.5055308263276));
#26804=CARTESIAN_POINT('Ctrl Pts',(1.95040514692448,-3.41744527354718,34.5116203099188));
#26805=CARTESIAN_POINT('Ctrl Pts',(2.05433904962835,-3.3560007849713,34.5177097935101));
#26806=CARTESIAN_POINT('Ctrl Pts',(2.15527686239892,-3.28987395600619,34.5237992771013));
#26807=CARTESIAN_POINT('Ctrl Pts',(2.25227297506802,-3.22632943114782,34.5296509616218));
#26808=CARTESIAN_POINT('Ctrl Pts',(2.3465022275652,-3.15846164931986,34.5355026461422));
#26809=CARTESIAN_POINT('Ctrl Pts',(2.43756296134221,-3.08654755503501,34.5413543306626));
#26810=CARTESIAN_POINT('Ctrl Pts',(2.52860980637792,-3.01464442921273,34.547205122674));
#26811=CARTESIAN_POINT('Ctrl Pts',(2.61648876923229,-2.93869647417318,34.5530559146853));
#26812=CARTESIAN_POINT('Ctrl Pts',(2.70082990059299,-2.85902200902037,34.5589067066966));
#26813=CARTESIAN_POINT('Ctrl Pts',(2.78517859638419,-2.7793403979834,34.5647580234568));
#26814=CARTESIAN_POINT('Ctrl Pts',(2.86598852937225,-2.69593189633577,34.570609340217));
#26815=CARTESIAN_POINT('Ctrl Pts',(2.9429258910973,-2.60915239100923,34.5764606569771));
#26816=CARTESIAN_POINT('Ctrl Pts',(3.01988878823249,-2.5223440836779,34.5823139157817));
#26817=CARTESIAN_POINT('Ctrl Pts',(3.09297628425374,-2.4321628571224,34.5881671745863));
#26818=CARTESIAN_POINT('Ctrl Pts',(3.16189467562143,-2.33899787521854,34.5940204333908));
#26819=CARTESIAN_POINT('Ctrl Pts',(3.23089147510185,-2.24572689997592,34.599880351419));
#26820=CARTESIAN_POINT('Ctrl Pts',(3.29570945667985,-2.14946572640307,34.6057402694471));
#26821=CARTESIAN_POINT('Ctrl Pts',(3.35609805496617,-2.05063279147007,34.6116001874753));
#26822=CARTESIAN_POINT('Ctrl Pts',(3.41652731462377,-1.9517333094938,34.6174640511539));
#26823=CARTESIAN_POINT('Ctrl Pts',(3.47252105314246,-1.85025897920198,34.6233279148325));
#26824=CARTESIAN_POINT('Ctrl Pts',(3.52387531996301,-1.7466515764043,34.6291917785112));
#26825=CARTESIAN_POINT('Ctrl Pts',(3.57530534667407,-1.64289132777746,34.6350642927986));
#26826=CARTESIAN_POINT('Ctrl Pts',(3.62208207524941,-1.53699210297488,34.640936807086));
#26827=CARTESIAN_POINT('Ctrl Pts',(3.66405015128883,-1.42941438667739,34.6468093213734));
#26828=CARTESIAN_POINT('Ctrl Pts',(3.67564922775244,-1.3996822122517,34.6484323584216));
#26829=CARTESIAN_POINT('Ctrl Pts',(3.68688129123842,-1.36982190487914,34.6500553954697));
#26830=CARTESIAN_POINT('Ctrl Pts',(3.6977437448767,-1.33984334801695,34.6516784325179));
#26831=CARTESIAN_POINT('Ctrl Pts',(3.74330859657717,-1.21409197147652,34.6584866035691));
#26832=CARTESIAN_POINT('Ctrl Pts',(3.78249192574234,-1.08591200323833,34.6652947746203));
#26833=CARTESIAN_POINT('Ctrl Pts',(3.81506507350435,-0.955911860438615,
34.6721029456715));
#26834=CARTESIAN_POINT('Ctrl Pts',(3.84749838015831,-0.826469826549651,
34.6788818882861));
#26835=CARTESIAN_POINT('Ctrl Pts',(3.873378040257,-0.695223338518079,34.6856608309007));
#26836=CARTESIAN_POINT('Ctrl Pts',(3.89252502226064,-0.562794768165829,
34.6924397735153));
#26837=CARTESIAN_POINT('Ctrl Pts',(3.91152246576056,-0.431400468919896,
34.6991657723848));
#26838=CARTESIAN_POINT('Ctrl Pts',(3.92389189775187,-0.298842620994969,
34.7058917712543));
#26839=CARTESIAN_POINT('Ctrl Pts',(3.92950587279998,-0.165748591639581,
34.7126177701238));
#26840=CARTESIAN_POINT('Ctrl Pts',(3.9317925032017,-0.111538009796322,34.7153573393889));
#26841=CARTESIAN_POINT('Ctrl Pts',(3.9329589488365,-0.0572386882909903,
34.718096908654));
#26842=CARTESIAN_POINT('Ctrl Pts',(3.93299893535526,-0.00289387187375899,
34.7208364779192));
#26843=CARTESIAN_POINT('',(3.93133412486678,0.00259602383233126,35.9708370172092));
#26844=CARTESIAN_POINT('Ctrl Pts',(3.93299893535593,-0.00289387096241059,
34.7208364779651));
#26845=CARTESIAN_POINT('Ctrl Pts',(3.93308449943932,0.113394468515101,34.7266986738786));
#26846=CARTESIAN_POINT('Ctrl Pts',(3.92800824320406,0.229730550276868,34.7325608697921));
#26847=CARTESIAN_POINT('Ctrl Pts',(3.91778417834047,0.345624264115084,34.7384230657055));
#26848=CARTESIAN_POINT('Ctrl Pts',(3.90756092742359,0.461508751553829,34.7442847949245));
#26849=CARTESIAN_POINT('Ctrl Pts',(3.89219071857662,0.576950531920689,34.7501465241435));
#26850=CARTESIAN_POINT('Ctrl Pts',(3.8717395335229,0.691463653821281,34.7560082533624));
#26851=CARTESIAN_POINT('Ctrl Pts',(3.85128510293533,0.805994948566741,34.761870912818));
#26852=CARTESIAN_POINT('Ctrl Pts',(3.825748164523,0.919596887314197,34.7677335722735));
#26853=CARTESIAN_POINT('Ctrl Pts',(3.79524588350174,1.03179343076175,34.7735962317291));
#26854=CARTESIAN_POINT('Ctrl Pts',(3.76473149296649,1.14403451663584,34.7794612186813));
#26855=CARTESIAN_POINT('Ctrl Pts',(3.72924794657055,1.25486870131012,34.7853262056335));
#26856=CARTESIAN_POINT('Ctrl Pts',(3.68896215429787,1.36383548280502,34.7911911925857));
#26857=CARTESIAN_POINT('Ctrl Pts',(3.64862612139279,1.47293815737053,34.7970634937953));
#26858=CARTESIAN_POINT('Ctrl Pts',(3.60347602983005,1.58016839428293,34.8029357950049));
#26859=CARTESIAN_POINT('Ctrl Pts',(3.55372687053111,1.68508585231292,34.8088080962145));
#26860=CARTESIAN_POINT('Ctrl Pts',(3.5039418090126,1.7900790255845,34.8146846352574));
#26861=CARTESIAN_POINT('Ctrl Pts',(3.4495512622404,1.89275573424209,34.8205611743004));
#26862=CARTESIAN_POINT('Ctrl Pts',(3.39081520360784,1.99270199853916,34.8264377133433));
#26863=CARTESIAN_POINT('Ctrl Pts',(3.33198561160341,2.0928074207934,34.8323236103943));
#26864=CARTESIAN_POINT('Ctrl Pts',(3.26879691658386,2.1901733754738,34.8382095074454));
#26865=CARTESIAN_POINT('Ctrl Pts',(3.20155135893729,2.28441631409137,34.8440954044964));
#26866=CARTESIAN_POINT('Ctrl Pts',(3.17673668813112,2.31919344405276,34.8462673932914));
#26867=CARTESIAN_POINT('Ctrl Pts',(3.15136996528233,2.35354564591212,34.8484393820864));
#26868=CARTESIAN_POINT('Ctrl Pts',(3.12546767104165,2.3874548869609,34.8506113708814));
#26869=CARTESIAN_POINT('Ctrl Pts',(3.05543900278248,2.47913089721161,34.8564834948474));
#26870=CARTESIAN_POINT('Ctrl Pts',(2.98125596041048,2.56787687429776,34.8623556188135));
#26871=CARTESIAN_POINT('Ctrl Pts',(2.90319258488516,2.65329263653066,34.8682277427795));
#26872=CARTESIAN_POINT('Ctrl Pts',(2.82523042007632,2.73859765553172,34.8740922534202));
#26873=CARTESIAN_POINT('Ctrl Pts',(2.74339820312646,2.82058074365277,34.8799567640609));
#26874=CARTESIAN_POINT('Ctrl Pts',(2.65801185747507,2.89887253350711,34.8858212747017));
#26875=CARTESIAN_POINT('Ctrl Pts',(2.57271337352382,2.97708376188864,34.8916797508193));
#26876=CARTESIAN_POINT('Ctrl Pts',(2.48386833801903,3.05161096930942,34.8975382269369));
#26877=CARTESIAN_POINT('Ctrl Pts',(2.39183089826845,3.1221201056475,34.9033967030545));
#26878=CARTESIAN_POINT('Ctrl Pts',(2.29616430035269,3.19540951063011,34.9094861866458));
#26879=CARTESIAN_POINT('Ctrl Pts',(2.19704866423798,3.26435711381674,34.915575670237));
#26880=CARTESIAN_POINT('Ctrl Pts',(2.09492169686575,3.32863216411804,34.9216651538283));
#26881=CARTESIAN_POINT('Ctrl Pts',(1.99678286700722,3.39039722370975,34.9275168383487));
#26882=CARTESIAN_POINT('Ctrl Pts',(1.89586386492034,3.44784757492006,34.9333685228691));
#26883=CARTESIAN_POINT('Ctrl Pts',(1.79258363747825,3.50073319501005,34.9392202073895));
#26884=CARTESIAN_POINT('Ctrl Pts',(1.68931916251607,3.55361074889328,34.9450709994008));
#26885=CARTESIAN_POINT('Ctrl Pts',(1.58369454614019,3.60192476758779,34.9509217914122));
#26886=CARTESIAN_POINT('Ctrl Pts',(1.47615316630719,3.6454712767489,34.9567725834235));
#26887=CARTESIAN_POINT('Ctrl Pts',(1.36860214124798,3.68902169153158,34.9626239001836));
#26888=CARTESIAN_POINT('Ctrl Pts',(1.25913439419929,3.72780359159629,34.9684752169438));
#26889=CARTESIAN_POINT('Ctrl Pts',(1.1482124287817,3.76166149705037,34.9743265337039));
#26890=CARTESIAN_POINT('Ctrl Pts',(1.03725364850827,3.79553063989916,34.9801797925084));
#26891=CARTESIAN_POINT('Ctrl Pts',(0.924840085335178,3.824472417874,34.986033051313));
#26892=CARTESIAN_POINT('Ctrl Pts',(0.811447817419639,3.84838166501257,34.9918863101175));
#26893=CARTESIAN_POINT('Ctrl Pts',(0.697926543682018,3.87231811358329,34.9977462281457));
#26894=CARTESIAN_POINT('Ctrl Pts',(0.583424747509723,3.89121051805523,35.0036061461738));
#26895=CARTESIAN_POINT('Ctrl Pts',(0.468427178755177,3.90500511884472,35.0094660642019));
#26896=CARTESIAN_POINT('Ctrl Pts',(0.353352178846265,3.91880900793374,35.0153299278806));
#26897=CARTESIAN_POINT('Ctrl Pts',(0.237781152898853,3.92750822761217,35.0211937915592));
#26898=CARTESIAN_POINT('Ctrl Pts',(0.1222006797235,3.93110111722849,35.0270576552379));
#26899=CARTESIAN_POINT('Ctrl Pts',(0.00644969756160697,3.93469930722082,
35.0329301695253));
#26900=CARTESIAN_POINT('Ctrl Pts',(-0.109310347814557,3.93317613797182,
35.0388026838127));
#26901=CARTESIAN_POINT('Ctrl Pts',(-0.22459608319201,3.92658192317629,35.0446751981001));
#26902=CARTESIAN_POINT('Ctrl Pts',(-0.256458588840009,3.92475942358014,
35.0462982351483));
#26903=CARTESIAN_POINT('Ctrl Pts',(-0.288284915948909,3.92254987399867,
35.0479212721966));
#26904=CARTESIAN_POINT('Ctrl Pts',(-0.320064996648115,3.91995502498698,
35.0495443092448));
#26905=CARTESIAN_POINT('Ctrl Pts',(-0.435044857224395,3.91056689975203,
35.0554164332108));
#26906=CARTESIAN_POINT('Ctrl Pts',(-0.549804072018368,3.89609987364649,
35.0612885571768));
#26907=CARTESIAN_POINT('Ctrl Pts',(-0.663857834012495,3.87656829892371,
35.0671606811429));
#26908=CARTESIAN_POINT('Ctrl Pts',(-0.777763723039442,3.85706204727539,
35.0730251917836));
#26909=CARTESIAN_POINT('Ctrl Pts',(-0.890965574426317,3.83250437410963,
35.0788897024243));
#26910=CARTESIAN_POINT('Ctrl Pts',(-1.00298187849455,3.80296152378795,35.084754213065));
#26911=CARTESIAN_POINT('Ctrl Pts',(-1.11488291890037,3.77344907276532,35.0906126891826));
#26912=CARTESIAN_POINT('Ctrl Pts',(-1.22560044112233,3.73896175259171,35.0964711653002));
#26913=CARTESIAN_POINT('Ctrl Pts',(-1.33466199872459,3.69961705439367,35.1023296414178));
#26914=CARTESIAN_POINT('Ctrl Pts',(-1.44802399800991,3.65872094262829,35.108419125009));
#26915=CARTESIAN_POINT('Ctrl Pts',(-1.55959630369201,3.61257658314203,35.1145086086003));
#26916=CARTESIAN_POINT('Ctrl Pts',(-1.66886409402027,3.56137356025592,35.1205980921916));
#26917=CARTESIAN_POINT('Ctrl Pts',(-1.77386489214357,3.51217005524117,35.126449776712));
#26918=CARTESIAN_POINT('Ctrl Pts',(-1.87673737398393,3.45829575416629,35.1323014612324));
#26919=CARTESIAN_POINT('Ctrl Pts',(-1.97704478296076,3.39996807722773,35.1381531457528));
#26920=CARTESIAN_POINT('Ctrl Pts',(-2.07733689287734,3.34164929652778,35.1440039377641));
#26921=CARTESIAN_POINT('Ctrl Pts',(-2.17506435053188,3.27887869825674,35.1498547297754));
#26922=CARTESIAN_POINT('Ctrl Pts',(-2.26981594510763,3.21191914209171,35.1557055217867));
#26923=CARTESIAN_POINT('Ctrl Pts',(-2.36457603781286,3.14495358042376,35.1615568385468));
#26924=CARTESIAN_POINT('Ctrl Pts',(-2.45635939922802,3.07379855260523,35.167408155307));
#26925=CARTESIAN_POINT('Ctrl Pts',(-2.54478528928676,2.99875921531384,35.1732594720671));
#26926=CARTESIAN_POINT('Ctrl Pts',(-2.63324052778291,2.92369497256443,35.1791127308716));
#26927=CARTESIAN_POINT('Ctrl Pts',(-2.71833576408511,2.84474412420826,35.1849659896761));
#26928=CARTESIAN_POINT('Ctrl Pts',(-2.79972525940178,2.76225043612407,35.1908192484807));
#26929=CARTESIAN_POINT('Ctrl Pts',(-2.88120735114467,2.67966289537901,35.1966791665088));
#26930=CARTESIAN_POINT('Ctrl Pts',(-2.95897499634738,2.59352476425835,35.2025390845369));
#26931=CARTESIAN_POINT('Ctrl Pts',(-3.03272102596396,2.50421488268801,35.208399002565));
#26932=CARTESIAN_POINT('Ctrl Pts',(-3.10651671089285,2.4148448662184,35.2142628662436));
#26933=CARTESIAN_POINT('Ctrl Pts',(-3.1762851400794,2.32229917614978,35.2201267299223));
#26934=CARTESIAN_POINT('Ctrl Pts',(-3.24176199442419,2.22698634290983,35.2259905936009));
#26935=CARTESIAN_POINT('Ctrl Pts',(-3.3073354428715,2.13153290032515,35.2318631078883));
#26936=CARTESIAN_POINT('Ctrl Pts',(-3.36860446279633,2.03330451671135,35.2377356221756));
#26937=CARTESIAN_POINT('Ctrl Pts',(-3.42535020062493,1.93273510939258,35.243608136463));
#26938=CARTESIAN_POINT('Ctrl Pts',(-3.44103350599065,1.90493988131405,35.2452311735114));
#26939=CARTESIAN_POINT('Ctrl Pts',(-3.45637158232295,1.8769659537885,35.2468542105598));
#26940=CARTESIAN_POINT('Ctrl Pts',(-3.47136046246102,1.8488227442517,35.2484772476082));
#26941=CARTESIAN_POINT('Ctrl Pts',(-3.52559000846581,1.74700102960462,35.2543493715742));
#26942=CARTESIAN_POINT('Ctrl Pts',(-3.57542672946076,1.6426206029676,35.2602214955402));
#26943=CARTESIAN_POINT('Ctrl Pts',(-3.62062073765856,1.53609715644447,35.2660936195063));
#26944=CARTESIAN_POINT('Ctrl Pts',(-3.66575615092748,1.4297118196846,35.271958130147));
#26945=CARTESIAN_POINT('Ctrl Pts',(-3.70626066176825,1.32118936546262,35.2778226407877));
#26946=CARTESIAN_POINT('Ctrl Pts',(-3.74192982829283,1.21097075114654,35.2836871514284));
#26947=CARTESIAN_POINT('Ctrl Pts',(-3.77756229159994,1.10086555068798,35.289545627546));
#26948=CARTESIAN_POINT('Ctrl Pts',(-3.80836918061562,0.989068052643565,
35.2954041036637));
#26949=CARTESIAN_POINT('Ctrl Pts',(-3.8341940719254,0.876039279263296,35.3012625797813));
#26950=CARTESIAN_POINT('Ctrl Pts',(-3.86103727290798,0.758553631627159,
35.3073520633725));
#26951=CARTESIAN_POINT('Ctrl Pts',(-3.88249732192508,0.639738028258825,
35.3134415469638));
#26952=CARTESIAN_POINT('Ctrl Pts',(-3.89845556038526,0.52012810316428,35.3195310305551));
#26953=CARTESIAN_POINT('Ctrl Pts',(-3.91379061722067,0.405189038681629,
35.3253827150755));
#26954=CARTESIAN_POINT('Ctrl Pts',(-3.92404544006576,0.289516974445092,
35.3312343995959));
#26955=CARTESIAN_POINT('Ctrl Pts',(-3.92916697493633,0.173596898214589,
35.3370860841163));
#26956=CARTESIAN_POINT('Ctrl Pts',(-3.9342877286615,0.0576945023155024,
35.3429368761276));
#26957=CARTESIAN_POINT('Ctrl Pts',(-3.93427673289576,-0.0584554174693667,
35.3487876681389));
#26958=CARTESIAN_POINT('Ctrl Pts',(-3.92913297192955,-0.174364815533547,
35.3546384601502));
#26959=CARTESIAN_POINT('Ctrl Pts',(-3.92398874962709,-0.290284609338774,
35.3604897769103));
#26960=CARTESIAN_POINT('Ctrl Pts',(-3.91371086531983,-0.405963425509345,
35.3663410936704));
#26961=CARTESIAN_POINT('Ctrl Pts',(-3.89835035856407,-0.520916002713838,
35.3721924104306));
#26962=CARTESIAN_POINT('Ctrl Pts',(-3.88298475367618,-0.635906732528653,
35.3780456692351));
#26963=CARTESIAN_POINT('Ctrl Pts',(-3.86253322674438,-0.750170334535612,
35.3838989280396));
#26964=CARTESIAN_POINT('Ctrl Pts',(-3.8370982175806,-0.863230136545143,
35.3897521868441));
#26965=CARTESIAN_POINT('Ctrl Pts',(-3.81163427113265,-0.976418566132486,
35.3956121048722));
#26966=CARTESIAN_POINT('Ctrl Pts',(-3.78117561670702,-1.08840005854956,
35.4014720229003));
#26967=CARTESIAN_POINT('Ctrl Pts',(-3.74587504796018,-1.19871144362158,
35.4073319409285));
#26968=CARTESIAN_POINT('Ctrl Pts',(-3.71055071033013,-1.3090971045062,35.4131958046071));
#26969=CARTESIAN_POINT('Ctrl Pts',(-3.67037810963136,-1.41781003204734,
35.4190596682857));
#26970=CARTESIAN_POINT('Ctrl Pts',(-3.62555817622155,-1.52440706861163,
35.4249235319644));
#26971=CARTESIAN_POINT('Ctrl Pts',(-3.58067212263409,-1.6311613614335,35.4307960462517));
#26972=CARTESIAN_POINT('Ctrl Pts',(-3.53112522943475,-1.73579316120889,
35.4366685605391));
#26973=CARTESIAN_POINT('Ctrl Pts',(-3.47716435577114,-1.8378838491468,35.4425410748265));
#26974=CARTESIAN_POINT('Ctrl Pts',(-3.46225072715634,-1.86609952657313,
35.4441641118749));
#26975=CARTESIAN_POINT('Ctrl Pts',(-3.44700018962873,-1.89412127369666,
35.4457871489232));
#26976=CARTESIAN_POINT('Ctrl Pts',(-3.43141852376622,-1.92194066369231,
35.4474101859715));
#26977=CARTESIAN_POINT('Ctrl Pts',(-3.37504428780202,-2.0225908040453,35.4532823099376));
#26978=CARTESIAN_POINT('Ctrl Pts',(-3.31414339153919,-2.12092723197976,
35.4591544339036));
#26979=CARTESIAN_POINT('Ctrl Pts',(-3.24893058939597,-2.21651506317623,
35.4650265578697));
#26980=CARTESIAN_POINT('Ctrl Pts',(-3.18380233694565,-2.31197896285149,
35.4708910685104));
#26981=CARTESIAN_POINT('Ctrl Pts',(-3.11437352686747,-2.40470101416566,
35.4767555791511));
#26982=CARTESIAN_POINT('Ctrl Pts',(-3.04090472941805,-2.49427092085101,
35.4826200897918));
#26983=CARTESIAN_POINT('Ctrl Pts',(-2.96751153063028,-2.58374866099349,
35.4884785659094));
#26984=CARTESIAN_POINT('Ctrl Pts',(-2.89008687375796,-2.67008039031691,
35.494337042027));
#26985=CARTESIAN_POINT('Ctrl Pts',(-2.80893415916184,-2.75288537529149,
35.5001955181447));
#26986=CARTESIAN_POINT('Ctrl Pts',(-2.72458148553147,-2.83895547051,35.5062850017359));
#26987=CARTESIAN_POINT('Ctrl Pts',(-2.63620095757036,-2.92121459514035,
35.5123744853272));
#26988=CARTESIAN_POINT('Ctrl Pts',(-2.54417916322711,-2.99927347626071,
35.5184639689185));
#26989=CARTESIAN_POINT('Ctrl Pts',(-2.45575089153084,-3.0742840973563,35.5243156534389));
#26990=CARTESIAN_POINT('Ctrl Pts',(-2.36396075026656,-3.14541607190399,
35.5301673379593));
#26991=CARTESIAN_POINT('Ctrl Pts',(-2.26918816081457,-3.21236269602593,
35.5360190224797));
#26992=CARTESIAN_POINT('Ctrl Pts',(-2.17443002624266,-3.27929910933239,
35.541869814491));
#26993=CARTESIAN_POINT('Ctrl Pts',(-2.07669068551382,-3.34205120300941,
35.5477206065023));
#26994=CARTESIAN_POINT('Ctrl Pts',(-1.97638025177208,-3.40035440805886,
35.5535713985136));
#26995=CARTESIAN_POINT('Ctrl Pts',(-1.87606082133687,-3.45866284223598,
35.5594227152738));
#26996=CARTESIAN_POINT('Ctrl Pts',(-1.77317019692764,-3.51252138682477,
35.5652740320339));
#26997=CARTESIAN_POINT('Ctrl Pts',(-1.66814427682793,-3.5617107787812,35.5711253487941));
#26998=CARTESIAN_POINT('Ctrl Pts',(-1.56308349876298,-3.61091649663237,
35.5769786075986));
#26999=CARTESIAN_POINT('Ctrl Pts',(-1.45588638998729,-3.65544980515002,
35.5828318664031));
#27000=CARTESIAN_POINT('Ctrl Pts',(-1.34700939553298,-3.69513933273779,
35.5886851252076));
#27001=CARTESIAN_POINT('Ctrl Pts',(-1.23800853226013,-3.73487401490496,
35.5945450432357));
#27002=CARTESIAN_POINT('Ctrl Pts',(-1.12732435725081,-3.76975377516615,
35.6004049612638));
#27003=CARTESIAN_POINT('Ctrl Pts',(-1.01542916296309,-3.79965690753837,
35.6062648792919));
#27004=CARTESIAN_POINT('Ctrl Pts',(-0.903458626439311,-3.82958017454527,
35.6121287429706));
#27005=CARTESIAN_POINT('Ctrl Pts',(-0.790275849730697,-3.85452005260933,
35.6179926066492));
#27006=CARTESIAN_POINT('Ctrl Pts',(-0.676362296463616,-3.87440615371214,
35.6238564703278));
#27007=CARTESIAN_POINT('Ctrl Pts',(-0.562280693316787,-3.89432159159536,
35.6297289846152));
#27008=CARTESIAN_POINT('Ctrl Pts',(-0.447466570445664,-3.90916831983273,
35.6356014989026));
#27009=CARTESIAN_POINT('Ctrl Pts',(-0.33240556098613,-3.91892785631804,
35.64147401319));
#27010=CARTESIAN_POINT('Ctrl Pts',(-0.300605164761025,-3.92162518296817,
35.6430970502384));
#27011=CARTESIAN_POINT('Ctrl Pts',(-0.268785901634046,-3.92393423057186,
35.6447200872867));
#27012=CARTESIAN_POINT('Ctrl Pts',(-0.236957985810335,-3.92585530973324,
35.6463431243351));
#27013=CARTESIAN_POINT('Ctrl Pts',(-0.12180505847427,-3.93280574564311,
35.6522152483011));
#27014=CARTESIAN_POINT('Ctrl Pts',(-0.00615301487706181,-3.93469705103759,
35.6580873722671));
#27015=CARTESIAN_POINT('Ctrl Pts',(0.109516173067406,-3.93147494050727,
35.6639594962331));
#27016=CARTESIAN_POINT('Ctrl Pts',(0.225035393613353,-3.92825700750722,
35.6698240068738));
#27017=CARTESIAN_POINT('Ctrl Pts',(0.340571304870519,-3.9199388539467,35.6756885175145));
#27018=CARTESIAN_POINT('Ctrl Pts',(0.455637867855379,-3.90651803187649,
35.6815530281552));
#27019=CARTESIAN_POINT('Ctrl Pts',(0.570586028491408,-3.89311101969871,
35.6874115042727));
#27020=CARTESIAN_POINT('Ctrl Pts',(0.685065393318412,-3.87461183029995,
35.6932699803903));
#27021=CARTESIAN_POINT('Ctrl Pts',(0.798591655527019,-3.85107002892996,
35.6991284565079));
#27022=CARTESIAN_POINT('Ctrl Pts',(0.91659440863619,-3.8265999431475,35.7052179400992));
#27023=CARTESIAN_POINT('Ctrl Pts',(1.03356689370182,-3.79668140298861,35.7113074236904));
#27024=CARTESIAN_POINT('Ctrl Pts',(1.14897266828838,-3.76142935697672,35.7173969072817));
#27025=CARTESIAN_POINT('Ctrl Pts',(1.25987175760961,-3.7275539307822,35.7232485918021));
#27026=CARTESIAN_POINT('Ctrl Pts',(1.36932377014749,-3.68875386908664,35.7291002763224));
#27027=CARTESIAN_POINT('Ctrl Pts',(1.47686561295159,-3.64518270615906,35.7349519608428));
#27028=CARTESIAN_POINT('Ctrl Pts',(1.58439105328696,-3.60161818878097,35.7408027528541));
#27029=CARTESIAN_POINT('Ctrl Pts',(1.69000652011514,-3.55328417225595,35.7466535448653));
#27030=CARTESIAN_POINT('Ctrl Pts',(1.79326779031035,-3.50038278367315,35.7525043368766));
#27031=CARTESIAN_POINT('Ctrl Pts',(1.89653832185472,-3.4474766504438,35.7583556536367));
#27032=CARTESIAN_POINT('Ctrl Pts',(1.99745386907001,-3.39000251933694,35.7642069703967));
#27033=CARTESIAN_POINT('Ctrl Pts',(2.09559439821291,-3.32820869510592,35.7700582871568));
#27034=CARTESIAN_POINT('Ctrl Pts',(2.19376750006895,-3.26639436158554,35.7759115459613));
#27035=CARTESIAN_POINT('Ctrl Pts',(2.28916340279892,-3.2002577042806,35.7817648047657));
#27036=CARTESIAN_POINT('Ctrl Pts',(2.38139126813706,-3.13009019487308,35.7876180635702));
#27037=CARTESIAN_POINT('Ctrl Pts',(2.4737240606623,-3.05984285623649,35.7934779815983));
#27038=CARTESIAN_POINT('Ctrl Pts',(2.56288129257514,-2.98555576266775,35.7993378996263));
#27039=CARTESIAN_POINT('Ctrl Pts',(2.64850535321294,-2.90756055723736,35.8051978176544));
#27040=CARTESIAN_POINT('Ctrl Pts',(2.73418706698117,-2.82951283540307,35.811061681333));
#27041=CARTESIAN_POINT('Ctrl Pts',(2.81633058015491,-2.74775232106522,35.8169255450116));
#27042=CARTESIAN_POINT('Ctrl Pts',(2.89461650753271,-2.66264610384466,35.8227894086902));
#27043=CARTESIAN_POINT('Ctrl Pts',(2.9730179254756,-2.57741433449169,35.8286619229776));
#27044=CARTESIAN_POINT('Ctrl Pts',(3.04755013455306,-2.48882732664115,35.834534437265));
#27045=CARTESIAN_POINT('Ctrl Pts',(3.11793517238354,-2.39728372555558,35.8404069515523));
#27046=CARTESIAN_POINT('Ctrl Pts',(3.13738808786115,-2.37198303681087,35.842029988601));
#27047=CARTESIAN_POINT('Ctrl Pts',(3.15652448380116,-2.34645666696298,35.8436530256498));
#27048=CARTESIAN_POINT('Ctrl Pts',(3.17533910233628,-2.32071337850546,35.8452760626985));
#27049=CARTESIAN_POINT('Ctrl Pts',(3.24386965336691,-2.22694577221349,35.8511878287586));
#27050=CARTESIAN_POINT('Ctrl Pts',(3.30835742877721,-2.12998392340895,35.8570995948188));
#27051=CARTESIAN_POINT('Ctrl Pts',(3.36849264223259,-2.03020844230953,35.8630113608789));
#27052=CARTESIAN_POINT('Ctrl Pts',(3.42854818206181,-1.9305651545445,35.8689152943929));
#27053=CARTESIAN_POINT('Ctrl Pts',(3.48426242031965,-1.82811599172916,35.8748192279068));
#27054=CARTESIAN_POINT('Ctrl Pts',(3.53536685330977,-1.72327311025228,35.8807231614208));
#27055=CARTESIAN_POINT('Ctrl Pts',(3.58641539569186,-1.61854489069514,35.8866206380695));
#27056=CARTESIAN_POINT('Ctrl Pts',(3.63286398405451,-1.51142852206661,35.8925181147183));
#27057=CARTESIAN_POINT('Ctrl Pts',(3.67448867569264,-1.40236299587752,35.898415591367));
#27058=CARTESIAN_POINT('Ctrl Pts',(3.71708453564452,-1.29075280259325,35.9044506652502));
#27059=CARTESIAN_POINT('Ctrl Pts',(3.75462837515732,-1.17710173246275,35.9104857391334));
#27060=CARTESIAN_POINT('Ctrl Pts',(3.78693102001708,-1.06190510387342,35.9165208130165));
#27061=CARTESIAN_POINT('Ctrl Pts',(3.81844890924432,-0.949507044984043,
35.9224092717156));
#27062=CARTESIAN_POINT('Ctrl Pts',(3.84497722627513,-0.835638076692662,
35.9282977304147));
#27063=CARTESIAN_POINT('Ctrl Pts',(3.8663899645524,-0.720775722405051,35.9341861891138));
#27064=CARTESIAN_POINT('Ctrl Pts',(3.88860242803569,-0.601623476803267,
35.940294570589));
#27065=CARTESIAN_POINT('Ctrl Pts',(3.90530960984758,-0.481402630182505,
35.9464029520642));
#27066=CARTESIAN_POINT('Ctrl Pts',(3.91642873442305,-0.360659074730551,
35.9525113335394));
#27067=CARTESIAN_POINT('Ctrl Pts',(3.92754785899851,-0.239915519278558,
35.9586197150147));
#27068=CARTESIAN_POINT('Ctrl Pts',(3.93307887719384,-0.118649740920967,
35.9647280964899));
#27069=CARTESIAN_POINT('Ctrl Pts',(3.93299914955306,0.00258642898096291,
35.9708364779651));
#27070=CARTESIAN_POINT('',(3.93496388660084,0.00195648875352047,37.2208358380349));
#27071=CARTESIAN_POINT('Ctrl Pts',(3.9282775211904,0.00261363778016546,
35.9708380071379));
#27072=CARTESIAN_POINT('Ctrl Pts',(3.93118033843727,0.487443495032958,35.9952950051125));
#27073=CARTESIAN_POINT('Ctrl Pts',(3.62292672813806,2.28323870400638,36.086062982542));
#27074=CARTESIAN_POINT('Ctrl Pts',(0.933577472432809,4.55771548976854,36.2431419394252));
#27075=CARTESIAN_POINT('Ctrl Pts',(-3.3305959172111,3.24830235946759,36.4420748777888));
#27076=CARTESIAN_POINT('Ctrl Pts',(-4.53293738673136,-1.04728985028724,
36.6410078161523));
#27077=CARTESIAN_POINT('Ctrl Pts',(-1.56812897439943,-4.38010375485825,
36.8399407545156));
#27078=CARTESIAN_POINT('Ctrl Pts',(2.7129575081135,-3.70599985813041,37.0332163973897));
#27079=CARTESIAN_POINT('Ctrl Pts',(3.93099554165428,-1.19260423393931,37.1601810608092));
#27080=CARTESIAN_POINT('Ctrl Pts',(3.93831984400274,0.00193663700642166,
37.2208347447742));
#27081=CARTESIAN_POINT('',(3.93300214177874,-0.00350894827663559,38.4708364798097));
#27082=CARTESIAN_POINT('Ctrl Pts',(3.93299950757024,0.00196810879246953,
37.220836477965));
#27083=CARTESIAN_POINT('Ctrl Pts',(3.93294383452817,0.113223161314397,37.2264931957242));
#27084=CARTESIAN_POINT('Ctrl Pts',(3.92816790717577,0.22435667800964,37.2321499134834));
#27085=CARTESIAN_POINT('Ctrl Pts',(3.91869980905131,0.335083282992792,37.2378066312426));
#27086=CARTESIAN_POINT('Ctrl Pts',(3.90887116844884,0.450026325534738,37.2436787552018));
#27087=CARTESIAN_POINT('Ctrl Pts',(3.89396450975248,0.564729262387047,37.249550879161));
#27088=CARTESIAN_POINT('Ctrl Pts',(3.87399604281211,0.678707345087798,37.2554230031202));
#27089=CARTESIAN_POINT('Ctrl Pts',(3.85405346538562,0.79253765294116,37.261287513754));
#27090=CARTESIAN_POINT('Ctrl Pts',(3.82906220129585,0.905644572093272,37.2671520243879));
#27091=CARTESIAN_POINT('Ctrl Pts',(3.79909033948502,1.01754685023913,37.2730165350218));
#27092=CARTESIAN_POINT('Ctrl Pts',(3.76914931842163,1.12933398205476,37.2788750111326));
#27093=CARTESIAN_POINT('Ctrl Pts',(3.73423799979103,1.23991854148262,37.2847334872434));
#27094=CARTESIAN_POINT('Ctrl Pts',(3.69447568419538,1.34882853576318,37.2905919633542));
#27095=CARTESIAN_POINT('Ctrl Pts',(3.65314548775988,1.46203299556326,37.296681446948));
#27096=CARTESIAN_POINT('Ctrl Pts',(3.6065739399445,1.57342766445927,37.3027709305419));
#27097=CARTESIAN_POINT('Ctrl Pts',(3.55495259639291,1.6824984509352,37.3088604141357));
#27098=CARTESIAN_POINT('Ctrl Pts',(3.50534710653775,1.78730993819564,37.3147120986494));
#27099=CARTESIAN_POINT('Ctrl Pts',(3.45107901028721,1.88997522706534,37.3205637831631));
#27100=CARTESIAN_POINT('Ctrl Pts',(3.392367399822,1.99005839729012,37.3264154676768));
#27101=CARTESIAN_POINT('Ctrl Pts',(3.33366474415319,2.09012630265662,37.3322662596814));
#27102=CARTESIAN_POINT('Ctrl Pts',(3.27052013093913,2.1876125159477,37.338117051686));
#27103=CARTESIAN_POINT('Ctrl Pts',(3.20319799362034,2.28210683660223,37.3439678436907));
#27104=CARTESIAN_POINT('Ctrl Pts',(3.13586981827867,2.37660963231256,37.3498191604442));
#27105=CARTESIAN_POINT('Ctrl Pts',(3.06436361390616,2.46811966523383,37.3556704771977));
#27106=CARTESIAN_POINT('Ctrl Pts',(2.98898599387445,2.55625736740696,37.3615217939512));
#27107=CARTESIAN_POINT('Ctrl Pts',(2.91358335610828,2.64442432236928,37.3673750527492));
#27108=CARTESIAN_POINT('Ctrl Pts',(2.83430701626353,2.72921640696602,37.3732283115471));
#27109=CARTESIAN_POINT('Ctrl Pts',(2.75150206251009,2.81028920220014,37.3790815703451));
#27110=CARTESIAN_POINT('Ctrl Pts',(2.66860290196837,2.89145423355433,37.3849414883668));
#27111=CARTESIAN_POINT('Ctrl Pts',(2.58216741028541,2.96889124035578,37.3908014063884));
#27112=CARTESIAN_POINT('Ctrl Pts',(2.49257560162771,3.04229450746805,37.3966613244101));
#27113=CARTESIAN_POINT('Ctrl Pts',(2.4029234682402,3.11574719910163,37.4025251880824));
#27114=CARTESIAN_POINT('Ctrl Pts',(2.31011111636953,3.18516049589827,37.4083890517546));
#27115=CARTESIAN_POINT('Ctrl Pts',(2.21454808627185,3.25027164612278,37.4142529154269));
#27116=CARTESIAN_POINT('Ctrl Pts',(2.11884407772622,3.31547885095014,37.4201254297081));
#27117=CARTESIAN_POINT('Ctrl Pts',(2.02038164240613,3.37637102573865,37.4259979439892));
#27118=CARTESIAN_POINT('Ctrl Pts',(1.91959553306117,3.4327309812235,37.4318704582704));
#27119=CARTESIAN_POINT('Ctrl Pts',(1.89174041207018,3.44830766524553,37.4334934953822));
#27120=CARTESIAN_POINT('Ctrl Pts',(1.86370791579227,3.46353843799419,37.4351165324941));
#27121=CARTESIAN_POINT('Ctrl Pts',(1.83550747679674,3.47841936842343,37.4367395696059));
#27122=CARTESIAN_POINT('Ctrl Pts',(1.73347871087051,3.53225835184389,37.4426116935682));
#27123=CARTESIAN_POINT('Ctrl Pts',(1.62890808433844,3.5816947379408,37.4484838175304));
#27124=CARTESIAN_POINT('Ctrl Pts',(1.52221224378136,3.62648023362628,37.4543559414927));
#27125=CARTESIAN_POINT('Ctrl Pts',(1.41565473650146,3.67120766402677,37.4602204521296));
#27126=CARTESIAN_POINT('Ctrl Pts',(1.30697787232185,3.71129603691539,37.4660849627664));
#27127=CARTESIAN_POINT('Ctrl Pts',(1.19662338876077,3.74654260158225,37.4719494734033));
#27128=CARTESIAN_POINT('Ctrl Pts',(1.0863824588669,3.78175289788424,37.477807949517));
#27129=CARTESIAN_POINT('Ctrl Pts',(0.974467734634347,3.81213117071812,37.4836664256307));
#27130=CARTESIAN_POINT('Ctrl Pts',(0.861340834317039,3.83752276438043,37.4895249017444));
#27131=CARTESIAN_POINT('Ctrl Pts',(0.743753190362223,3.86391558223926,37.4956143853371));
#27132=CARTESIAN_POINT('Ctrl Pts',(0.624856227806823,3.88492019147547,37.5017038689298));
#27133=CARTESIAN_POINT('Ctrl Pts',(0.505186031405749,3.90041998683123,37.5077933525225));
#27134=CARTESIAN_POINT('Ctrl Pts',(0.390189049364761,3.91531450310821,37.5136450370389));
#27135=CARTESIAN_POINT('Ctrl Pts',(0.274478539588281,3.92512601396187,37.5194967215552));
#27136=CARTESIAN_POINT('Ctrl Pts',(0.158539689569357,3.9298033241921,37.5253484060716));
#27137=CARTESIAN_POINT('Ctrl Pts',(0.0426185227462051,3.9344799210308,37.5311991980788));
#27138=CARTESIAN_POINT('Ctrl Pts',(-0.0735305021100036,3.93402385758884,
37.537049990086));
#27139=CARTESIAN_POINT('Ctrl Pts',(-0.189419339084341,3.92843598827585,
37.5429007820933));
#27140=CARTESIAN_POINT('Ctrl Pts',(-0.305318569954967,3.92284761779523,
37.5487520988493));
#27141=CARTESIAN_POINT('Ctrl Pts',(-0.420957153596696,3.91212654639289,
37.5546034156052));
#27142=CARTESIAN_POINT('Ctrl Pts',(-0.535850027816559,3.89632567269331,
37.5604547323612));
#27143=CARTESIAN_POINT('Ctrl Pts',(-0.650781034830726,3.88051955470447,
37.5663079911616));
#27144=CARTESIAN_POINT('Ctrl Pts',(-0.76496543094427,3.85963033825317,37.572161249962));
#27145=CARTESIAN_POINT('Ctrl Pts',(-0.877926940000475,3.83376228892995,
37.5780145087623));
#27146=CARTESIAN_POINT('Ctrl Pts',(-0.991016964806267,3.80786480965508,
37.5838744267862));
#27147=CARTESIAN_POINT('Ctrl Pts',(-1.10288092238968,3.77697728386623,37.5897343448101));
#27148=CARTESIAN_POINT('Ctrl Pts',(-1.21305623145749,3.74125427889126,37.595594262834));
#27149=CARTESIAN_POINT('Ctrl Pts',(-1.3233057247134,3.70550722059488,37.6014581265084));
#27150=CARTESIAN_POINT('Ctrl Pts',(-1.43186391914719,3.66491834447394,37.6073219901828));
#27151=CARTESIAN_POINT('Ctrl Pts',(-1.53828843031218,3.61969027751929,37.6131858538572));
#27152=CARTESIAN_POINT('Ctrl Pts',(-1.64486994321869,3.57439548829174,37.6190583681404));
#27153=CARTESIAN_POINT('Ctrl Pts',(-1.74931111907896,3.52444802672684,37.6249308824235));
#27154=CARTESIAN_POINT('Ctrl Pts',(-1.85119428810024,3.47009635423932,37.6308033967067));
#27155=CARTESIAN_POINT('Ctrl Pts',(-1.87935261244782,3.45507471683406,37.6324264337942));
#27156=CARTESIAN_POINT('Ctrl Pts',(-1.90731571692631,3.43971691608275,37.6340494708818));
#27157=CARTESIAN_POINT('Ctrl Pts',(-1.93507519692215,3.42402876481152,37.6356725079694));
#27158=CARTESIAN_POINT('Ctrl Pts',(-2.03550858192254,3.36726926727036,37.6415446319685));
#27159=CARTESIAN_POINT('Ctrl Pts',(-2.13361092601821,3.30599200839285,37.6474167559676));
#27160=CARTESIAN_POINT('Ctrl Pts',(-2.22894817098408,3.24041340743226,37.6532888799667));
#27161=CARTESIAN_POINT('Ctrl Pts',(-2.32416180932104,3.17491983042843,37.6591533906405));
#27162=CARTESIAN_POINT('Ctrl Pts',(-2.41661714034022,3.10513623365194,37.6650179013144));
#27163=CARTESIAN_POINT('Ctrl Pts',(-2.50590486924698,3.03132475764051,37.6708824119883));
#27164=CARTESIAN_POINT('Ctrl Pts',(-2.59510072197035,2.95758923290243,37.6767408881391));
#27165=CARTESIAN_POINT('Ctrl Pts',(-2.6811351390289,2.87983433464965,37.6825993642899));
#27166=CARTESIAN_POINT('Ctrl Pts',(-2.76362855226727,2.79836491992969,37.6884578404407));
#27167=CARTESIAN_POINT('Ctrl Pts',(-2.84937478940238,2.71368305892279,37.6945473240195));
#27168=CARTESIAN_POINT('Ctrl Pts',(-2.93129464984765,2.62498797621149,37.7006368075984));
#27169=CARTESIAN_POINT('Ctrl Pts',(-3.00900034488857,2.53266774853325,37.7067262911772));
#27170=CARTESIAN_POINT('Ctrl Pts',(-3.08367157267096,2.44395269687256,37.7125779757308));
#27171=CARTESIAN_POINT('Ctrl Pts',(-3.15445130019248,2.3518906626465,37.7184296602843));
#27172=CARTESIAN_POINT('Ctrl Pts',(-3.22103427970653,2.25686223969374,37.7242813448378));
#27173=CARTESIAN_POINT('Ctrl Pts',(-3.28760710386799,2.16184831064238,37.7301321368822));
#27174=CARTESIAN_POINT('Ctrl Pts',(-3.3499842155701,2.06386923093621,37.7359829289266));
#27175=CARTESIAN_POINT('Ctrl Pts',(-3.40790261924258,1.96333612449819,37.741833720971));
#27176=CARTESIAN_POINT('Ctrl Pts',(-3.46582621752925,1.86279400139762,37.747685037764));
#27177=CARTESIAN_POINT('Ctrl Pts',(-3.51929010644619,1.75969775444043,37.7535363545571));
#27178=CARTESIAN_POINT('Ctrl Pts',(-3.5680766948491,1.65448411889468,37.7593876713502));
#27179=CARTESIAN_POINT('Ctrl Pts',(-3.61687947545567,1.54923556308354,37.7652409301875));
#27180=CARTESIAN_POINT('Ctrl Pts',(-3.66100169490512,1.44186859615042,37.7710941890248));
#27181=CARTESIAN_POINT('Ctrl Pts',(-3.700273731881,1.33284031644884,37.7769474478621));
#27182=CARTESIAN_POINT('Ctrl Pts',(-3.73959044845628,1.22368799582058,37.7828073659227));
#27183=CARTESIAN_POINT('Ctrl Pts',(-3.77404582853621,1.11287097908181,37.7886672839832));
#27184=CARTESIAN_POINT('Ctrl Pts',(-3.8035199767779,1.00086202158512,37.7945272020437));
#27185=CARTESIAN_POINT('Ctrl Pts',(-3.83301397080609,0.888777645255686,
37.8003910657546));
#27186=CARTESIAN_POINT('Ctrl Pts',(-3.8575199673137,0.775500133178189,37.8062549294654));
#27187=CARTESIAN_POINT('Ctrl Pts',(-3.87696942368804,0.66151121516421,37.8121187931763));
#27188=CARTESIAN_POINT('Ctrl Pts',(-3.89644757268483,0.547354136101167,
37.8179913074954));
#27189=CARTESIAN_POINT('Ctrl Pts',(-3.91085424229472,0.432483965168393,
37.8238638218144));
#27190=CARTESIAN_POINT('Ctrl Pts',(-3.92017281141305,0.317386402761502,
37.8297363361335));
#27191=CARTESIAN_POINT('Ctrl Pts',(-3.92274826362268,0.285575910435982,
37.8313593728667));
#27192=CARTESIAN_POINT('Ctrl Pts',(-3.92493536749216,0.253748039176991,
37.8329824095998));
#27193=CARTESIAN_POINT('Ctrl Pts',(-3.92673447276226,0.221913001918477,
37.8346054463329));
#27194=CARTESIAN_POINT('Ctrl Pts',(-3.93324361014652,0.106734288036302,
37.8404775702442));
#27195=CARTESIAN_POINT('Ctrl Pts',(-3.93469174171344,-0.00892415268081789,
37.8463496941556));
#27196=CARTESIAN_POINT('Ctrl Pts',(-3.93102642928762,-0.124580143852121,
37.8522218180669));
#27197=CARTESIAN_POINT('Ctrl Pts',(-3.92736586901214,-0.240086184734537,
37.858086328653));
#27198=CARTESIAN_POINT('Ctrl Pts',(-3.91860506174942,-0.355589373000882,
37.8639508392392));
#27199=CARTESIAN_POINT('Ctrl Pts',(-3.90474342198803,-0.470603663862904,
37.8698153498253));
#27200=CARTESIAN_POINT('Ctrl Pts',(-3.89089604571586,-0.585499606165482,
37.8756738258884));
#27201=CARTESIAN_POINT('Ctrl Pts',(-3.87195832603939,-0.699907243723816,
37.8815323019515));
#27202=CARTESIAN_POINT('Ctrl Pts',(-3.84798168362691,-0.813342463216951,
37.8873907780147));
#27203=CARTESIAN_POINT('Ctrl Pts',(-3.82305961012834,-0.93125058516743,
37.8934802616264));
#27204=CARTESIAN_POINT('Ctrl Pts',(-3.792693070022,-1.04810756904737,37.8995697452381));
#27205=CARTESIAN_POINT('Ctrl Pts',(-3.75699906654958,-1.16337741681088,
37.9056592288499));
#27206=CARTESIAN_POINT('Ctrl Pts',(-3.72269894210745,-1.27414588596759,
37.9115109133165));
#27207=CARTESIAN_POINT('Ctrl Pts',(-3.68347976335989,-1.38344841858774,
37.9173625977831));
#27208=CARTESIAN_POINT('Ctrl Pts',(-3.63949683794381,-1.49082251344585,
37.9232142822497));
#27209=CARTESIAN_POINT('Ctrl Pts',(-3.59552062087744,-1.59818023142654,
37.9290650742076));
#27210=CARTESIAN_POINT('Ctrl Pts',(-3.54678225846339,-1.70360971400905,
37.9349158661654));
#27211=CARTESIAN_POINT('Ctrl Pts',(-3.49348557849583,-1.80666751585389,
37.9407666581233));
#27212=CARTESIAN_POINT('Ctrl Pts',(-3.44018411842481,-1.90973456080647,
37.9466179748304));
#27213=CARTESIAN_POINT('Ctrl Pts',(-3.38232371800281,-2.01042913493269,
37.9524692915375));
#27214=CARTESIAN_POINT('Ctrl Pts',(-3.32015428965931,-2.10833215904347,
37.9583206082445));
#27215=CARTESIAN_POINT('Ctrl Pts',(-3.25796422735877,-2.20626767704789,
37.9641738669965));
#27216=CARTESIAN_POINT('Ctrl Pts',(-3.19146251485241,-2.3014094539185,37.9700271257484));
#27217=CARTESIAN_POINT('Ctrl Pts',(-3.12094211930887,-2.39336777113837,
37.9758803845003));
#27218=CARTESIAN_POINT('Ctrl Pts',(-3.05034149304818,-2.48543070889649,
37.9817403024767));
#27219=CARTESIAN_POINT('Ctrl Pts',(-2.97571330981273,-2.57430262972343,
37.9876002204532));
#27220=CARTESIAN_POINT('Ctrl Pts',(-2.89739058054179,-2.65962719639195,
37.9934601384296));
#27221=CARTESIAN_POINT('Ctrl Pts',(-2.81901511432891,-2.74500921454052,
37.999324002057));
#27222=CARTESIAN_POINT('Ctrl Pts',(-2.73694044074398,-2.82683883131214,
38.0051878656845));
#27223=CARTESIAN_POINT('Ctrl Pts',(-2.65153487054218,-2.90479807048595,
38.0110517293119));
#27224=CARTESIAN_POINT('Ctrl Pts',(-2.56600330657343,-2.98287231829664,
38.0169242435492));
#27225=CARTESIAN_POINT('Ctrl Pts',(-2.47713135497954,-3.05706452898509,
38.0227967577865));
#27226=CARTESIAN_POINT('Ctrl Pts',(-2.38531872319976,-3.12709826976266,
38.0286692720237));
#27227=CARTESIAN_POINT('Ctrl Pts',(-2.35994367196755,-3.1464541004993,38.0302923095813));
#27228=CARTESIAN_POINT('Ctrl Pts',(-2.33434415400022,-3.16549254905002,
38.0319153471388));
#27229=CARTESIAN_POINT('Ctrl Pts',(-2.30852895188268,-3.18420839115775,
38.0335383846963));
#27230=CARTESIAN_POINT('Ctrl Pts',(-2.21512996297538,-3.2519220089498,38.0394105086541));
#27231=CARTESIAN_POINT('Ctrl Pts',(-2.11859260879058,-3.31563630408255,
38.045282632612));
#27232=CARTESIAN_POINT('Ctrl Pts',(-2.01929427785179,-3.37504660996482,
38.0511547565698));
#27233=CARTESIAN_POINT('Ctrl Pts',(-1.9201246891795,-3.43437988920061,38.0570192672018));
#27234=CARTESIAN_POINT('Ctrl Pts',(-1.81820159388598,-3.48942006590099,
38.0628837778338));
#27235=CARTESIAN_POINT('Ctrl Pts',(-1.713933654004,-3.53990401418916,38.0687482884658));
#27236=CARTESIAN_POINT('Ctrl Pts',(-1.60977300480372,-3.59033601499247,
38.0746067645742));
#27237=CARTESIAN_POINT('Ctrl Pts',(-1.50327268008492,-3.63622093358974,
38.0804652406826));
#27238=CARTESIAN_POINT('Ctrl Pts',(-1.39486781808445,-3.67734044794228,
38.086323716791));
#27239=CARTESIAN_POINT('Ctrl Pts',(-1.28218840854103,-3.72008135930414,
38.0924132003855));
#27240=CARTESIAN_POINT('Ctrl Pts',(-1.16745156534972,-3.75767308877766,
38.0985026839801));
#27241=CARTESIAN_POINT('Ctrl Pts',(-1.05117152210389,-3.78992446245539,
38.1045921675746));
#27242=CARTESIAN_POINT('Ctrl Pts',(-0.939432305251541,-3.82091639483319,
38.1104438520846));
#27243=CARTESIAN_POINT('Ctrl Pts',(-0.826268588830766,-3.84697711368964,
38.1162955365947));
#27244=CARTESIAN_POINT('Ctrl Pts',(-0.712153460845849,-3.86798738987154,
38.1221472211047));
#27245=CARTESIAN_POINT('Ctrl Pts',(-0.598055737906514,-3.88899446152815,
38.1279980131053));
#27246=CARTESIAN_POINT('Ctrl Pts',(-0.483007298395968,-3.90495254727666,
38.1338488051058));
#27247=CARTESIAN_POINT('Ctrl Pts',(-0.367491413656636,-3.91579354165776,
38.1396995971063));
#27248=CARTESIAN_POINT('Ctrl Pts',(-0.251965168477452,-3.92663550835077,
38.1455509138553));
#27249=CARTESIAN_POINT('Ctrl Pts',(-0.135971806356071,-3.93235943270726,
38.1514022306043));
#27250=CARTESIAN_POINT('Ctrl Pts',(-0.0199989976658834,-3.93294915300114,
38.1572535473532));
#27251=CARTESIAN_POINT('Ctrl Pts',(0.0960123022405029,-3.93353906902237,
38.1631068061462));
#27252=CARTESIAN_POINT('Ctrl Pts',(0.212002621962486,-3.9289913905169,38.1689600649392));
#27253=CARTESIAN_POINT('Ctrl Pts',(0.327485731892573,-3.91934204878916,
38.1748133237322));
#27254=CARTESIAN_POINT('Ctrl Pts',(0.443100226376169,-3.90968172905385,
38.1806732417482));
#27255=CARTESIAN_POINT('Ctrl Pts',(0.558205947068432,-3.89490819563718,
38.1865331597643));
#27256=CARTESIAN_POINT('Ctrl Pts',(0.672323115213581,-3.87510911185085,
38.1923930777804));
#27257=CARTESIAN_POINT('Ctrl Pts',(0.786517121708234,-3.85529669677577,
38.1982569414466));
#27258=CARTESIAN_POINT('Ctrl Pts',(0.899720847457973,-3.83045208183573,
38.2041208051129));
#27259=CARTESIAN_POINT('Ctrl Pts',(1.0114677180855,-3.80071336136664,38.2099846687792));
#27260=CARTESIAN_POINT('Ctrl Pts',(1.12337944220788,-3.77093076913654,38.2158571830539));
#27261=CARTESIAN_POINT('Ctrl Pts',(1.23382962884221,-3.73623978505086,38.2217296973286));
#27262=CARTESIAN_POINT('Ctrl Pts',(1.34236969486437,-3.69682736982804,38.2276022116033));
#27263=CARTESIAN_POINT('Ctrl Pts',(1.37236784410884,-3.68593462250193,38.2292252487554));
#27264=CARTESIAN_POINT('Ctrl Pts',(1.40222022487575,-3.67468150291303,38.2308482859076));
#27265=CARTESIAN_POINT('Ctrl Pts',(1.43191769561372,-3.66307257817645,38.2324713230597));
#27266=CARTESIAN_POINT('Ctrl Pts',(1.53936270135205,-3.62107166180405,38.2383434472439));
#27267=CARTESIAN_POINT('Ctrl Pts',(1.64513831810261,-3.57426896837866,38.244215571428));
#27268=CARTESIAN_POINT('Ctrl Pts',(1.74878426559977,-3.52281742251719,38.2500876956121));
#27269=CARTESIAN_POINT('Ctrl Pts',(1.85229583408655,-3.47143258459735,38.2559522064717));
#27270=CARTESIAN_POINT('Ctrl Pts',(1.95368285738747,-3.41541106253365,38.2618167173313));
#27271=CARTESIAN_POINT('Ctrl Pts',(2.05250311076411,-3.35495454221121,38.2676812281908));
#27272=CARTESIAN_POINT('Ctrl Pts',(2.15122167909573,-3.29456023103903,38.2735397045278));
#27273=CARTESIAN_POINT('Ctrl Pts',(2.24737838040768,-3.22974021321016,38.2793981808648));
#27274=CARTESIAN_POINT('Ctrl Pts',(2.34055438342991,-3.16074266244613,38.2852566572018));
#27275=CARTESIAN_POINT('Ctrl Pts',(2.43740443474394,-3.08902445051076,38.291346140711));
#27276=CARTESIAN_POINT('Ctrl Pts',(2.53103347873433,-3.01279267932383,38.2974356242203));
#27277=CARTESIAN_POINT('Ctrl Pts',(2.62100278877615,-2.93237674612722,38.3035251077295));
#27278=CARTESIAN_POINT('Ctrl Pts',(2.70745873168408,-2.85510111373542,38.3093767924692));
#27279=CARTESIAN_POINT('Ctrl Pts',(2.79053507015703,-2.77396227756016,38.3152284772089));
#27280=CARTESIAN_POINT('Ctrl Pts',(2.86987584775278,-2.68929388845571,38.3210801619486));
#27281=CARTESIAN_POINT('Ctrl Pts',(2.94920452415025,-2.60463841312645,38.3269309541787));
#27282=CARTESIAN_POINT('Ctrl Pts',(3.02479848991697,-2.51645475682456,38.3327817464089));
#27283=CARTESIAN_POINT('Ctrl Pts',(3.09633930368138,-2.42511276366232,38.3386325386391));
#27284=CARTESIAN_POINT('Ctrl Pts',(3.16788653382689,-2.33376257818289,38.3444838556175));
#27285=CARTESIAN_POINT('Ctrl Pts',(3.23537963439635,-2.23925381822338,38.3503351725959));
#27286=CARTESIAN_POINT('Ctrl Pts',(3.2985414946412,-2.14198809710283,38.3561864895743));
#27287=CARTESIAN_POINT('Ctrl Pts',(3.361724318215,-2.04469009363182,38.3620397485962));
#27288=CARTESIAN_POINT('Ctrl Pts',(3.42057281799139,-1.94463365605857,38.3678930076182));
#27289=CARTESIAN_POINT('Ctrl Pts',(3.4748544949905,-1.84224733373245,38.3737462666401));
#27290=CARTESIAN_POINT('Ctrl Pts',(3.52919792796067,-1.73974452703981,38.3796061848832));
#27291=CARTESIAN_POINT('Ctrl Pts',(3.57896397401331,-1.63490691034585,38.3854661031264));
#27292=CARTESIAN_POINT('Ctrl Pts',(3.62396714934554,-1.52818555825672,38.3913260213695));
#27293=CARTESIAN_POINT('Ctrl Pts',(3.66900062659402,-1.42139234764983,38.397189885262));
#27294=CARTESIAN_POINT('Ctrl Pts',(3.70926470413201,-1.3127132627864,38.4030537491546));
#27295=CARTESIAN_POINT('Ctrl Pts',(3.74462346788478,-1.20261551784705,38.4089176130471));
#27296=CARTESIAN_POINT('Ctrl Pts',(3.78003439429353,-1.09235535233121,38.4147901275451));
#27297=CARTESIAN_POINT('Ctrl Pts',(3.81052545570312,-0.980672747095065,
38.4206626420431));
#27298=CARTESIAN_POINT('Ctrl Pts',(3.83601157778903,-0.868046182566633,
38.4265351565411));
#27299=CARTESIAN_POINT('Ctrl Pts',(3.84305538622439,-0.8369186558838,38.4281581915018));
#27300=CARTESIAN_POINT('Ctrl Pts',(3.84971719773295,-0.805719058755463,
38.4297812264625));
#27301=CARTESIAN_POINT('Ctrl Pts',(3.85599591566377,-0.774457551053836,
38.4314042614232));
#27302=CARTESIAN_POINT('Ctrl Pts',(3.88876514262491,-0.611300764539638,
38.4398750354855));
#27303=CARTESIAN_POINT('Ctrl Pts',(3.91118760611058,-0.446001857174323,
38.4483458095477));
#27304=CARTESIAN_POINT('Ctrl Pts',(3.92304612497759,-0.279639234189963,
38.45681658361));
#27305=CARTESIAN_POINT('Ctrl Pts',(3.92958843073383,-0.187857523659283,
38.4614898817283));
#27306=CARTESIAN_POINT('Ctrl Pts',(3.93291613600371,-0.095752414987991,
38.4661631798467));
#27307=CARTESIAN_POINT('Ctrl Pts',(3.93299843466147,-0.00350898139352327,
38.470836477965));
#27308=CARTESIAN_POINT('',(3.93045782683572,-0.000399788568204086,39.7208363664874));
#27309=CARTESIAN_POINT('Ctrl Pts',(3.93439718561015,-0.00349648589506154,
38.4708371739967));
#27310=CARTESIAN_POINT('Ctrl Pts',(3.92467201342099,1.04631151308355,38.52400384926));
#27311=CARTESIAN_POINT('Ctrl Pts',(2.95138670712728,3.42137387922279,38.6434815039779));
#27312=CARTESIAN_POINT('Ctrl Pts',(-1.06465162905695,4.5288909683736,38.82927013815));
#27313=CARTESIAN_POINT('Ctrl Pts',(-4.38608045124232,1.55133378955204,39.0282030765135));
#27314=CARTESIAN_POINT('Ctrl Pts',(-3.67536551296059,-2.85237220456728,
39.2271360148771));
#27315=CARTESIAN_POINT('Ctrl Pts',(0.414129357579048,-4.63387829221155,
39.4260689532403));
#27316=CARTESIAN_POINT('Ctrl Pts',(3.48221100255245,-2.58359817983051,39.5906356795963));
#27317=CARTESIAN_POINT('Ctrl Pts',(3.92709165371068,-0.634376258868161,
39.6888914264977));
#27318=CARTESIAN_POINT('Ctrl Pts',(3.9265231354041,-0.000402814833626348,
39.7208361939446));
#27319=CARTESIAN_POINT('',(3.93299828088553,0.00367730219960298,40.9708364779999));
#27320=CARTESIAN_POINT('Ctrl Pts',(3.93299997987905,-0.000397833337409791,
39.720836477965));
#27321=CARTESIAN_POINT('Ctrl Pts',(3.93301221516407,0.120560797364908,39.7269213266806));
#27322=CARTESIAN_POINT('Ctrl Pts',(3.92744003772526,0.241429729961996,39.7330061753961));
#27323=CARTESIAN_POINT('Ctrl Pts',(3.91633416341394,0.361684559356363,39.7390910241117));
#27324=CARTESIAN_POINT('Ctrl Pts',(3.90521572833616,0.482075397207768,39.7451827548036));
#27325=CARTESIAN_POINT('Ctrl Pts',(3.88855115022812,0.601850385441626,39.7512744854954));
#27326=CARTESIAN_POINT('Ctrl Pts',(3.86644259922617,0.720493321890755,39.7573662161873));
#27327=CARTESIAN_POINT('Ctrl Pts',(3.84428593703237,0.83939444138757,39.7634712033076));
#27328=CARTESIAN_POINT('Ctrl Pts',(3.81666169142604,0.957158227337841,39.7695761904279));
#27329=CARTESIAN_POINT('Ctrl Pts',(3.78372278395199,1.07328043595445,39.7756811775482));
#27330=CARTESIAN_POINT('Ctrl Pts',(3.75074559613254,1.18953759738512,39.7817932596523));
#27331=CARTESIAN_POINT('Ctrl Pts',(3.7124415414633,1.30414903190815,39.7879053417564));
#27332=CARTESIAN_POINT('Ctrl Pts',(3.6690122216127,1.41662920965814,39.7940174238605));
#27333=CARTESIAN_POINT('Ctrl Pts',(3.62548637651813,1.52935938387681,39.800143090571));
#27334=CARTESIAN_POINT('Ctrl Pts',(3.57681264168092,1.6399484994239,39.8062687572815));
#27335=CARTESIAN_POINT('Ctrl Pts',(3.52323976422024,1.74793322636116,39.8123944239921));
#27336=CARTESIAN_POINT('Ctrl Pts',(3.48959701781275,1.81574557761853,39.8162412259838));
#27337=CARTESIAN_POINT('Ctrl Pts',(3.45402314951959,1.88253138719219,39.8200880279755));
#27338=CARTESIAN_POINT('Ctrl Pts',(3.4165884287368,1.94818184690798,39.8239348299672));
#27339=CARTESIAN_POINT('Ctrl Pts',(3.35944435755049,2.04839722089677,39.8298069701157));
#27340=CARTESIAN_POINT('Ctrl Pts',(3.29779147146901,2.14626424612989,39.8356791102642));
#27341=CARTESIAN_POINT('Ctrl Pts',(3.23184785271714,2.24134969535939,39.8415512504126));
#27342=CARTESIAN_POINT('Ctrl Pts',(3.16598973252548,2.3363118624706,39.8474157770946));
#27343=CARTESIAN_POINT('Ctrl Pts',(3.09585217608569,2.42849928888059,39.8532803037766));
#27344=CARTESIAN_POINT('Ctrl Pts',(3.02169889165576,2.51750368582974,39.8591448304587));
#27345=CARTESIAN_POINT('Ctrl Pts',(2.94762191199982,2.60641649600097,39.8650033224601));
#27346=CARTESIAN_POINT('Ctrl Pts',(2.86953768660722,2.69215247589465,39.8708618144616));
#27347=CARTESIAN_POINT('Ctrl Pts',(2.78775252601083,2.77433322687096,39.8767203064631));
#27348=CARTESIAN_POINT('Ctrl Pts',(2.70274278262887,2.85975415776465,39.8828097840409));
#27349=CARTESIAN_POINT('Ctrl Pts',(2.61373452287241,2.94133337134355,39.8888992616187));
#27350=CARTESIAN_POINT('Ctrl Pts',(2.52111730365917,3.01868457133075,39.8949887391965));
#27351=CARTESIAN_POINT('Ctrl Pts',(2.432116536821,3.09301541578056,39.9008404391145));
#27352=CARTESIAN_POINT('Ctrl Pts',(2.33978370955459,3.16344194615921,39.9066921390324));
#27353=CARTESIAN_POINT('Ctrl Pts',(2.2445005837303,3.22966037372885,39.9125438389503));
#27354=CARTESIAN_POINT('Ctrl Pts',(2.14923199393858,3.29586869926612,39.9183946461551));
#27355=CARTESIAN_POINT('Ctrl Pts',(2.05101433988827,3.35786996257495,39.9242454533599));
#27356=CARTESIAN_POINT('Ctrl Pts',(1.95025975148123,3.41540274371155,39.9300962605647));
#27357=CARTESIAN_POINT('Ctrl Pts',(1.84949613034208,3.47294068270952,39.9359475922991));
#27358=CARTESIAN_POINT('Ctrl Pts',(1.74619548174536,3.52600913816299,39.9417989240336));
#27359=CARTESIAN_POINT('Ctrl Pts',(1.6407953728763,3.57439219229615,39.9476502557681));
#27360=CARTESIAN_POINT('Ctrl Pts',(1.53536028615924,3.6227913027231,39.9535035293126));
#27361=CARTESIAN_POINT('Ctrl Pts',(1.42782472930042,3.66650174766016,39.9593568028571));
#27362=CARTESIAN_POINT('Ctrl Pts',(1.31864644875282,3.70535565677461,39.9652100764017));
#27363=CARTESIAN_POINT('Ctrl Pts',(1.20934396475316,3.74425376689327,39.9710700087503));
#27364=CARTESIAN_POINT('Ctrl Pts',(1.0983954167113,3.77828417495523,39.9769299410989));
#27365=CARTESIAN_POINT('Ctrl Pts',(0.986274017562826,3.80732879618775,39.9827898734475));
#27366=CARTESIAN_POINT('Ctrl Pts',(0.874077128378057,3.83639297282653,39.9886537512206));
#27367=CARTESIAN_POINT('Ctrl Pts',(0.760706219113384,3.86046459279032,39.9945176289936));
#27368=CARTESIAN_POINT('Ctrl Pts',(0.646643280547311,3.87947695800903,40.0003815067666));
#27369=CARTESIAN_POINT('Ctrl Pts',(0.532412080682976,3.89851736954405,40.0062540347086));
#27370=CARTESIAN_POINT('Ctrl Pts',(0.417487222934432,3.91248358144626,40.0121265626506));
#27371=CARTESIAN_POINT('Ctrl Pts',(0.302354469892053,3.92136083197355,40.0179990905925));
#27372=CARTESIAN_POINT('Ctrl Pts',(0.270537151625742,3.92381408960783,40.0196219831719));
#27373=CARTESIAN_POINT('Ctrl Pts',(0.238703945366235,3.92587900390329,40.0212448757513));
#27374=CARTESIAN_POINT('Ctrl Pts',(0.206865059890492,3.92755596357283,40.0228677683307));
#27375=CARTESIAN_POINT('Ctrl Pts',(0.0916611675682571,3.93362377274115,
40.0287399444189));
#27376=CARTESIAN_POINT('Ctrl Pts',(-0.0240030362714795,3.93462867850176,
40.0346121205071));
#27377=CARTESIAN_POINT('Ctrl Pts',(-0.139645169554283,3.93052009619849,
40.0404842965954));
#27378=CARTESIAN_POINT('Ctrl Pts',(-0.255137378609357,3.92641684046617,
40.0463488597017));
#27379=CARTESIAN_POINT('Ctrl Pts',(-0.370607164683488,3.91721329465202,
40.0522134228081));
#27380=CARTESIAN_POINT('Ctrl Pts',(-0.485568476785245,3.90291074127406,
40.0580779859144));
#27381=CARTESIAN_POINT('Ctrl Pts',(-0.600411501363643,3.88862290426969,
40.0639365147765));
#27382=CARTESIAN_POINT('Ctrl Pts',(-0.71474668483969,3.86924654605267,40.0697950436385));
#27383=CARTESIAN_POINT('Ctrl Pts',(-0.828090107617243,3.84483494751939,
40.0756535725005));
#27384=CARTESIAN_POINT('Ctrl Pts',(-0.945901370540731,3.81946107771107,
40.0817430364253));
#27385=CARTESIAN_POINT('Ctrl Pts',(-1.06264062231353,3.78864685520957,40.08783250035));
#27386=CARTESIAN_POINT('Ctrl Pts',(-1.1777723297283,3.75251133766793,40.0939219642747));
#27387=CARTESIAN_POINT('Ctrl Pts',(-1.28840941579538,3.71778651290763,40.0997737019017));
#27388=CARTESIAN_POINT('Ctrl Pts',(-1.39756168502639,3.6781482099432,40.1056254395288));
#27389=CARTESIAN_POINT('Ctrl Pts',(-1.50476722862093,3.63375351223339,40.1114771771558));
#27390=CARTESIAN_POINT('Ctrl Pts',(-1.61195642198051,3.58936558529041,40.117328022317));
#27391=CARTESIAN_POINT('Ctrl Pts',(-1.71719909819135,3.54022286407388,40.1231788674782));
#27392=CARTESIAN_POINT('Ctrl Pts',(-1.82005259035601,3.48653087873009,40.1290297126394));
#27393=CARTESIAN_POINT('Ctrl Pts',(-1.92291530698139,3.43283407799695,40.1348810825362));
#27394=CARTESIAN_POINT('Ctrl Pts',(-2.02338804710449,3.37458739338451,40.140732452433));
#27395=CARTESIAN_POINT('Ctrl Pts',(-2.12105268651087,3.31204234590155,40.1465838223298));
#27396=CARTESIAN_POINT('Ctrl Pts',(-2.21874973922562,3.24947654073265,40.1524371342013));
#27397=CARTESIAN_POINT('Ctrl Pts',(-2.31363649012476,3.18260975890633,40.1582904460728));
#27398=CARTESIAN_POINT('Ctrl Pts',(-2.40532434044997,3.11173646333344,40.1641437579443));
#27399=CARTESIAN_POINT('Ctrl Pts',(-2.49711649680897,3.04078254080358,40.1700037286669));
#27400=CARTESIAN_POINT('Ctrl Pts',(-2.58570216169739,2.96581326006773,40.1758636993896));
#27401=CARTESIAN_POINT('Ctrl Pts',(-2.67072627081659,2.88716299961919,40.1817236701122));
#27402=CARTESIAN_POINT('Ctrl Pts',(-2.7558076263903,2.80845978420761,40.1875875863339));
#27403=CARTESIAN_POINT('Ctrl Pts',(-2.8373223612883,2.72607094727657,40.1934515025557));
#27404=CARTESIAN_POINT('Ctrl Pts',(-2.91495390705511,2.64036602003286,40.1993154187774));
#27405=CARTESIAN_POINT('Ctrl Pts',(-2.99269996862671,2.55453466778213,40.2051879849762));
#27406=CARTESIAN_POINT('Ctrl Pts',(-3.06655114597935,2.46537777960961,40.2110605511749));
#27407=CARTESIAN_POINT('Ctrl Pts',(-3.13623253395467,2.37329612416239,40.2169331173736));
#27408=CARTESIAN_POINT('Ctrl Pts',(-3.15548478634672,2.34785490775071,40.2185556471471));
#27409=CARTESIAN_POINT('Ctrl Pts',(-3.17441899725897,2.32219058273379,40.2201781769206));
#27410=CARTESIAN_POINT('Ctrl Pts',(-3.1930299809604,2.29631194324465,40.2218007066941));
#27411=CARTESIAN_POINT('Ctrl Pts',(-3.26038337409214,2.20265680887942,40.2276726631395));
#27412=CARTESIAN_POINT('Ctrl Pts',(-3.32372571208478,2.10587877460033,40.2335446195849));
#27413=CARTESIAN_POINT('Ctrl Pts',(-3.38275377933201,2.00635636625575,40.2394165760303));
#27414=CARTESIAN_POINT('Ctrl Pts',(-3.44170531139888,1.90696299763461,40.2452809189578));
#27415=CARTESIAN_POINT('Ctrl Pts',(-3.49635348786262,1.80483268346802,40.2511452618853));
#27416=CARTESIAN_POINT('Ctrl Pts',(-3.54643675227542,1.70037506512833,40.2570096048129));
#27417=CARTESIAN_POINT('Ctrl Pts',(-3.59646848004553,1.5960249356877,40.2628679132187));
#27418=CARTESIAN_POINT('Ctrl Pts',(-3.64194446140186,1.4893526360771,40.2687262216245));
#27419=CARTESIAN_POINT('Ctrl Pts',(-3.6826480441159,1.38079411324402,40.2745845300303));
#27420=CARTESIAN_POINT('Ctrl Pts',(-3.72495827103363,1.26795058870246,40.2806740764898));
#27421=CARTESIAN_POINT('Ctrl Pts',(-3.76211135809236,1.15306926060779,40.2867636229493));
#27422=CARTESIAN_POINT('Ctrl Pts',(-3.79391808266823,1.03666512529506,40.2928531694087));
#27423=CARTESIAN_POINT('Ctrl Pts',(-3.82448154379396,0.924811002874548,
40.298704687255));
#27424=CARTESIAN_POINT('Ctrl Pts',(-3.8501086301726,0.811551320650944,40.3045562051013));
#27425=CARTESIAN_POINT('Ctrl Pts',(-3.8706819284736,0.697359597759905,40.3104077229476));
#27426=CARTESIAN_POINT('Ctrl Pts',(-3.89125209113257,0.583185279193724,
40.3162583489453));
#27427=CARTESIAN_POINT('Ctrl Pts',(-3.9067699239503,0.46807960918544,40.3221089749431));
#27428=CARTESIAN_POINT('Ctrl Pts',(-3.91716917591749,0.352526094412765,
40.3279596009409));
#27429=CARTESIAN_POINT('Ctrl Pts',(-3.9275693620848,0.236962199075433,40.3338107525203));
#27430=CARTESIAN_POINT('Ctrl Pts',(-3.93285001626266,0.120950790796229,
40.3396619040996));
#27431=CARTESIAN_POINT('Ctrl Pts',(-3.93299684767512,0.00497957604032452,
40.345513055679));
#27432=CARTESIAN_POINT('Ctrl Pts',(-3.93314372784736,-0.111030150432251,
40.3513661503086));
#27433=CARTESIAN_POINT('Ctrl Pts',(-3.92815339477199,-0.226999243621648,
40.3572192449382));
#27434=CARTESIAN_POINT('Ctrl Pts',(-3.91806364478637,-0.34244163795214,
40.3630723395677));
#27435=CARTESIAN_POINT('Ctrl Pts',(-3.90796241143149,-0.458015419843687,
40.3689320957347));
#27436=CARTESIAN_POINT('Ctrl Pts',(-3.89275021303907,-0.57306089428121,
40.3747918519017));
#27437=CARTESIAN_POINT('Ctrl Pts',(-3.87251655278508,-0.687098645323602,
40.3806516080687));
#27438=CARTESIAN_POINT('Ctrl Pts',(-3.85226926429982,-0.801213205644506,
40.3865153110308));
#27439=CARTESIAN_POINT('Ctrl Pts',(-3.82699386935437,-0.914318288559313,
40.3923790139929));
#27440=CARTESIAN_POINT('Ctrl Pts',(-3.79683025086908,-1.0259478768853,40.3982427169551));
#27441=CARTESIAN_POINT('Ctrl Pts',(-3.76662211752302,-1.13774220590991,
40.404115073452));
#27442=CARTESIAN_POINT('Ctrl Pts',(-3.73151148787811,-1.24805630196375,
40.4099874299489));
#27443=CARTESIAN_POINT('Ctrl Pts',(-3.69168704150918,-1.35644232739664,
40.4158597864458));
#27444=CARTESIAN_POINT('Ctrl Pts',(-3.680669390645,-1.38642791403136,40.417484405983));
#27445=CARTESIAN_POINT('Ctrl Pts',(-3.66929122729997,-1.41626606714415,
40.4191090255203));
#27446=CARTESIAN_POINT('Ctrl Pts',(-3.65755716757587,-1.44594763595172,
40.4207336450576));
#27447=CARTESIAN_POINT('Ctrl Pts',(-3.6151437429181,-1.55323335052489,40.4266059245553));
#27448=CARTESIAN_POINT('Ctrl Pts',(-3.56793476664441,-1.65883117085618,
40.432478204053));
#27449=CARTESIAN_POINT('Ctrl Pts',(-3.51608493954222,-1.76228139010897,
40.4383504835507));
#27450=CARTESIAN_POINT('Ctrl Pts',(-3.46430234261555,-1.8655974724362,40.4442151488594));
#27451=CARTESIAN_POINT('Ctrl Pts',(-3.40789104497284,-1.96677112519497,
40.4500798141681));
#27452=CARTESIAN_POINT('Ctrl Pts',(-3.34705443881563,-2.06536088459248,
40.4559444794768));
#27453=CARTESIAN_POINT('Ctrl Pts',(-3.28628044193404,-2.16384918150202,
40.4618031092344));
#27454=CARTESIAN_POINT('Ctrl Pts',(-3.22109041095424,-2.25975852461353,
40.467661738992));
#27455=CARTESIAN_POINT('Ctrl Pts',(-3.15173413566648,-2.35267102206719,
40.4735203687496));
#27456=CARTESIAN_POINT('Ctrl Pts',(-3.07964562751407,-2.4492437301943,40.4796097943609));
#27457=CARTESIAN_POINT('Ctrl Pts',(-3.0030560804933,-2.54257821622054,40.4856992199722));
#27458=CARTESIAN_POINT('Ctrl Pts',(-2.92229654886902,-2.63223704868468,
40.4917886455835));
#27459=CARTESIAN_POINT('Ctrl Pts',(-2.84468800944538,-2.71839766519671,
40.4976404802601));
#27460=CARTESIAN_POINT('Ctrl Pts',(-2.76322908759393,-2.80116374017019,
40.5034923149366));
#27461=CARTESIAN_POINT('Ctrl Pts',(-2.6782548069731,-2.88018058269364,40.5093441496132));
#27462=CARTESIAN_POINT('Ctrl Pts',(-2.59329350864828,-2.95918535309325,
40.5151950902516));
#27463=CARTESIAN_POINT('Ctrl Pts',(-2.50481822207306,-3.03444174853172,
40.52104603089));
#27464=CARTESIAN_POINT('Ctrl Pts',(-2.4132000205352,-3.10563273116589,40.5268969715284));
#27465=CARTESIAN_POINT('Ctrl Pts',(-2.32157362839142,-3.17683007822628,
40.532748435237));
#27466=CARTESIAN_POINT('Ctrl Pts',(-2.22680408918084,-3.24396103632612,
40.5385998989456));
#27467=CARTESIAN_POINT('Ctrl Pts',(-2.12929408747564,-3.30675001913378,
40.5444513626542));
#27468=CARTESIAN_POINT('Ctrl Pts',(-2.03175175363044,-3.3695598213666,40.5503047665775));
#27469=CARTESIAN_POINT('Ctrl Pts',(-1.93146749782905,-3.42802456186416,
40.5561581705008));
#27470=CARTESIAN_POINT('Ctrl Pts',(-1.82887077054162,-3.48191336834484,
40.5620115744242));
#27471=CARTESIAN_POINT('Ctrl Pts',(-1.72615738244759,-3.53586345077259,
40.5678716341429));
#27472=CARTESIAN_POINT('Ctrl Pts',(-1.62112664071319,-3.58522702136902,
40.5737316938616));
#27473=CARTESIAN_POINT('Ctrl Pts',(-1.51423034177429,-3.62982030850704,
40.5795917535803));
#27474=CARTESIAN_POINT('Ctrl Pts',(-1.40726210138794,-3.67444360702669,
40.5854557571323));
#27475=CARTESIAN_POINT('Ctrl Pts',(-1.29842619104318,-3.71429008774057,
40.5913197606842));
#27476=CARTESIAN_POINT('Ctrl Pts',(-1.18819035846714,-3.74922560964871,
40.5971837642362));
#27477=CARTESIAN_POINT('Ctrl Pts',(-1.07779197578118,-3.78421264632109,
40.6030564146537));
#27478=CARTESIAN_POINT('Ctrl Pts',(-0.96598994866209,-3.81427416447574,
40.6089290650712));
#27479=CARTESIAN_POINT('Ctrl Pts',(-0.853263097909405,-3.83932690529812,
40.6148017154887));
#27480=CARTESIAN_POINT('Ctrl Pts',(-0.822135685109074,-3.84624475140267,
40.6164233381328));
#27481=CARTESIAN_POINT('Ctrl Pts',(-0.790937788482818,-3.85278099027465,
40.6180449607769));
#27482=CARTESIAN_POINT('Ctrl Pts',(-0.759679545227435,-3.85893456650447,
40.619666583421));
#27483=CARTESIAN_POINT('Ctrl Pts',(-0.646483380285604,-3.88121864767312,
40.6255390012275));
#27484=CARTESIAN_POINT('Ctrl Pts',(-0.532116263583732,-3.8985551698722,
40.6314114190341));
#27485=CARTESIAN_POINT('Ctrl Pts',(-0.417048635583041,-3.91082592754501,
40.6372838368406));
#27486=CARTESIAN_POINT('Ctrl Pts',(-0.30213013859324,-3.92308078195704,
40.6431486438219));
#27487=CARTESIAN_POINT('Ctrl Pts',(-0.186513342999179,-3.93028288460637,
40.6490134508033));
#27488=CARTESIAN_POINT('Ctrl Pts',(-0.0706796452800259,-3.93236485943803,
40.6548782577846));
#27489=CARTESIAN_POINT('Ctrl Pts',(0.0450349087417255,-3.9344446928015,
40.6607370323695));
#27490=CARTESIAN_POINT('Ctrl Pts',(0.160965510318117,-3.93141486618567,
40.6665958069543));
#27491=CARTESIAN_POINT('Ctrl Pts',(0.276625530107023,-3.92325978187693,
40.6724545815392));
#27492=CARTESIAN_POINT('Ctrl Pts',(0.396837860319034,-3.9147837182413,40.6785439540494));
#27493=CARTESIAN_POINT('Ctrl Pts',(0.516757419054958,-3.90077060884241,
40.6846333265596));
#27494=CARTESIAN_POINT('Ctrl Pts',(0.635837280804501,-3.88126267499884,
40.6907226990699));
#27495=CARTESIAN_POINT('Ctrl Pts',(0.750274971915399,-3.86251523210964,
40.6965746854607));
#27496=CARTESIAN_POINT('Ctrl Pts',(0.86393676234027,-3.83869342962096,40.7024266718516));
#27497=CARTESIAN_POINT('Ctrl Pts',(0.976343152373888,-3.80988753755444,
40.7082786582424));
#27498=CARTESIAN_POINT('Ctrl Pts',(1.08873241304881,-3.78108603515346,40.7141297528622));
#27499=CARTESIAN_POINT('Ctrl Pts',(1.19986625339821,-3.74730205591859,40.7199808474819));
#27500=CARTESIAN_POINT('Ctrl Pts',(1.30927737957966,-3.70867654875981,40.7258319421016));
#27501=CARTESIAN_POINT('Ctrl Pts',(1.41869832591295,-3.6700475747841,40.731683561884));
#27502=CARTESIAN_POINT('Ctrl Pts',(1.52639586089314,-3.62657634665328,40.7375351816664));
#27503=CARTESIAN_POINT('Ctrl Pts',(1.63192049055313,-3.57845280987647,40.7433868014488));
#27504=CARTESIAN_POINT('Ctrl Pts',(1.73748014350494,-3.53031330104956,40.7492403633653));
#27505=CARTESIAN_POINT('Ctrl Pts',(1.84086508121008,-3.47751858467989,40.7550939252818));
#27506=CARTESIAN_POINT('Ctrl Pts',(1.94164897260077,-3.42030528859609,40.7609474871984));
#27507=CARTESIAN_POINT('Ctrl Pts',(2.04254749510528,-3.36302691838422,40.7668077069281));
#27508=CARTESIAN_POINT('Ctrl Pts',(2.14083870667397,-3.30132014153676,40.7726679266578));
#27509=CARTESIAN_POINT('Ctrl Pts',(2.2361238351808,-3.23546583875279,40.7785281463875));
#27510=CARTESIAN_POINT('Ctrl Pts',(2.33147311131144,-3.16956720169435,40.7843923113202));
#27511=CARTESIAN_POINT('Ctrl Pts',(2.4238119461695,-3.09951572811584,40.7902564762529));
#27512=CARTESIAN_POINT('Ctrl Pts',(2.5127747104818,-3.02563253789404,40.7961206411856));
#27513=CARTESIAN_POINT('Ctrl Pts',(2.60186866387217,-2.95164039571144,40.8019934537182));
#27514=CARTESIAN_POINT('Ctrl Pts',(2.68757630562578,-2.87380553649343,40.8078662662508));
#27515=CARTESIAN_POINT('Ctrl Pts',(2.76956883811472,-2.79248589091223,40.8137390787833));
#27516=CARTESIAN_POINT('Ctrl Pts',(2.7921883257094,-2.77005203433296,40.8153592264504));
#27517=CARTESIAN_POINT('Ctrl Pts',(2.81452531070709,-2.74735315744052,40.8169793741174));
#27518=CARTESIAN_POINT('Ctrl Pts',(2.83657344498074,-2.7243971977724,40.8185995217844));
#27519=CARTESIAN_POINT('Ctrl Pts',(2.91546205128647,-2.64226037648168,40.8243964381981));
#27520=CARTESIAN_POINT('Ctrl Pts',(2.99092924005757,-2.55653868550325,40.8301933546118));
#27521=CARTESIAN_POINT('Ctrl Pts',(3.06262502772754,-2.46755282406211,40.8359902710255));
#27522=CARTESIAN_POINT('Ctrl Pts',(3.13420561239945,-2.37870994784167,40.8417778727755));
#27523=CARTESIAN_POINT('Ctrl Pts',(3.20202658929276,-2.28661366453194,40.8475654745255));
#27524=CARTESIAN_POINT('Ctrl Pts',(3.26577467118157,-2.1916214994996,40.8533530762755));
#27525=CARTESIAN_POINT('Ctrl Pts',(3.32946416229371,-2.09671664163891,40.8591353586485));
#27526=CARTESIAN_POINT('Ctrl Pts',(3.38908796031717,-1.99892154033182,40.8649176410214));
#27527=CARTESIAN_POINT('Ctrl Pts',(3.44437310944292,-1.89862657806808,40.8706999233944));
#27528=CARTESIAN_POINT('Ctrl Pts',(3.49962165888698,-1.7983980127256,40.876478377801));
#27529=CARTESIAN_POINT('Ctrl Pts',(3.55053706312625,-1.6956732461639,40.8822568322075));
#27530=CARTESIAN_POINT('Ctrl Pts',(3.59689024853921,-1.59087068612239,40.8880352866141));
#27531=CARTESIAN_POINT('Ctrl Pts',(3.64322465994652,-1.48611057330079,40.8938114006262));
#27532=CARTESIAN_POINT('Ctrl Pts',(3.68500035492406,-1.37927472836459,40.8995875146384));
#27533=CARTESIAN_POINT('Ctrl Pts',(3.72203509766008,-1.27080436408855,40.9053636286506));
#27534=CARTESIAN_POINT('Ctrl Pts',(3.75907629846722,-1.16231508488898,40.9111407498941));
#27535=CARTESIAN_POINT('Ctrl Pts',(3.79137474787259,-1.05219111583276,40.9169178711376));
#27536=CARTESIAN_POINT('Ctrl Pts',(3.81879724499092,-0.940891386744367,
40.9226949923812));
#27537=CARTESIAN_POINT('Ctrl Pts',(3.84622140628905,-0.829584903246992,
40.9284724642189));
#27538=CARTESIAN_POINT('Ctrl Pts',(3.86876893300363,-0.717102932663289,
40.9342499360566));
#27539=CARTESIAN_POINT('Ctrl Pts',(3.8863575033137,-0.603915852116282,40.9400274078944));
#27540=CARTESIAN_POINT('Ctrl Pts',(3.90396114259419,-0.490631798777366,
40.9458098295689));
#27541=CARTESIAN_POINT('Ctrl Pts',(3.91659728308609,-0.376641850685132,
40.9515922512434));
#27542=CARTESIAN_POINT('Ctrl Pts',(3.92423538306663,-0.2624226710631,40.9573746729179));
#27543=CARTESIAN_POINT('Ctrl Pts',(3.93016269280269,-0.173786432058322,
40.961861941267));
#27544=CARTESIAN_POINT('Ctrl Pts',(3.93308120450337,-0.0850123104087433,
40.966349209616));
#27545=CARTESIAN_POINT('Ctrl Pts',(3.93299828088617,0.00367730151040331,
40.970836477965));
#27546=CARTESIAN_POINT('',(1.74869731696171,-3.52286058390776,41.9999376421029));
#27547=CARTESIAN_POINT('Ctrl Pts',(3.93299828088553,0.00367730219960045,
40.9708364779999));
#27548=CARTESIAN_POINT('Ctrl Pts',(3.93285383869511,0.158163078935381,40.9786527162416));
#27549=CARTESIAN_POINT('Ctrl Pts',(3.92360365029584,0.31224237002749,40.9864689544833));
#27550=CARTESIAN_POINT('Ctrl Pts',(3.9054123314799,0.46501991476143,40.9942851927251));
#27551=CARTESIAN_POINT('Ctrl Pts',(3.8873772938139,0.61648495155591,41.002034281866));
#27552=CARTESIAN_POINT('Ctrl Pts',(3.86055430226053,0.766671074542145,41.009783371007));
#27553=CARTESIAN_POINT('Ctrl Pts',(3.82514809528352,0.914730041678332,41.0175324601479));
#27554=CARTESIAN_POINT('Ctrl Pts',(3.79831164379733,1.02695266104069,41.0234059516215));
#27555=CARTESIAN_POINT('Ctrl Pts',(3.76648749677485,1.13818108591094,41.0292794430952));
#27556=CARTESIAN_POINT('Ctrl Pts',(3.72976395877152,1.2479382243721,41.0351529345688));
#27557=CARTESIAN_POINT('Ctrl Pts',(3.69308805402098,1.35755299938448,41.0410188076723));
#27558=CARTESIAN_POINT('Ctrl Pts',(3.65152552588073,1.46569989484038,41.0468846807759));
#27559=CARTESIAN_POINT('Ctrl Pts',(3.60521545744127,1.57191300822485,41.0527505538794));
#27560=CARTESIAN_POINT('Ctrl Pts',(3.55895308211299,1.67801673645841,41.0586103859265));
#27561=CARTESIAN_POINT('Ctrl Pts',(3.50795305583398,1.78219026741922,41.0644702179736));
#27562=CARTESIAN_POINT('Ctrl Pts',(3.45240372207426,1.88398448502311,41.0703300500206));
#27563=CARTESIAN_POINT('Ctrl Pts',(3.39468220674908,1.98975922782837,41.0764190228744));
#27564=CARTESIAN_POINT('Ctrl Pts',(3.33204847832998,2.09296434917749,41.0825079957282));
#27565=CARTESIAN_POINT('Ctrl Pts',(3.26476834986139,2.19312029349585,41.0885969685819));
#27566=CARTESIAN_POINT('Ctrl Pts',(3.20009542808786,2.28939504355196,41.0944499845321));
#27567=CARTESIAN_POINT('Ctrl Pts',(3.13112976417696,2.38285216241336,41.1003030004822));
#27568=CARTESIAN_POINT('Ctrl Pts',(3.05815299369713,2.4730930567088,41.1061560164323));
#27569=CARTESIAN_POINT('Ctrl Pts',(2.98518749119529,2.56332001735927,41.1120081286476));
#27570=CARTESIAN_POINT('Ctrl Pts',(2.90821237333455,2.65033141965462,41.1178602408628));
#27571=CARTESIAN_POINT('Ctrl Pts',(2.82755028482658,2.73376085032636,41.123712353078));
#27572=CARTESIAN_POINT('Ctrl Pts',(2.74688113675843,2.81719758275656,41.1295649774711));
#27573=CARTESIAN_POINT('Ctrl Pts',(2.66252466381531,2.89705142328491,41.1354176018642));
#27574=CARTESIAN_POINT('Ctrl Pts',(2.57484066466697,2.97299252464202,41.1412702262573));
#27575=CARTESIAN_POINT('Ctrl Pts',(2.48712777846706,3.04895864441221,41.1471247787681));
#27576=CARTESIAN_POINT('Ctrl Pts',(2.39608549844132,3.12100919146258,41.1529793312788));
#27577=CARTESIAN_POINT('Ctrl Pts',(2.3021064437128,3.18885479785706,41.1588338837895));
#27578=CARTESIAN_POINT('Ctrl Pts',(2.20802092745584,3.25677726123819,41.1646950684654));
#27579=CARTESIAN_POINT('Ctrl Pts',(2.11099233141337,3.32048503420083,41.1705562531412));
#27580=CARTESIAN_POINT('Ctrl Pts',(2.01144205714743,3.37973221583286,41.176417437817));
#27581=CARTESIAN_POINT('Ctrl Pts',(1.91182500794981,3.43901913845541,41.1822825539758));
#27582=CARTESIAN_POINT('Ctrl Pts',(1.80968327565849,3.49383931701827,41.1881476701346));
#27583=CARTESIAN_POINT('Ctrl Pts',(1.70546107652955,3.54399372409753,41.1940127862934));
#27584=CARTESIAN_POINT('Ctrl Pts',(1.60108569834002,3.59422184488677,41.1998865226213));
#27585=CARTESIAN_POINT('Ctrl Pts',(1.49462412910148,3.63977034598794,41.2057602589493));
#27586=CARTESIAN_POINT('Ctrl Pts',(1.38653874719456,3.6804890031799,41.2116339952772));
#27587=CARTESIAN_POINT('Ctrl Pts',(1.35690377355658,3.69165329118229,41.2132444630219));
#27588=CARTESIAN_POINT('Ctrl Pts',(1.327146803713,3.70245478722107,41.2148549307666));
#27589=CARTESIAN_POINT('Ctrl Pts',(1.29727751869983,3.71289106216113,41.2164653985113));
#27590=CARTESIAN_POINT('Ctrl Pts',(1.18833940384668,3.75095384530303,41.2223390349262));
#27591=CARTESIAN_POINT('Ctrl Pts',(1.07754295601843,3.78428161568497,41.228212671341));
#27592=CARTESIAN_POINT('Ctrl Pts',(0.965337447573294,3.81269099355202,41.2340863077559));
#27593=CARTESIAN_POINT('Ctrl Pts',(0.853277037124245,3.84106363397314,41.239952348707));
#27594=CARTESIAN_POINT('Ctrl Pts',(0.739811586491714,3.86453042970389,41.2458183896581));
#27595=CARTESIAN_POINT('Ctrl Pts',(0.625408373353521,3.88295678144108,41.2516844306092));
#27596=CARTESIAN_POINT('Ctrl Pts',(0.511122540017522,3.90136422740228,41.2575444528943));
#27597=CARTESIAN_POINT('Ctrl Pts',(0.395901263452485,3.91474145074433,41.2634044751794));
#27598=CARTESIAN_POINT('Ctrl Pts',(0.280224296749863,3.92300437719754,41.2692644974645));
#27599=CARTESIAN_POINT('Ctrl Pts',(0.160029082088124,3.93159004681775,41.27535340744));
#27600=CARTESIAN_POINT('Ctrl Pts',(0.0393422945093155,3.93465364349232,
41.2814423174154));
#27601=CARTESIAN_POINT('Ctrl Pts',(-0.0812889261354467,3.93215985311988,
41.2875312273908));
#27602=CARTESIAN_POINT('Ctrl Pts',(-0.197251541468887,3.92976257609544,
41.2933844876124));
#27603=CARTESIAN_POINT('Ctrl Pts',(-0.31316235941206,3.92223008221031,41.299237747834));
#27604=CARTESIAN_POINT('Ctrl Pts',(-0.428533760636677,3.90958409757286,
41.3050910080556));
#27605=CARTESIAN_POINT('Ctrl Pts',(-0.54388773069462,3.89694002358453,41.3109433839232));
#27606=CARTESIAN_POINT('Ctrl Pts',(-0.658702035494459,3.87918404001055,
41.3167957597908));
#27607=CARTESIAN_POINT('Ctrl Pts',(-0.772493990199379,3.85638976701083,
41.3226481356584));
#27608=CARTESIAN_POINT('Ctrl Pts',(-0.886296273008748,3.83359342513345,
41.3285010427055));
#27609=CARTESIAN_POINT('Ctrl Pts',(-0.999075616123448,3.80575796591518,
41.3343539497526));
#27610=CARTESIAN_POINT('Ctrl Pts',(-1.11036004185059,3.77300802774942,41.3402068567997));
#27611=CARTESIAN_POINT('Ctrl Pts',(-1.22168148223857,3.74024719652431,41.3460617106005));
#27612=CARTESIAN_POINT('Ctrl Pts',(-1.33150662037376,3.70256875254571,41.3519165644013));
#27613=CARTESIAN_POINT('Ctrl Pts',(-1.43937981899881,3.66014681900316,41.3577714182021));
#27614=CARTESIAN_POINT('Ctrl Pts',(-1.5473756888414,3.61767664409663,41.3636329300241));
#27615=CARTESIAN_POINT('Ctrl Pts',(-1.65341480395904,3.57045236420457,41.3694944418461));
#27616=CARTESIAN_POINT('Ctrl Pts',(-1.75706256052522,3.51869580361823,41.3753559536681));
#27617=CARTESIAN_POINT('Ctrl Pts',(-1.86078010940055,3.4669043922064,41.3812214124009));
#27618=CARTESIAN_POINT('Ctrl Pts',(-1.96210273312705,3.41057482342103,41.3870868711337));
#27619=CARTESIAN_POINT('Ctrl Pts',(-2.06062295316566,3.34997343943006,41.3929523298664));
#27620=CARTESIAN_POINT('Ctrl Pts',(-2.15928829598066,3.28928278806742,41.3988264285683));
#27621=CARTESIAN_POINT('Ctrl Pts',(-2.25514265560694,3.22430799375315,41.4047005272701));
#27622=CARTESIAN_POINT('Ctrl Pts',(-2.34780981417076,3.15535704421599,41.410574625972));
#27623=CARTESIAN_POINT('Ctrl Pts',(-2.37317538403825,3.13648325813017,41.4121825296062));
#27624=CARTESIAN_POINT('Ctrl Pts',(-2.39830235271441,3.11731177138596,41.4137904332405));
#27625=CARTESIAN_POINT('Ctrl Pts',(-2.4231834817654,3.09784938525089,41.4153983368747));
#27626=CARTESIAN_POINT('Ctrl Pts',(-2.5139243099458,3.02687057104019,41.421262319458));
#27627=CARTESIAN_POINT('Ctrl Pts',(-2.60169853262691,2.95178047655881,41.4271263020412));
#27628=CARTESIAN_POINT('Ctrl Pts',(-2.68610962259956,2.87285643487071,41.4329902846244));
#27629=CARTESIAN_POINT('Ctrl Pts',(-2.77041086511586,2.79403510012819,41.4388466361775));
#27630=CARTESIAN_POINT('Ctrl Pts',(-2.85135737773794,2.71139001988999,41.4447029877306));
#27631=CARTESIAN_POINT('Ctrl Pts',(-2.92858385142488,2.62524010809933,41.4505593392837));
#27632=CARTESIAN_POINT('Ctrl Pts',(-3.00573063919795,2.53917908984638,41.4564096479774));
#27633=CARTESIAN_POINT('Ctrl Pts',(-3.07916474743663,2.44962073974177,41.4622599566711));
#27634=CARTESIAN_POINT('Ctrl Pts',(-3.14855656489229,2.35692183953428,41.4681102653647));
#27635=CARTESIAN_POINT('Ctrl Pts',(-3.22082156659725,2.26038471992616,41.4742028074428));
#27636=CARTESIAN_POINT('Ctrl Pts',(-3.28870197815474,2.16044168279813,41.4802953495208));
#27637=CARTESIAN_POINT('Ctrl Pts',(-3.35187063466801,2.05753547926888,41.4863878915989));
#27638=CARTESIAN_POINT('Ctrl Pts',(-3.41245765236363,1.95883494773385,41.4922314376717));
#27639=CARTESIAN_POINT('Ctrl Pts',(-3.46871023004299,1.85740907706089,41.4980749837446));
#27640=CARTESIAN_POINT('Ctrl Pts',(-3.52038354497778,1.75367861829061,41.5039185298174));
#27641=CARTESIAN_POINT('Ctrl Pts',(-3.57204917985033,1.64996357669225,41.5097612073801));
#27642=CARTESIAN_POINT('Ctrl Pts',(-3.61913672024701,1.54394499904711,41.5156038849428));
#27643=CARTESIAN_POINT('Ctrl Pts',(-3.66144766340146,1.43606755000314,41.5214465625056));
#27644=CARTESIAN_POINT('Ctrl Pts',(-3.70376264035098,1.32817981625524,41.5272897970912));
#27645=CARTESIAN_POINT('Ctrl Pts',(-3.74129996337929,1.21843324488357,41.5331330316768));
#27646=CARTESIAN_POINT('Ctrl Pts',(-3.77390984208486,1.10729106553562,41.5389762662624));
#27647=CARTESIAN_POINT('Ctrl Pts',(-3.8065307854242,0.996111175298837,41.5448214834757));
#27648=CARTESIAN_POINT('Ctrl Pts',(-3.83422084347951,0.883535133223119,
41.5506667006891));
#27649=CARTESIAN_POINT('Ctrl Pts',(-3.85688069745533,0.77003914549617,41.5565119179025));
#27650=CARTESIAN_POINT('Ctrl Pts',(-3.87956675613467,0.656411906759731,
41.5623638947439));
#27651=CARTESIAN_POINT('Ctrl Pts',(-3.89721091892512,0.541863005858298,
41.5682158715852));
#27652=CARTESIAN_POINT('Ctrl Pts',(-3.90976537386394,0.426876705073691,
41.5740678484266));
#27653=CARTESIAN_POINT('Ctrl Pts',(-3.92232839714301,0.311811926827965,
41.5799238192072));
#27654=CARTESIAN_POINT('Ctrl Pts',(-3.92979476977478,0.196309567073772,
41.5857797899877));
#27655=CARTESIAN_POINT('Ctrl Pts',(-3.93216879837236,0.0808550623451563,
41.5916357607682));
#27656=CARTESIAN_POINT('Ctrl Pts',(-3.93454638763816,-0.0347726059187965,
41.5975005145806));
#27657=CARTESIAN_POINT('Ctrl Pts',(-3.9318163996028,-0.150351862985736,
41.6033652683931));
#27658=CARTESIAN_POINT('Ctrl Pts',(-3.92403507123059,-0.26540112990027,
41.6092300222056));
#27659=CARTESIAN_POINT('Ctrl Pts',(-3.92177896488034,-0.298758336955588,
41.6109304398831));
#27660=CARTESIAN_POINT('Ctrl Pts',(-3.91909855040044,-0.332071051361949,
41.6126308575607));
#27661=CARTESIAN_POINT('Ctrl Pts',(-3.91599599938462,-0.36532770604443,
41.6143312752382));
#27662=CARTESIAN_POINT('Ctrl Pts',(-3.90526104620493,-0.480397088983917,
41.6202147898239));
#27663=CARTESIAN_POINT('Ctrl Pts',(-3.88943223306831,-0.595182622947716,
41.6260983044096));
#27664=CARTESIAN_POINT('Ctrl Pts',(-3.86853032292968,-0.709198237852823,
41.6319818189952));
#27665=CARTESIAN_POINT('Ctrl Pts',(-3.84765556061053,-0.823065766994018,
41.6378576919544));
#27666=CARTESIAN_POINT('Ctrl Pts',(-3.82172087916518,-0.936164964568238,
41.6437335649135));
#27667=CARTESIAN_POINT('Ctrl Pts',(-3.79079888577828,-1.04801374398534,
41.6496094378726));
#27668=CARTESIAN_POINT('Ctrl Pts',(-3.75990886633242,-1.15974686959469,
41.6554792350651));
#27669=CARTESIAN_POINT('Ctrl Pts',(-3.72404190230729,-1.27023175454549,
41.6613490322575));
#27670=CARTESIAN_POINT('Ctrl Pts',(-3.68332172739711,-1.37899603062677,
41.66721882945));
#27671=CARTESIAN_POINT('Ctrl Pts',(-3.64110708328714,-1.49175205922383,
41.6733040537897));
#27672=CARTESIAN_POINT('Ctrl Pts',(-3.59367623703547,-1.60265831580807,
41.6793892781293));
#27673=CARTESIAN_POINT('Ctrl Pts',(-3.54122397187539,-1.71120477471723,
41.685474502469));
#27674=CARTESIAN_POINT('Ctrl Pts',(-3.49068863748631,-1.81578427344784,
41.6913373350063));
#27675=CARTESIAN_POINT('Ctrl Pts',(-3.43549267616954,-1.91817303245174,
41.6972001675436));
#27676=CARTESIAN_POINT('Ctrl Pts',(-3.37585917784821,-2.0179355320074,41.703063000081));
#27677=CARTESIAN_POINT('Ctrl Pts',(-3.31623560038966,-2.11768143468218,
41.7089248572545));
#27678=CARTESIAN_POINT('Ctrl Pts',(-3.25217616516896,-2.21480159349513,
41.714786714428));
#27679=CARTESIAN_POINT('Ctrl Pts',(-3.18394911200897,-2.30888653946817,
41.7206485716015));
#27680=CARTESIAN_POINT('Ctrl Pts',(-3.11571705126772,-2.402978390884,41.7265108590108));
#27681=CARTESIAN_POINT('Ctrl Pts',(-3.04331700627884,-2.49403425335169,
41.7323731464202));
#27682=CARTESIAN_POINT('Ctrl Pts',(-2.96705918382821,-2.58167557986295,
41.7382354338296));
#27683=CARTESIAN_POINT('Ctrl Pts',(-2.89077748099677,-2.66934435153568,
41.744099557033));
#27684=CARTESIAN_POINT('Ctrl Pts',(-2.81063586852203,-2.75359615052861,
41.7499636802364));
#27685=CARTESIAN_POINT('Ctrl Pts',(-2.72698280046746,-2.83408782608349,
41.7558278034398));
#27686=CARTESIAN_POINT('Ctrl Pts',(-2.64323775706398,-2.91466800108155,
41.7616983741626));
#27687=CARTESIAN_POINT('Ctrl Pts',(-2.55597384866479,-2.99147951499695,
41.7675689448854));
#27688=CARTESIAN_POINT('Ctrl Pts',(-2.46557420551259,-3.06421814450456,
41.7734395156082));
#27689=CARTESIAN_POINT('Ctrl Pts',(-2.37511550448373,-3.13700429398968,
41.7793139215612));
#27690=CARTESIAN_POINT('Ctrl Pts',(-2.28151732014737,-3.20571201698357,
41.7851883275142));
#27691=CARTESIAN_POINT('Ctrl Pts',(-2.18519207308076,-3.27008021365608,
41.7910627334672));
#27692=CARTESIAN_POINT('Ctrl Pts',(-2.08872895754162,-3.33454053928985,
41.7969455473444));
#27693=CARTESIAN_POINT('Ctrl Pts',(-1.98953133977585,-3.39464872925959,
41.8028283612216));
#27694=CARTESIAN_POINT('Ctrl Pts',(-1.8880365988769,-3.45018938629481,41.8087111750988));
#27695=CARTESIAN_POINT('Ctrl Pts',(-1.86185244773223,-3.46451805934332,
41.8102288545998));
#27696=CARTESIAN_POINT('Ctrl Pts',(-1.83551551169213,-3.47854298330307,
41.8117465341007));
#27697=CARTESIAN_POINT('Ctrl Pts',(-1.80903350294568,-3.4922609846946,41.8132642136017));
#27698=CARTESIAN_POINT('Ctrl Pts',(-1.70742103092262,-3.54489747635787,
41.8190876074124));
#27699=CARTESIAN_POINT('Ctrl Pts',(-1.60332774807853,-3.59318933627977,
41.8249110012232));
#27700=CARTESIAN_POINT('Ctrl Pts',(-1.49716503359537,-3.63689233579706,
41.8307343950339));
#27701=CARTESIAN_POINT('Ctrl Pts',(-1.39113820063262,-3.68053939825537,
41.8365503352711));
#27702=CARTESIAN_POINT('Ctrl Pts',(-1.28304758713599,-3.71960911780812,
41.8423662755082));
#27703=CARTESIAN_POINT('Ctrl Pts',(-1.17332958763058,-3.75390285953042,
41.8481822157454));
#27704=CARTESIAN_POINT('Ctrl Pts',(-1.06372144601052,-3.78816226378791,
41.8539923326272));
#27705=CARTESIAN_POINT('Ctrl Pts',(-0.952489557777298,-3.81765507416629,
41.859802449509));
#27706=CARTESIAN_POINT('Ctrl Pts',(-0.840090023954876,-3.84223083008446,
41.8656125663909));
#27707=CARTESIAN_POINT('Ctrl Pts',(-0.727768808379918,-3.86678946199802,
41.8714186348736));
#27708=CARTESIAN_POINT('Ctrl Pts',(-0.614281974956971,-3.88643776297211,
41.8772247033564));
#27709=CARTESIAN_POINT('Ctrl Pts',(-0.500099795513575,-3.90107538949548,
41.8830307718391));
#27710=CARTESIAN_POINT('Ctrl Pts',(-0.385958726636555,-3.91570774583465,
41.8888347498838));
#27711=CARTESIAN_POINT('Ctrl Pts',(-0.271123226235575,-3.92533295960325,
41.8946387279286));
#27712=CARTESIAN_POINT('Ctrl Pts',(-0.15607206147564,-3.92990209949647,
41.9004427059734));
#27713=CARTESIAN_POINT('Ctrl Pts',(-0.0410333161247926,-3.9344707461655,
41.9062460574971));
#27714=CARTESIAN_POINT('Ctrl Pts',(0.0742206267747902,-3.93398438758145,
41.9120494090208));
#27715=CARTESIAN_POINT('Ctrl Pts',(0.18920841364813,-3.92844615289617,41.9178527605445));
#27716=CARTESIAN_POINT('Ctrl Pts',(0.304212776840347,-3.92290711983442,
41.9236569486632));
#27717=CARTESIAN_POINT('Ctrl Pts',(0.418950487396495,-3.91231478424112,
41.9294611367818));
#27718=CARTESIAN_POINT('Ctrl Pts',(0.532943549870492,-3.89672428748192,
41.9352653249005));
#27719=CARTESIAN_POINT('Ctrl Pts',(0.647049319293432,-3.88111837612393,
41.9410752517222));
#27720=CARTESIAN_POINT('Ctrl Pts',(0.760408552861537,-3.86050449312197,
41.946885178544));
#27721=CARTESIAN_POINT('Ctrl Pts',(0.872551680866595,-3.83498925216445,
41.9526951053657));
#27722=CARTESIAN_POINT('Ctrl Pts',(0.984753634335691,-3.80946062700841,
41.9585080798253));
#27723=CARTESIAN_POINT('Ctrl Pts',(1.0957378064602,-3.77902563596717,41.9643210542848));
#27724=CARTESIAN_POINT('Ctrl Pts',(1.20504985637141,-3.74384078770175,41.9701340287444));
#27725=CARTESIAN_POINT('Ctrl Pts',(1.31452994394932,-3.70860185226286,41.9759559390776));
#27726=CARTESIAN_POINT('Ctrl Pts',(1.42233238172794,-3.66859862421664,41.9817778494108));
#27727=CARTESIAN_POINT('Ctrl Pts',(1.52802263117264,-3.62403584952249,41.987599759744));
#27728=CARTESIAN_POINT('Ctrl Pts',(1.60268276788032,-3.59255647589797,41.991712387197));
#27729=CARTESIAN_POINT('Ctrl Pts',(1.67628935708178,-3.55880285359254,41.99582501465));
#27730=CARTESIAN_POINT('Ctrl Pts',(1.74869731696171,-3.52286058390776,41.9999376421029));
#27731=CARTESIAN_POINT('',(-1.7486944753309,-3.52286199445099,42.));
#27732=CARTESIAN_POINT('Origin',(0.,0.,42.));
#27733=CARTESIAN_POINT('',(3.93228009845805,0.00389650693369247,41.1541638748943));
#27734=CARTESIAN_POINT('Ctrl Pts',(-1.7486944753309,-3.52286199445099,42.));
#27735=CARTESIAN_POINT('Ctrl Pts',(-2.92291840980274,-2.93999530530831,
41.9336890205455));
#27736=CARTESIAN_POINT('Ctrl Pts',(-4.621982019705,-0.51750383458989,41.8010670616367));
#27737=CARTESIAN_POINT('Ctrl Pts',(-2.92991200205014,3.61782035329863,41.602134123273));
#27738=CARTESIAN_POINT('Ctrl Pts',(1.45961866169696,4.41606836987815,41.4032011849098));
#27739=CARTESIAN_POINT('Ctrl Pts',(3.74575420314252,1.97212767892205,41.2538777887601));
#27740=CARTESIAN_POINT('Ctrl Pts',(3.93515403968839,0.334151972648519,41.1708653720651));
#27741=CARTESIAN_POINT('Ctrl Pts',(3.93215815619892,0.00389757136549701,
41.1541639348245));
#27742=CARTESIAN_POINT('',(3.93299992557056,-0.000765154855056892,39.9041635219977));
#27743=CARTESIAN_POINT('Ctrl Pts',(3.93299807602736,0.00389023972029836,
41.1541635220349));
#27744=CARTESIAN_POINT('Ctrl Pts',(3.93311122308255,-0.110500436017224,
41.1483798001704));
#27745=CARTESIAN_POINT('Ctrl Pts',(3.92822960554725,-0.22502150371433,41.142596078306));
#27746=CARTESIAN_POINT('Ctrl Pts',(3.91834595805662,-0.339196039159292,
41.1368123564415));
#27747=CARTESIAN_POINT('Ctrl Pts',(3.90846841189372,-0.453300092906078,
41.1310322049576));
#27748=CARTESIAN_POINT('Ctrl Pts',(3.89359501003231,-0.567057617791912,
41.1252520534736));
#27749=CARTESIAN_POINT('Ctrl Pts',(3.87377055495045,-0.679993152611765,
41.1194719019897));
#27750=CARTESIAN_POINT('Ctrl Pts',(3.85395218492908,-0.792894022188202,
41.113693524707));
#27751=CARTESIAN_POINT('Ctrl Pts',(3.8291858546012,-0.90497298515588,41.1079151474242));
#27752=CARTESIAN_POINT('Ctrl Pts',(3.79956795898915,-1.01576194308659,41.1021367701414));
#27753=CARTESIAN_POINT('Ctrl Pts',(3.76995155801667,-1.1265453101555,41.0963586844591));
#27754=CARTESIAN_POINT('Ctrl Pts',(3.73548418844761,-1.23603839142066,41.0905805987768));
#27755=CARTESIAN_POINT('Ctrl Pts',(3.69631266180428,-1.34378633204291,41.0848025130945));
#27756=CARTESIAN_POINT('Ctrl Pts',(3.65713306433753,-1.45155647283649,41.0790232369069));
#27757=CARTESIAN_POINT('Ctrl Pts',(3.61324752952121,-1.55758035968635,41.0732439607192));
#27758=CARTESIAN_POINT('Ctrl Pts',(3.56485142260143,-1.66142208206602,41.0674646845316));
#27759=CARTESIAN_POINT('Ctrl Pts',(3.51640383488079,-1.76537426488084,41.0616792607056));
#27760=CARTESIAN_POINT('Ctrl Pts',(3.4634362768292,-1.86713926420627,41.0558938368796));
#27761=CARTESIAN_POINT('Ctrl Pts',(3.4061905932739,-1.96630481927202,41.0501084130536));
#27762=CARTESIAN_POINT('Ctrl Pts',(3.34891136462435,-2.06552848383504,41.0443195990577));
#27763=CARTESIAN_POINT('Ctrl Pts',(3.28734924928495,-2.16214931524564,41.0385307850619));
#27764=CARTESIAN_POINT('Ctrl Pts',(3.22178896106807,-2.25578476152755,41.0327419710661));
#27765=CARTESIAN_POINT('Ctrl Pts',(3.15612629068068,-2.34956643352762,41.0269441169736));
#27766=CARTESIAN_POINT('Ctrl Pts',(3.08645324145257,-2.44035307775196,41.0211462628811));
#27767=CARTESIAN_POINT('Ctrl Pts',(3.01309433601815,-2.52779578333681,41.0153484087886));
#27768=CARTESIAN_POINT('Ctrl Pts',(2.97086318815253,-2.57813467276619,41.0120107085867));
#27769=CARTESIAN_POINT('Ctrl Pts',(2.92741121452159,-2.62736604230084,41.0086730083847));
#27770=CARTESIAN_POINT('Ctrl Pts',(2.88280549253714,-2.67542921644317,41.0053353081828));
#27771=CARTESIAN_POINT('Ctrl Pts',(2.80430807862628,-2.76001107515256,40.999461603586));
#27772=CARTESIAN_POINT('Ctrl Pts',(2.72195391264452,-2.84127661989262,40.9935878989893));
#27773=CARTESIAN_POINT('Ctrl Pts',(2.63605432670703,-2.91885364255372,40.9877141943925));
#27774=CARTESIAN_POINT('Ctrl Pts',(2.55026600203703,-2.99633018373084,40.9818480976999));
#27775=CARTESIAN_POINT('Ctrl Pts',(2.46094169355245,-3.07012742940372,40.9759820010073));
#27776=CARTESIAN_POINT('Ctrl Pts',(2.36843146370396,-3.13990786516692,40.9701159043147));
#27777=CARTESIAN_POINT('Ctrl Pts',(2.27601634556961,-3.20961655819562,40.9642558386796));
#27778=CARTESIAN_POINT('Ctrl Pts',(2.18042214917457,-3.27531640841443,40.9583957730444));
#27779=CARTESIAN_POINT('Ctrl Pts',(2.0820335956378,-3.336708723673,40.9525357074093));
#27780=CARTESIAN_POINT('Ctrl Pts',(1.97980317277675,-3.40049828174347,40.9464468183431));
#27781=CARTESIAN_POINT('Ctrl Pts',(1.87455605503832,-3.45963674409439,40.9403579292768));
#27782=CARTESIAN_POINT('Ctrl Pts',(1.76675931968063,-3.51383700622576,40.9342690402106));
#27783=CARTESIAN_POINT('Ctrl Pts',(1.66313390444639,-3.56593992613824,40.9284157677927));
#27784=CARTESIAN_POINT('Ctrl Pts',(1.55715292797622,-3.61347951740685,40.9225624953748));
#27785=CARTESIAN_POINT('Ctrl Pts',(1.44925754859986,-3.65624692243649,40.916709222957));
#27786=CARTESIAN_POINT('Ctrl Pts',(1.34137868292838,-3.69900778178912,40.9108568463997));
#27787=CARTESIAN_POINT('Ctrl Pts',(1.23158638092573,-3.73699775498812,40.9050044698423));
#27788=CARTESIAN_POINT('Ctrl Pts',(1.12034171211492,-3.77005615980656,40.899152093285));
#27789=CARTESIAN_POINT('Ctrl Pts',(1.00908716513153,-3.80311750010616,40.8932991970553));
#27790=CARTESIAN_POINT('Ctrl Pts',(0.89638039103105,-3.83124628380499,40.8874463008256));
#27791=CARTESIAN_POINT('Ctrl Pts',(0.78269685867274,-3.8543319301046,40.8815934045958));
#27792=CARTESIAN_POINT('Ctrl Pts',(0.668975737292473,-3.8774252095842,40.8757385731285));
#27793=CARTESIAN_POINT('Ctrl Pts',(0.554277620140873,-3.89547195374573,
40.8698837416612));
#27794=CARTESIAN_POINT('Ctrl Pts',(0.439086679126237,-3.90841296285511,
40.8640289101939));
#27795=CARTESIAN_POINT('Ctrl Pts',(0.323765078495354,-3.92136865078619,
40.8581674376658));
#27796=CARTESIAN_POINT('Ctrl Pts',(0.207949949061725,-3.92920699804321,
40.8523059651378));
#27797=CARTESIAN_POINT('Ctrl Pts',(0.0921291821830041,-3.93192080461831,
40.8464444926098));
#27798=CARTESIAN_POINT('Ctrl Pts',(-0.0237693783711899,-3.93463643398386,
40.8405790830892));
#27799=CARTESIAN_POINT('Ctrl Pts',(-0.139673171838126,-3.93222067739507,
40.8347136735687));
#27800=CARTESIAN_POINT('Ctrl Pts',(-0.255097458942097,-3.92471837033452,
40.8288482640481));
#27801=CARTESIAN_POINT('Ctrl Pts',(-0.370691491350461,-3.91720503022861,
40.822974228737));
#27802=CARTESIAN_POINT('Ctrl Pts',(-0.485804200819735,-3.90459025494561,
40.817100193426));
#27803=CARTESIAN_POINT('Ctrl Pts',(-0.59995899977985,-3.88697031099842,
40.8112261581149));
#27804=CARTESIAN_POINT('Ctrl Pts',(-0.631207170979042,-3.88214711451437,
40.809618228683));
#27805=CARTESIAN_POINT('Ctrl Pts',(-0.662383643985488,-3.87694916719674,
40.8080102992512));
#27806=CARTESIAN_POINT('Ctrl Pts',(-0.693478838898908,-3.87137909536116,
40.8064023698194));
#27807=CARTESIAN_POINT('Ctrl Pts',(-0.807061393191453,-3.85103309050611,
40.80052902725));
#27808=CARTESIAN_POINT('Ctrl Pts',(-0.919937276006077,-3.82565030150215,
40.7946556846807));
#27809=CARTESIAN_POINT('Ctrl Pts',(-1.03162511240368,-3.79529163931549,
40.7887823421113));
#27810=CARTESIAN_POINT('Ctrl Pts',(-1.14316862030515,-3.76497220808003,
40.7829165893631));
#27811=CARTESIAN_POINT('Ctrl Pts',(-1.25352673979851,-3.72968979828012,
40.7770508366148));
#27812=CARTESIAN_POINT('Ctrl Pts',(-1.36222637023903,-3.68955665578202,
40.7711850838666));
#27813=CARTESIAN_POINT('Ctrl Pts',(-1.47081457925781,-3.64946465134279,
40.765325343747));
#27814=CARTESIAN_POINT('Ctrl Pts',(-1.57774729535856,-3.60453194651736,
40.7594656036273));
#27815=CARTESIAN_POINT('Ctrl Pts',(-1.6825653666707,-3.55492092554536,40.7536058635077));
#27816=CARTESIAN_POINT('Ctrl Pts',(-1.79148472318545,-3.50336874172185,
40.7475168455056));
#27817=CARTESIAN_POINT('Ctrl Pts',(-1.89812013501853,-3.44676478256776,
40.7414278275034));
#27818=CARTESIAN_POINT('Ctrl Pts',(-2.00197761118039,-3.38534704931894,
40.7353388095013));
#27819=CARTESIAN_POINT('Ctrl Pts',(-2.10180936321883,-3.32630999062031,
40.729485814052));
#27820=CARTESIAN_POINT('Ctrl Pts',(-2.1990741372511,-3.26282562168927,40.7236328186027));
#27821=CARTESIAN_POINT('Ctrl Pts',(-2.29335789691542,-3.19515235265169,
40.7177798231534));
#27822=CARTESIAN_POINT('Ctrl Pts',(-2.38762752339369,-3.12748922787338,
40.7119277050713));
#27823=CARTESIAN_POINT('Ctrl Pts',(-2.47891668839842,-3.05563869237956,
40.7060755869892));
#27824=CARTESIAN_POINT('Ctrl Pts',(-2.5668411441862,-2.9799019347141,40.700223468907));
#27825=CARTESIAN_POINT('Ctrl Pts',(-2.65477369118737,-2.90415820740338,
40.6943708122861));
#27826=CARTESIAN_POINT('Ctrl Pts',(-2.7393406003306,-2.82452781666461,40.6885181556651));
#27827=CARTESIAN_POINT('Ctrl Pts',(-2.82019201104604,-2.74135113052526,
40.6826654990441));
#27828=CARTESIAN_POINT('Ctrl Pts',(-2.9010704220475,-2.65814666757537,40.6768108879315));
#27829=CARTESIAN_POINT('Ctrl Pts',(-2.97823057949439,-2.57139385045657,
40.6709562768189));
#27830=CARTESIAN_POINT('Ctrl Pts',(-3.05136116400601,-2.48146812326813,
40.6651016657063));
#27831=CARTESIAN_POINT('Ctrl Pts',(-3.12457507635168,-2.39143993120645,
40.659240383622));
#27832=CARTESIAN_POINT('Ctrl Pts',(-3.19374999046137,-2.29823193371721,
40.6533791015377));
#27833=CARTESIAN_POINT('Ctrl Pts',(-3.2586163394363,-2.20225079233923,40.6475178194533));
#27834=CARTESIAN_POINT('Ctrl Pts',(-3.32352644906473,-2.10620489939843,
40.6416525831841));
#27835=CARTESIAN_POINT('Ctrl Pts',(-3.38412199026311,-2.00738248872334,
40.635787346915));
#27836=CARTESIAN_POINT('Ctrl Pts',(-3.44017889227008,-1.90621567226255,
40.6299221106458));
#27837=CARTESIAN_POINT('Ctrl Pts',(-3.4963184910571,-1.80489961155763,40.6240482218087));
#27838=CARTESIAN_POINT('Ctrl Pts',(-3.54790590417778,-1.70123261100789,
40.6181743329715));
#27839=CARTESIAN_POINT('Ctrl Pts',(-3.59476474769179,-1.59566769997778,
40.6123004441344));
#27840=CARTESIAN_POINT('Ctrl Pts',(-3.60761118687321,-1.56672688310006,
40.6106901065749));
#27841=CARTESIAN_POINT('Ctrl Pts',(-3.62010251857552,-1.53764351164238,
40.6090797690154));
#27842=CARTESIAN_POINT('Ctrl Pts',(-3.63223576574945,-1.50842710861696,
40.6074694314559));
#27843=CARTESIAN_POINT('Ctrl Pts',(-3.67647145818702,-1.40190922434097,
40.6015984229797));
#27844=CARTESIAN_POINT('Ctrl Pts',(-3.71609204453458,-1.29326458447947,
40.5957274145035));
#27845=CARTESIAN_POINT('Ctrl Pts',(-3.75088844203362,-1.18293063846473,
40.5898564060273));
#27846=CARTESIAN_POINT('Ctrl Pts',(-3.78563962999961,-1.07274004482372,
40.5839930255118));
#27847=CARTESIAN_POINT('Ctrl Pts',(-3.81557897026632,-0.960864900513171,
40.5781296449963));
#27848=CARTESIAN_POINT('Ctrl Pts',(-3.84054502427604,-0.847763479107561,
40.5722662644808));
#27849=CARTESIAN_POINT('Ctrl Pts',(-3.86548532727636,-0.734778715134654,
40.5664089316958));
#27850=CARTESIAN_POINT('Ctrl Pts',(-3.88546245842252,-0.620570591278151,
40.5605515989107));
#27851=CARTESIAN_POINT('Ctrl Pts',(-3.90036469004281,-0.505612781352745,
40.5546942661257));
#27852=CARTESIAN_POINT('Ctrl Pts',(-3.91585863773476,-0.386090394427762,
40.548604358916));
#27853=CARTESIAN_POINT('Ctrl Pts',(-3.9258661880868,-0.265757987767407,
40.5425144517063));
#27854=CARTESIAN_POINT('Ctrl Pts',(-3.93032027697842,-0.145160326440494,
40.5364245444966));
#27855=CARTESIAN_POINT('Ctrl Pts',(-3.93459927735498,-0.0293033126295149,
40.5305740291886));
#27856=CARTESIAN_POINT('Ctrl Pts',(-3.93375315879367,0.0867980431762234,
40.5247235138806));
#27857=CARTESIAN_POINT('Ctrl Pts',(-3.92777539071006,0.202656063645884,
40.5188729985725));
#27858=CARTESIAN_POINT('Ctrl Pts',(-3.92179854230237,0.318496259430816,
40.5130233833627));
#27859=CARTESIAN_POINT('Ctrl Pts',(-3.91069163543769,0.43409278138595,40.5071737681528));
#27860=CARTESIAN_POINT('Ctrl Pts',(-3.89450023206756,0.548959873238225,
40.501324152943));
#27861=CARTESIAN_POINT('Ctrl Pts',(-3.87830739385005,0.663837144365366,
40.4954740193528));
#27862=CARTESIAN_POINT('Ctrl Pts',(-3.85702922116871,0.777984447321958,
40.4896238857626));
#27863=CARTESIAN_POINT('Ctrl Pts',(-3.83076282774209,0.890923766429782,
40.4837737521724));
#27864=CARTESIAN_POINT('Ctrl Pts',(-3.80448773790008,1.00390047808009,40.4779216816893));
#27865=CARTESIAN_POINT('Ctrl Pts',(-3.77322123704001,1.11566800799436,40.4720696112062));
#27866=CARTESIAN_POINT('Ctrl Pts',(-3.73711078392592,1.22576179931689,40.4662175407231));
#27867=CARTESIAN_POINT('Ctrl Pts',(-3.70095925018538,1.3359808375285,40.4603588127017));
#27868=CARTESIAN_POINT('Ctrl Pts',(-3.65995289405373,1.44452194337658,40.4545000846804));
#27869=CARTESIAN_POINT('Ctrl Pts',(-3.61428800787736,1.55093881120884,40.4486413566591));
#27870=CARTESIAN_POINT('Ctrl Pts',(-3.56859238718388,1.65742730236746,40.4427786854509));
#27871=CARTESIAN_POINT('Ctrl Pts',(-3.51823217262971,1.76178833713314,40.4369160142428));
#27872=CARTESIAN_POINT('Ctrl Pts',(-3.46344965982526,1.86360013250061,40.4310533430347));
#27873=CARTESIAN_POINT('Ctrl Pts',(-3.40858626068035,1.96556225291017,40.4251820155967));
#27874=CARTESIAN_POINT('Ctrl Pts',(-3.34928774270519,2.06496726793466,40.4193106881588));
#27875=CARTESIAN_POINT('Ctrl Pts',(-3.28583977385381,2.16142221247038,40.4134393607209));
#27876=CARTESIAN_POINT('Ctrl Pts',(-3.26817897534573,2.18827053198937,40.4118050715114));
#27877=CARTESIAN_POINT('Ctrl Pts',(-3.2501969195197,2.21489048117082,40.410170782302));
#27878=CARTESIAN_POINT('Ctrl Pts',(-3.23190030655268,2.24127405921379,40.4085364930925));
#27879=CARTESIAN_POINT('Ctrl Pts',(-3.1661558687843,2.33607704312568,40.4026640714907));
#27880=CARTESIAN_POINT('Ctrl Pts',(-3.09612640254298,2.42814361612027,40.3967916498889));
#27881=CARTESIAN_POINT('Ctrl Pts',(-3.02206731929664,2.51706140521824,40.3909192282871));
#27882=CARTESIAN_POINT('Ctrl Pts',(-2.94810422636286,2.60586394516656,40.3850544181161));
#27883=CARTESIAN_POINT('Ctrl Pts',(-2.8701221650361,2.69152550264971,40.3791896079451));
#27884=CARTESIAN_POINT('Ctrl Pts',(-2.78841979895134,2.77366256506017,40.3733247977741));
#27885=CARTESIAN_POINT('Ctrl Pts',(-2.70680147827903,2.85571513489572,40.3674660206032));
#27886=CARTESIAN_POINT('Ctrl Pts',(-2.62147075470606,2.93425012980326,40.3616072434324));
#27887=CARTESIAN_POINT('Ctrl Pts',(-2.53276609625377,3.00891756312257,40.3557484662616));
#27888=CARTESIAN_POINT('Ctrl Pts',(-2.4405701333704,3.08652381324533,40.3496590949477));
#27889=CARTESIAN_POINT('Ctrl Pts',(-2.34472948487233,3.15995145527803,40.3435697236339));
#27890=CARTESIAN_POINT('Ctrl Pts',(-2.24566615522885,3.228850030469,40.33748035232));
#27891=CARTESIAN_POINT('Ctrl Pts',(-2.15046464221147,3.29506271104948,40.3316283648642));
#27892=CARTESIAN_POINT('Ctrl Pts',(-2.05228737424939,3.35709256806077,40.3257763774084));
#27893=CARTESIAN_POINT('Ctrl Pts',(-1.95154140619407,3.4146705756061,40.3199243899526));
#27894=CARTESIAN_POINT('Ctrl Pts',(-1.85081080027235,3.47223980343486,40.3140732948304));
#27895=CARTESIAN_POINT('Ctrl Pts',(-1.74751263184131,3.52535832648561,40.3082221997082));
#27896=CARTESIAN_POINT('Ctrl Pts',(-1.64208047633481,3.57380199636746,40.3023711045861));
#27897=CARTESIAN_POINT('Ctrl Pts',(-1.53663886795298,3.62225000962984,40.2965194848642));
#27898=CARTESIAN_POINT('Ctrl Pts',(-1.42906326778344,3.66602216391514,40.2906678651424));
#27899=CARTESIAN_POINT('Ctrl Pts',(-1.31980858498105,3.70494187525396,40.2848162454205));
#27900=CARTESIAN_POINT('Ctrl Pts',(-1.21051765142338,3.74387450017135,40.2789626841285));
#27901=CARTESIAN_POINT('Ctrl Pts',(-1.09954691662211,3.7779513420285,40.2731091228364));
#27902=CARTESIAN_POINT('Ctrl Pts',(-0.987367162415443,3.80704545370602,
40.2672555615444));
#27903=CARTESIAN_POINT('Ctrl Pts',(-0.875059831446061,3.83617265274951,
40.2613953432722));
#27904=CARTESIAN_POINT('Ctrl Pts',(-0.761541137049103,3.86030570733626,
40.255535125));
#27905=CARTESIAN_POINT('Ctrl Pts',(-0.647292886608793,3.87936862375125,
40.2496749067278));
#27906=CARTESIAN_POINT('Ctrl Pts',(-0.53296773170299,3.89844437207738,40.2438107437391));
#27907=CARTESIAN_POINT('Ctrl Pts',(-0.417912452234003,3.91244313667986,
40.2379465807504));
#27908=CARTESIAN_POINT('Ctrl Pts',(-0.30261307848539,3.92134088351543,40.2320824177618));
#27909=CARTESIAN_POINT('Ctrl Pts',(-0.187143692032647,3.93025175037023,
40.2262096078727));
#27910=CARTESIAN_POINT('Ctrl Pts',(-0.0714299045538827,3.93404657419229,
40.2203367979835));
#27911=CARTESIAN_POINT('Ctrl Pts',(0.0440430656483174,3.9327533876876,40.2144639880944));
#27912=CARTESIAN_POINT('Ctrl Pts',(0.0758988375731602,3.93239663359807,
40.2128438436393));
#27913=CARTESIAN_POINT('Ctrl Pts',(0.107736319591384,3.93165295775469,40.2112236991842));
#27914=CARTESIAN_POINT('Ctrl Pts',(0.139545428639648,3.9305236385685,40.2096035547291));
#27915=CARTESIAN_POINT('Ctrl Pts',(0.254838451148347,3.92643038898535,40.2037312949672));
#27916=CARTESIAN_POINT('Ctrl Pts',(0.370144396461502,3.91725319001592,40.1978590352052));
#27917=CARTESIAN_POINT('Ctrl Pts',(0.484978287944126,3.90298412246614,40.1919867754433));
#27918=CARTESIAN_POINT('Ctrl Pts',(0.599663355638497,3.88873354751171,40.1861221260821));
#27919=CARTESIAN_POINT('Ctrl Pts',(0.713877179661275,3.86940427755655,40.180257476721));
#27920=CARTESIAN_POINT('Ctrl Pts',(0.827135695542844,3.84504038225333,40.1743928273599));
#27921=CARTESIAN_POINT('Ctrl Pts',(0.940277725286697,3.82070154516355,40.1685342097779));
#27922=CARTESIAN_POINT('Ctrl Pts',(1.05246599948158,3.79133846864503,40.1626755921959));
#27923=CARTESIAN_POINT('Ctrl Pts',(1.16322315497426,3.75704683118693,40.1568169746139));
#27924=CARTESIAN_POINT('Ctrl Pts',(1.27834384896804,3.72140419406069,40.1507275430202));
#27925=CARTESIAN_POINT('Ctrl Pts',(1.39191789019005,3.68043672491118,40.1446381114265));
#27926=CARTESIAN_POINT('Ctrl Pts',(1.50342232422801,3.63431015668901,40.1385486798329));
#27927=CARTESIAN_POINT('Ctrl Pts',(1.61057603848535,3.58998337135894,40.1326968478532));
#27928=CARTESIAN_POINT('Ctrl Pts',(1.71581820483762,3.5408927104959,40.1268450158735));
#27929=CARTESIAN_POINT('Ctrl Pts',(1.81870252352016,3.48723531338816,40.1209931838938));
#27930=CARTESIAN_POINT('Ctrl Pts',(1.92157118512904,3.43358608193511,40.1151422424538));
#27931=CARTESIAN_POINT('Ctrl Pts',(2.02208234608012,3.37537168716856,40.1092913010138));
#27932=CARTESIAN_POINT('Ctrl Pts',(2.11981313868685,3.31283583309687,40.1034403595737));
#27933=CARTESIAN_POINT('Ctrl Pts',(2.21755272678131,3.25029435097978,40.097588891566));
#27934=CARTESIAN_POINT('Ctrl Pts',(2.31251110087847,3.18343085924278,40.0917374235582));
#27935=CARTESIAN_POINT('Ctrl Pts',(2.40429388921138,3.11253271377199,40.0858859555504));
#27936=CARTESIAN_POINT('Ctrl Pts',(2.49610716553233,3.04161101767858,40.0800325438287));
#27937=CARTESIAN_POINT('Ctrl Pts',(2.5847424316022,2.96665225549757,40.0741791321069));
#27938=CARTESIAN_POINT('Ctrl Pts',(2.66983850645237,2.88798395935022,40.0683257203852));
#27939=CARTESIAN_POINT('Ctrl Pts',(2.75503141718546,2.80922614187151,40.0624656477182));
#27940=CARTESIAN_POINT('Ctrl Pts',(2.83667679426988,2.72675064561217,40.0566055750513));
#27941=CARTESIAN_POINT('Ctrl Pts',(2.91445037436277,2.64092181167423,40.0507455023844));
#27942=CARTESIAN_POINT('Ctrl Pts',(2.99227633610857,2.55503517075115,40.0448814828721));
#27943=CARTESIAN_POINT('Ctrl Pts',(3.06622504527783,2.46579101252098,40.0390174633598));
#27944=CARTESIAN_POINT('Ctrl Pts',(3.13601367904373,2.37358530599821,40.0331534438475));
#27945=CARTESIAN_POINT('Ctrl Pts',(3.20590527171927,2.28124356874244,40.0272807731692));
#27946=CARTESIAN_POINT('Ctrl Pts',(3.27162430620553,2.18593190221344,40.0214081024909));
#27947=CARTESIAN_POINT('Ctrl Pts',(3.33293221062449,2.08807372460403,40.0155354318126));
#27948=CARTESIAN_POINT('Ctrl Pts',(3.34986100144671,2.06105240272565,40.0139138266636));
#27949=CARTESIAN_POINT('Ctrl Pts',(3.36645373589272,2.03383705125486,40.0122922215146));
#27950=CARTESIAN_POINT('Ctrl Pts',(3.38270602987505,2.00643687053617,40.0106706163656));
#27951=CARTESIAN_POINT('Ctrl Pts',(3.44369369945361,1.90361611367065,40.0045854496118));
#27952=CARTESIAN_POINT('Ctrl Pts',(3.50007586451126,1.7978671486112,39.998500282858));
#27953=CARTESIAN_POINT('Ctrl Pts',(3.55157138761894,1.68962412348028,39.9924151161042));
#27954=CARTESIAN_POINT('Ctrl Pts',(3.60298325692126,1.58155693773127,39.9863398346244));
#27955=CARTESIAN_POINT('Ctrl Pts',(3.64952413097963,1.47100409189806,39.9802645531446));
#27956=CARTESIAN_POINT('Ctrl Pts',(3.69095737696613,1.35842653147651,39.9741892716648));
#27957=CARTESIAN_POINT('Ctrl Pts',(3.73230921499947,1.24607016320508,39.968125926885));
#27958=CARTESIAN_POINT('Ctrl Pts',(3.76857329834686,1.13169735592075,39.9620625821053));
#27959=CARTESIAN_POINT('Ctrl Pts',(3.79956034111828,1.01579043813237,39.9559992373255));
#27960=CARTESIAN_POINT('Ctrl Pts',(3.8305116112623,0.900017327723231,39.9499428923029));
#27961=CARTESIAN_POINT('Ctrl Pts',(3.85619787215542,0.782713989463498,39.9438865472803));
#27962=CARTESIAN_POINT('Ctrl Pts',(3.876478819681,0.664380132578184,39.9378302022577));
#27963=CARTESIAN_POINT('Ctrl Pts',(3.8967330581697,0.54620211571679,39.9317818331515));
#27964=CARTESIAN_POINT('Ctrl Pts',(3.91159610689816,0.426996649940712,39.9257334640453));
#27965=CARTESIAN_POINT('Ctrl Pts',(3.92097831272722,0.307275236754875,39.9196850949391));
#27966=CARTESIAN_POINT('Ctrl Pts',(3.92900397987927,0.204863902926982,39.9145112373044));
#27967=CARTESIAN_POINT('Ctrl Pts',(3.93301993290991,0.102075387700563,39.9093373796697));
#27968=CARTESIAN_POINT('Ctrl Pts',(3.93299992557071,-0.000765154113278074,
39.904163522035));
#27969=CARTESIAN_POINT('',(3.93299854544019,-0.00338253830022365,38.654163522061));
#27970=CARTESIAN_POINT('Ctrl Pts',(3.93299992557056,-0.000765154855056982,
39.9041635219977));
#27971=CARTESIAN_POINT('Ctrl Pts',(3.93297584444362,-0.124545419536255,
39.897936197091));
#27972=CARTESIAN_POINT('Ctrl Pts',(3.92710405386225,-0.248177403224034,
39.8917088721844));
#27973=CARTESIAN_POINT('Ctrl Pts',(3.91545184109601,-0.371114375978427,
39.8854815472778));
#27974=CARTESIAN_POINT('Ctrl Pts',(3.90376045750328,-0.494464621552789,
39.879233288196));
#27975=CARTESIAN_POINT('Ctrl Pts',(3.88624980653845,-0.617114855074719,
39.8729850291141));
#27976=CARTESIAN_POINT('Ctrl Pts',(3.86303883359203,-0.738525537919935,
39.8667367700323));
#27977=CARTESIAN_POINT('Ctrl Pts',(3.83978886561927,-0.860140193807824,
39.8604780137159));
#27978=CARTESIAN_POINT('Ctrl Pts',(3.81081953373273,-0.980510824637065,
39.8542192573995));
#27979=CARTESIAN_POINT('Ctrl Pts',(3.77629983507415,-1.09911262189958,39.8479605010831));
#27980=CARTESIAN_POINT('Ctrl Pts',(3.74167620520879,-1.21807150304158,39.8416829010305));
#27981=CARTESIAN_POINT('Ctrl Pts',(3.7014688820161,-1.33525058575408,39.8354053009779));
#27982=CARTESIAN_POINT('Ctrl Pts',(3.655896061848,-1.45014240161587,39.8291277009252));
#27983=CARTESIAN_POINT('Ctrl Pts',(3.61381456675723,-1.55623237733661,39.8233310266176));
#27984=CARTESIAN_POINT('Ctrl Pts',(3.56715880258182,-1.66037218740392,39.8175343523099));
#27985=CARTESIAN_POINT('Ctrl Pts',(3.51613468984839,-1.76218212533346,39.8117376780022));
#27986=CARTESIAN_POINT('Ctrl Pts',(3.4644459897974,-1.86531813421112,39.8058655022106));
#27987=CARTESIAN_POINT('Ctrl Pts',(3.40812898834692,-1.9663508802791,39.7999933264189));
#27988=CARTESIAN_POINT('Ctrl Pts',(3.34737823258863,-2.06483606322435,39.7941211506273));
#27989=CARTESIAN_POINT('Ctrl Pts',(3.28670623631199,-2.16319356640888,39.7882565877372));
#27990=CARTESIAN_POINT('Ctrl Pts',(3.22161213161076,-2.25900972585437,39.7823920248471));
#27991=CARTESIAN_POINT('Ctrl Pts',(3.15233736284497,-2.35186269812071,39.776527461957));
#27992=CARTESIAN_POINT('Ctrl Pts',(3.08313387225576,-2.44462013213162,39.7706689332314));
#27993=CARTESIAN_POINT('Ctrl Pts',(3.00975851934864,-2.53442011398401,39.7648104045057));
#27994=CARTESIAN_POINT('Ctrl Pts',(2.93249689180978,-2.62086836363942,39.7589518757801));
#27995=CARTESIAN_POINT('Ctrl Pts',(2.85218971538898,-2.71072428639816,39.7528624117742));
#27996=CARTESIAN_POINT('Ctrl Pts',(2.76768381859389,-2.79695841363815,39.7467729477683));
#27997=CARTESIAN_POINT('Ctrl Pts',(2.6793474830879,-2.87916412607384,39.7406834837624));
#27998=CARTESIAN_POINT('Ctrl Pts',(2.59445970586742,-2.95816061334627,39.7348317460719));
#27999=CARTESIAN_POINT('Ctrl Pts',(2.50603528321026,-3.03343700738436,39.7289800083814));
#28000=CARTESIAN_POINT('Ctrl Pts',(2.41443914510351,-3.10466948556394,39.7231282706908));
#28001=CARTESIAN_POINT('Ctrl Pts',(2.32285697544311,-3.17589110076315,39.7172774253926));
#28002=CARTESIAN_POINT('Ctrl Pts',(2.2281043783036,-3.24306977257902,39.7114265800943));
#28003=CARTESIAN_POINT('Ctrl Pts',(2.13057887950191,-3.30592235816578,39.705575734796));
#28004=CARTESIAN_POINT('Ctrl Pts',(2.03304463285899,-3.36878058150313,39.6997243646886));
#28005=CARTESIAN_POINT('Ctrl Pts',(1.93273733762553,-3.42731172325869,39.6938729945813));
#28006=CARTESIAN_POINT('Ctrl Pts',(1.83008235984536,-3.48127671353238,39.6880216244739));
#28007=CARTESIAN_POINT('Ctrl Pts',(1.72739331125911,-3.53525961458604,39.6821683123186));
#28008=CARTESIAN_POINT('Ctrl Pts',(1.62235539649211,-3.58467315844459,39.6763150001632));
#28009=CARTESIAN_POINT('Ctrl Pts',(1.5154167078962,-3.62932517163026,39.6704616880078));
#28010=CARTESIAN_POINT('Ctrl Pts',(1.40835636163583,-3.67402798270499,39.664601716894));
#28011=CARTESIAN_POINT('Ctrl Pts',(1.29939130717468,-3.71395829172389,39.6587417457802));
#28012=CARTESIAN_POINT('Ctrl Pts',(1.18898775042528,-3.74897280989588,39.6528817746663));
#28013=CARTESIAN_POINT('Ctrl Pts',(1.07850985814193,-3.78401090360277,39.6470178579905));
#28014=CARTESIAN_POINT('Ctrl Pts',(0.966591933218341,-3.81412650876455,
39.6411539413146));
#28015=CARTESIAN_POINT('Ctrl Pts',(0.853711702038665,-3.83922717871738,
39.6352900246387));
#28016=CARTESIAN_POINT('Ctrl Pts',(0.740664957332911,-3.86436487553503,
39.6294174578969));
#28017=CARTESIAN_POINT('Ctrl Pts',(0.626653478846901,-3.88447280116349,
39.6235448911551));
#28018=CARTESIAN_POINT('Ctrl Pts',(0.51216154411238,-3.89951016830735,39.6176723244133));
#28019=CARTESIAN_POINT('Ctrl Pts',(0.480528629986609,-3.90366483426389,
39.6160497961551));
#28020=CARTESIAN_POINT('Ctrl Pts',(0.448859045477699,-3.90743274129828,
39.614427267897));
#28021=CARTESIAN_POINT('Ctrl Pts',(0.417162998552484,-3.91081373024064,
39.6128047396388));
#28022=CARTESIAN_POINT('Ctrl Pts',(0.302450944877489,-3.92304996228389,
39.6069326020476));
#28023=CARTESIAN_POINT('Ctrl Pts',(0.187007763857721,-3.93025532372492,
39.6010604644563));
#28024=CARTESIAN_POINT('Ctrl Pts',(0.0713124254032304,-3.93235343502884,
39.5951883268651));
#28025=CARTESIAN_POINT('Ctrl Pts',(-0.0442329189806668,-3.93444882622096,
39.5893238022498));
#28026=CARTESIAN_POINT('Ctrl Pts',(-0.160029361168823,-3.93145012727812,
39.5834592776345));
#28027=CARTESIAN_POINT('Ctrl Pts',(-0.275591486117182,-3.9233325544465,
39.5775947530191));
#28028=CARTESIAN_POINT('Ctrl Pts',(-0.391034705595154,-3.91522333403845,
39.5717362625959));
#28029=CARTESIAN_POINT('Ctrl Pts',(-0.506243677474003,-3.90200574478828,
39.5658777721726));
#28030=CARTESIAN_POINT('Ctrl Pts',(-0.620732326585401,-3.88370704079644,
39.5600192817493));
#28031=CARTESIAN_POINT('Ctrl Pts',(-0.739735021830795,-3.86468685747323,
39.5539298033963));
#28032=CARTESIAN_POINT('Ctrl Pts',(-0.85795896923823,-3.84017663347876,
39.5478403250432));
#28033=CARTESIAN_POINT('Ctrl Pts',(-0.974863013293591,-3.81026653993026,
39.5417508466901));
#28034=CARTESIAN_POINT('Ctrl Pts',(-1.0872022489953,-3.78152436016946,39.5358991471228));
#28035=CARTESIAN_POINT('Ctrl Pts',(-1.19832228676465,-3.74779621277451,
39.5300474475556));
#28036=CARTESIAN_POINT('Ctrl Pts',(-1.30775346440781,-3.70921418582553,
39.5241957479884));
#28037=CARTESIAN_POINT('Ctrl Pts',(-1.41716795611689,-3.67063804181752,
39.5183449406812));
#28038=CARTESIAN_POINT('Ctrl Pts',(-1.52489370994096,-3.62720962725778,
39.5124941333741));
#28039=CARTESIAN_POINT('Ctrl Pts',(-1.63047768019904,-3.57911043897401,
39.5066433260669));
#28040=CARTESIAN_POINT('Ctrl Pts',(-1.73607112432105,-3.53100693483469,
39.5007919937771));
#28041=CARTESIAN_POINT('Ctrl Pts',(-1.8395220266095,-3.4782319952331,39.4949406614873));
#28042=CARTESIAN_POINT('Ctrl Pts',(-1.94039938280693,-3.42101435764343,
39.4890893291975));
#28043=CARTESIAN_POINT('Ctrl Pts',(-2.04131022375093,-3.36377772750513,
39.4832360546445));
#28044=CARTESIAN_POINT('Ctrl Pts',(-2.13964546057822,-3.30209567091129,
39.4773827800915));
#28045=CARTESIAN_POINT('Ctrl Pts',(-2.23500126961058,-3.2362413885307,39.4715295055385));
#28046=CARTESIAN_POINT('Ctrl Pts',(-2.33046556821409,-3.17031218147665,
39.4656695715145));
#28047=CARTESIAN_POINT('Ctrl Pts',(-2.42294333270254,-3.10020150904889,
39.4598096374905));
#28048=CARTESIAN_POINT('Ctrl Pts',(-2.51206208548798,-3.02622422808585,
39.4539497034664));
#28049=CARTESIAN_POINT('Ctrl Pts',(-2.60124084681026,-2.95219713416817,
39.4480858236279));
#28050=CARTESIAN_POINT('Ctrl Pts',(-2.68705578737379,-2.87429852462632,
39.4422219437894));
#28051=CARTESIAN_POINT('Ctrl Pts',(-2.76917098541532,-2.79288042234786,
39.4363580639509));
#28052=CARTESIAN_POINT('Ctrl Pts',(-2.85140732442288,-2.7113422074983,39.4304855333865));
#28053=CARTESIAN_POINT('Ctrl Pts',(-2.92993274825609,-2.6262744399724,39.4246130028221));
#28054=CARTESIAN_POINT('Ctrl Pts',(-3.00445126377738,-2.53806256888724,
39.4187404722577));
#28055=CARTESIAN_POINT('Ctrl Pts',(-3.02504466499175,-2.51368497037473,
39.4171175819302));
#28056=CARTESIAN_POINT('Ctrl Pts',(-3.04533231008813,-2.48906742438508,
39.4154946916027));
#28057=CARTESIAN_POINT('Ctrl Pts',(-3.06530854553996,-2.46421844012248,
39.4138718012753));
#28058=CARTESIAN_POINT('Ctrl Pts',(-3.13758853511927,-2.37430738916955,
39.4079996990846));
#28059=CARTESIAN_POINT('Ctrl Pts',(-3.2060304752323,-2.28106274119832,39.402127596894));
#28060=CARTESIAN_POINT('Ctrl Pts',(-3.27031128522053,-2.18484624121681,
39.3962554947034));
#28061=CARTESIAN_POINT('Ctrl Pts',(-3.33450875013576,-2.08875449341588,
39.3903910061502));
#28062=CARTESIAN_POINT('Ctrl Pts',(-3.39455558654056,-1.98969889687443,
39.3845265175971));
#28063=CARTESIAN_POINT('Ctrl Pts',(-3.45016864544456,-1.88807450011679,
39.378662029044));
#28064=CARTESIAN_POINT('Ctrl Pts',(-3.50572447615461,-1.78655467916926,
39.3728035752981));
#28065=CARTESIAN_POINT('Ctrl Pts',(-3.55685540721134,-1.68247167634076,
39.3669451215521));
#28066=CARTESIAN_POINT('Ctrl Pts',(-3.60332171931176,-1.5762492147932,39.3610866678062));
#28067=CARTESIAN_POINT('Ctrl Pts',(-3.65162050975432,-1.46583768913797,
39.3549971759356));
#28068=CARTESIAN_POINT('Ctrl Pts',(-3.69487894392114,-1.35311486465532,
39.348907684065));
#28069=CARTESIAN_POINT('Ctrl Pts',(-3.73288047496086,-1.23858482134087,
39.3428181921944));
#28070=CARTESIAN_POINT('Ctrl Pts',(-3.76939782383343,-1.12852784643285,
39.3369665306163));
#28071=CARTESIAN_POINT('Ctrl Pts',(-3.80106104610488,-1.01680259758531,
39.3311148690381));
#28072=CARTESIAN_POINT('Ctrl Pts',(-3.82772750277615,-0.903875635522399,
39.32526320746));
#28073=CARTESIAN_POINT('Ctrl Pts',(-3.85438989143289,-0.790965900664772,
39.3194124385631));
#28074=CARTESIAN_POINT('Ctrl Pts',(-3.87605693512701,-0.676855219335641,
39.3135616696661));
#28075=CARTESIAN_POINT('Ctrl Pts',(-3.89263654801243,-0.562022868821104,
39.3077109007692));
#28076=CARTESIAN_POINT('Ctrl Pts',(-3.90921764748462,-0.447180222031505,
39.3018596072716));
#28077=CARTESIAN_POINT('Ctrl Pts',(-3.92071035026978,-0.331616186621927,
39.296008313774));
#28078=CARTESIAN_POINT('Ctrl Pts',(-3.92707423075191,-0.215817020098731,
39.2901570202764));
#28079=CARTESIAN_POINT('Ctrl Pts',(-3.93344022327085,-0.0999794222908921,
39.2843037848587));
#28080=CARTESIAN_POINT('Ctrl Pts',(-3.9346739862053,0.0160930492229305,
39.2784505494411));
#28081=CARTESIAN_POINT('Ctrl Pts',(-3.93078719408863,0.131912981881411,
39.2725973140234));
#28082=CARTESIAN_POINT('Ctrl Pts',(-3.92689598001484,0.247864681498345,
39.2667374194495));
#28083=CARTESIAN_POINT('Ctrl Pts',(-3.91787259703238,0.36356285536572,39.2608775248756));
#28084=CARTESIAN_POINT('Ctrl Pts',(-3.90378070873002,0.478523957756888,
39.2550176303017));
#28085=CARTESIAN_POINT('Ctrl Pts',(-3.88967933208241,0.593562465716907,
39.2491537901456));
#28086=CARTESIAN_POINT('Ctrl Pts',(-3.87050272295229,0.707862507278183,
39.2432899499895));
#28087=CARTESIAN_POINT('Ctrl Pts',(-3.84636557089953,0.820951213531456,
39.2374261098335));
#28088=CARTESIAN_POINT('Ctrl Pts',(-3.8221928102654,0.934206755059616,39.231553618987));
#28089=CARTESIAN_POINT('Ctrl Pts',(-3.7930450048547,1.04624699608982,39.2256811281406));
#28090=CARTESIAN_POINT('Ctrl Pts',(-3.75908654585292,1.15661460339541,39.2198086372942));
#28091=CARTESIAN_POINT('Ctrl Pts',(-3.7496998399369,1.18712212060575,39.2181853791667));
#28092=CARTESIAN_POINT('Ctrl Pts',(-3.73994585001045,1.21750196016856,39.2165621210393));
#28093=CARTESIAN_POINT('Ctrl Pts',(-3.7298286840558,1.24774476059591,39.2149388629118));
#28094=CARTESIAN_POINT('Ctrl Pts',(-3.69322985954276,1.35714802140888,39.2090667303787));
#28095=CARTESIAN_POINT('Ctrl Pts',(-3.65175207639979,1.46512305146793,39.2031945978455));
#28096=CARTESIAN_POINT('Ctrl Pts',(-3.6055251521091,1.5712025259363,39.1973224653123));
#28097=CARTESIAN_POINT('Ctrl Pts',(-3.55935816121916,1.67714446792224,39.1914579460235));
#28098=CARTESIAN_POINT('Ctrl Pts',(-3.50845443740917,1.7811953660978,39.1855934267348));
#28099=CARTESIAN_POINT('Ctrl Pts',(-3.45299339794814,1.88290350090666,39.179728907446));
#28100=CARTESIAN_POINT('Ctrl Pts',(-3.39758942659797,1.98450698042652,39.1738704226102));
#28101=CARTESIAN_POINT('Ctrl Pts',(-3.33763766370624,2.08377213070397,39.1680119377745));
#28102=CARTESIAN_POINT('Ctrl Pts',(-3.27336512150243,2.18026828196242,39.1621534529387));
#28103=CARTESIAN_POINT('Ctrl Pts',(-3.20655836280267,2.28056920163255,39.1560639725891));
#28104=CARTESIAN_POINT('Ctrl Pts',(-3.13508326715353,2.37787785409162,39.1499744922395));
#28105=CARTESIAN_POINT('Ctrl Pts',(-3.05924697712946,2.4717396571897,39.1438850118899));
#28106=CARTESIAN_POINT('Ctrl Pts',(-2.98637200435748,2.56193626811212,39.1380333185314));
#28107=CARTESIAN_POINT('Ctrl Pts',(-2.90947032923454,2.64894981731903,39.1321816251728));
#28108=CARTESIAN_POINT('Ctrl Pts',(-2.82885746565195,2.73240817577191,39.1263299318142));
#28109=CARTESIAN_POINT('Ctrl Pts',(-2.74825689686142,2.81585380544783,39.1204791309355));
#28110=CARTESIAN_POINT('Ctrl Pts',(-2.6639465521651,2.89574502521451,39.1146283300567));
#28111=CARTESIAN_POINT('Ctrl Pts',(-2.5762799617768,2.97174537242801,39.108777529178));
#28112=CARTESIAN_POINT('Ctrl Pts',(-2.48860550841617,3.04775253624777,39.1029262035305));
#28113=CARTESIAN_POINT('Ctrl Pts',(-2.39757452333728,3.11986786295776,39.097074877883));
#28114=CARTESIAN_POINT('Ctrl Pts',(-2.30357432451143,3.18779458739921,39.0912235522355));
#28115=CARTESIAN_POINT('Ctrl Pts',(-2.20954292702009,3.25574385672014,39.085370284533));
#28116=CARTESIAN_POINT('Ctrl Pts',(-2.11254069111792,3.3195015174474,39.0795170168306));
#28117=CARTESIAN_POINT('Ctrl Pts',(-2.0129840587443,3.37881401962897,39.0736637491282));
#28118=CARTESIAN_POINT('Ctrl Pts',(-1.91331416195372,3.43819400095099,39.0678038222315));
#28119=CARTESIAN_POINT('Ctrl Pts',(-1.81108442354978,3.49311851796205,39.0619438953348));
#28120=CARTESIAN_POINT('Ctrl Pts',(-1.7067361238206,3.54337985596321,39.0560839684381));
#28121=CARTESIAN_POINT('Ctrl Pts',(-1.60231756360945,3.59367503625831,39.050220095897));
#28122=CARTESIAN_POINT('Ctrl Pts',(-1.49577798076658,3.63930062315217,39.0443562233559));
#28123=CARTESIAN_POINT('Ctrl Pts',(-1.38757724339026,3.68009760653511,39.0384923508147));
#28124=CARTESIAN_POINT('Ctrl Pts',(-1.27921688558971,3.72095477464464,39.0326198277427));
#28125=CARTESIAN_POINT('Ctrl Pts',(-1.16919087378767,3.75696899438222,39.0267473046707));
#28126=CARTESIAN_POINT('Ctrl Pts',(-1.05797285985379,3.78803147133347,39.0208747815987));
#28127=CARTESIAN_POINT('Ctrl Pts',(-1.02723623526008,3.79661601316469,39.0192518292486));
#28128=CARTESIAN_POINT('Ctrl Pts',(-0.996408618161356,3.80482265899863,
39.0176288768985));
#28129=CARTESIAN_POINT('Ctrl Pts',(-0.965500099659244,3.81264980788401,
39.0160059245485));
#28130=CARTESIAN_POINT('Ctrl Pts',(-0.853667681370461,3.84096979960727,
39.0101337994881));
#28131=CARTESIAN_POINT('Ctrl Pts',(-0.740400701736088,3.86441270439239,
39.0042616744278));
#28132=CARTESIAN_POINT('Ctrl Pts',(-0.626162532679911,3.88283523764116,
38.9983895493674));
#28133=CARTESIAN_POINT('Ctrl Pts',(-0.512072474885856,3.90123388583755,
38.9925250375931));
#28134=CARTESIAN_POINT('Ctrl Pts',(-0.397014136048743,3.9146250412806,38.9866605258187));
#28135=CARTESIAN_POINT('Ctrl Pts',(-0.281464558394382,3.92291558695415,
38.9807960140444));
#28136=CARTESIAN_POINT('Ctrl Pts',(-0.166033879338691,3.93119760179373,
38.9749375367554));
#28137=CARTESIAN_POINT('Ctrl Pts',(-0.0501133767523756,3.9343894168585,
38.9690790594664));
#28138=CARTESIAN_POINT('Ctrl Pts',(0.0658119013823674,3.93244933770754,
38.9632205821774));
#28139=CARTESIAN_POINT('Ctrl Pts',(0.186308234291358,3.93043275920968,38.957131099011));
#28140=CARTESIAN_POINT('Ctrl Pts',(0.306809277858817,3.92287117607742,38.9510416158447));
#28141=CARTESIAN_POINT('Ctrl Pts',(0.426766562145073,3.90977739793903,38.9449521326783));
#28142=CARTESIAN_POINT('Ctrl Pts',(0.542039454016827,3.89719493843671,38.939100446899));
#28143=CARTESIAN_POINT('Ctrl Pts',(0.656809808134693,3.87950429503028,38.9332487611196));
#28144=CARTESIAN_POINT('Ctrl Pts',(0.770594013338357,3.8567698747277,38.9273970753402));
#28145=CARTESIAN_POINT('Ctrl Pts',(0.884360864570448,3.83403892179989,38.9215462820396));
#28146=CARTESIAN_POINT('Ctrl Pts',(0.997141460650802,3.80626580248217,38.9156954887391));
#28147=CARTESIAN_POINT('Ctrl Pts',(1.10846165954716,3.77356618456785,38.9098446954385));
#28148=CARTESIAN_POINT('Ctrl Pts',(1.21979184313737,3.74086363371164,38.90399337736));
#28149=CARTESIAN_POINT('Ctrl Pts',(1.32966097247394,3.70323382237404,38.8981420592815));
#28150=CARTESIAN_POINT('Ctrl Pts',(1.43761005149298,3.66084229923202,38.892290741203));
#28151=CARTESIAN_POINT('Ctrl Pts',(1.54559495917646,3.61843670620008,38.8864374810523));
#28152=CARTESIAN_POINT('Ctrl Pts',(1.65165816476864,3.57126640981792,38.8805842209015));
#28153=CARTESIAN_POINT('Ctrl Pts',(1.7553612982158,3.51954481612696,38.8747309607508));
#28154=CARTESIAN_POINT('Ctrl Pts',(1.85918241479537,3.46776437874021,38.8688710413416));
#28155=CARTESIAN_POINT('Ctrl Pts',(1.96063772975617,3.41142249348793,38.8630111219324));
#28156=CARTESIAN_POINT('Ctrl Pts',(2.05931401940264,3.35077823340963,38.8571512025232));
#28157=CARTESIAN_POINT('Ctrl Pts',(2.15805675097397,3.29009313959725,38.8512873374415));
#28158=CARTESIAN_POINT('Ctrl Pts',(2.25401638983479,3.22510013387591,38.8454234723598));
#28159=CARTESIAN_POINT('Ctrl Pts',(2.34681065051272,3.15610024724185,38.839559607278));
#28160=CARTESIAN_POINT('Ctrl Pts',(2.4397418053458,3.08699856895476,38.8336870915659));
#28161=CARTESIAN_POINT('Ctrl Pts',(2.52949794281579,3.01387847237749,38.8278145758537));
#28162=CARTESIAN_POINT('Ctrl Pts',(2.61573158303177,2.93707972066304,38.8219420601415));
#28163=CARTESIAN_POINT('Ctrl Pts',(2.63956452461567,2.91585435943809,38.8203190354893));
#28164=CARTESIAN_POINT('Ctrl Pts',(2.66312863247738,2.89434821298065,38.8186960108372));
#28165=CARTESIAN_POINT('Ctrl Pts',(2.68641710589835,2.87256890833566,38.817072986185));
#28166=CARTESIAN_POINT('Ctrl Pts',(2.7694231565749,2.79494191955099,38.811288112952));
#28167=CARTESIAN_POINT('Ctrl Pts',(2.84922079101553,2.71356508602149,38.8055032397191));
#28168=CARTESIAN_POINT('Ctrl Pts',(2.92544421824122,2.62873831446933,38.7997183664862));
#28169=CARTESIAN_POINT('Ctrl Pts',(3.00535585908918,2.53980704032839,38.7936535813018));
#28170=CARTESIAN_POINT('Ctrl Pts',(3.08133832905436,2.44708382391803,38.7875887961174));
#28171=CARTESIAN_POINT('Ctrl Pts',(3.15300921663704,2.35096190522132,38.781524010933));
#28172=CARTESIAN_POINT('Ctrl Pts',(3.22120142124661,2.25950544684177,38.7757535916435));
#28173=CARTESIAN_POINT('Ctrl Pts',(3.28549042961106,2.16497283811683,38.7699831723539));
#28174=CARTESIAN_POINT('Ctrl Pts',(3.34558553305421,2.06773945191805,38.7642127530643));
#28175=CARTESIAN_POINT('Ctrl Pts',(3.40564321843576,1.97056660783711,38.7584459267115));
#28176=CARTESIAN_POINT('Ctrl Pts',(3.46151196362247,1.87069668919483,38.7526791003587));
#28177=CARTESIAN_POINT('Ctrl Pts',(3.51294353285398,1.76853519472456,38.7469122740059));
#28178=CARTESIAN_POINT('Ctrl Pts',(3.56435639504785,1.66641085912284,38.741147545202));
#28179=CARTESIAN_POINT('Ctrl Pts',(3.61133509773127,1.56199698520079,38.7353828163982));
#28180=CARTESIAN_POINT('Ctrl Pts',(3.65367709697633,1.45572410539588,38.7296180875944));
#28181=CARTESIAN_POINT('Ctrl Pts',(3.69601465676428,1.34946236804761,38.7238539632086));
#28182=CARTESIAN_POINT('Ctrl Pts',(3.73371632356553,1.24134240938727,38.7180898388228));
#28183=CARTESIAN_POINT('Ctrl Pts',(3.76662783714237,1.13181435600729,38.712325714437));
#28184=CARTESIAN_POINT('Ctrl Pts',(3.79955765479451,1.02222538747881,38.7065583842744));
#28185=CARTESIAN_POINT('Ctrl Pts',(3.82769187595247,0.911227169405309,38.7007910541117));
#28186=CARTESIAN_POINT('Ctrl Pts',(3.85092633608448,0.799284276118953,38.6950237239491));
#28187=CARTESIAN_POINT('Ctrl Pts',(3.87416835248562,0.68730497696714,38.6892545181458));
#28188=CARTESIAN_POINT('Ctrl Pts',(3.89250736448081,0.574380811676093,38.6834853123425));
#28189=CARTESIAN_POINT('Ctrl Pts',(3.90589074838289,0.460984231505777,38.6777161065392));
#28190=CARTESIAN_POINT('Ctrl Pts',(3.91928825110571,0.347468023444683,38.6719408145037));
#28191=CARTESIAN_POINT('Ctrl Pts',(3.92771965890806,0.233478830777794,38.6661655224681));
#28192=CARTESIAN_POINT('Ctrl Pts',(3.93118439497244,0.119491642909193,38.6603902304326));
#28193=CARTESIAN_POINT('Ctrl Pts',(3.93242957881912,0.0785260390580603,
38.6583146609754));
#28194=CARTESIAN_POINT('Ctrl Pts',(3.93303375826257,0.0375606726600528,
38.6562390915182));
#28195=CARTESIAN_POINT('Ctrl Pts',(3.93299854544019,-0.00338253830016815,
38.654163522061));
#28196=CARTESIAN_POINT('',(3.93463686453598,0.00228919349351085,37.4041629160656));
#28197=CARTESIAN_POINT('Ctrl Pts',(3.93299854543975,-0.00338253881235497,
38.654163522035));
#28198=CARTESIAN_POINT('Ctrl Pts',(3.93284766481448,-0.178816824309476,
38.6452700807004));
#28199=CARTESIAN_POINT('Ctrl Pts',(3.92095564116745,-0.353765040641901,
38.6363766393657));
#28200=CARTESIAN_POINT('Ctrl Pts',(3.89753452592024,-0.526985407065219,
38.6274831980311));
#28201=CARTESIAN_POINT('Ctrl Pts',(3.88933271406081,-0.587645236481059,
38.6243688146279));
#28202=CARTESIAN_POINT('Ctrl Pts',(3.87971743278634,-0.648093501288501,
38.6212544312248));
#28203=CARTESIAN_POINT('Ctrl Pts',(3.8686989668374,-0.708277702593558,38.6181400478216));
#28204=CARTESIAN_POINT('Ctrl Pts',(3.84792380700203,-0.821754152715708,
38.6122679224922));
#28205=CARTESIAN_POINT('Ctrl Pts',(3.82211685794453,-0.934506005180074,
38.6063957971629));
#28206=CARTESIAN_POINT('Ctrl Pts',(3.79134061006027,-1.04605228287492,38.6005236718335));
#28207=CARTESIAN_POINT('Ctrl Pts',(3.76060426410881,-1.15745393890912,38.5946591598153));
#28208=CARTESIAN_POINT('Ctrl Pts',(3.72491154062295,-1.26765273367135,38.5887946477971));
#28209=CARTESIAN_POINT('Ctrl Pts',(3.68437623701796,-1.37617613120463,38.5829301357788));
#28210=CARTESIAN_POINT('Ctrl Pts',(3.64388264374113,-1.48458785949848,38.5770716582712));
#28211=CARTESIAN_POINT('Ctrl Pts',(3.59855652546422,-1.59132723466118,38.5712131807636));
#28212=CARTESIAN_POINT('Ctrl Pts',(3.54856177111622,-1.69593583503991,38.565354703256));
#28213=CARTESIAN_POINT('Ctrl Pts',(3.4965956741155,-1.80466925608148,38.5592652201811));
#28214=CARTESIAN_POINT('Ctrl Pts',(3.43958530973284,-1.91109996956278,38.5531757371062));
#28215=CARTESIAN_POINT('Ctrl Pts',(3.37777051633314,-2.01473455794815,38.5470862540313));
#28216=CARTESIAN_POINT('Ctrl Pts',(3.31836961932331,-2.11432216752779,38.5412345680985));
#28217=CARTESIAN_POINT('Ctrl Pts',(3.25453271403067,-2.21132754548618,38.5353828821657));
#28218=CARTESIAN_POINT('Ctrl Pts',(3.18651957414802,-2.3053377200687,38.5295311962329));
#28219=CARTESIAN_POINT('Ctrl Pts',(3.1185168076769,-2.39933355615382,38.5236804028033));
#28220=CARTESIAN_POINT('Ctrl Pts',(3.04633931535211,-2.49033476233057,38.5178296093737));
#28221=CARTESIAN_POINT('Ctrl Pts',(2.97028954486185,-2.57795830448911,38.5119788159441));
#28222=CARTESIAN_POINT('Ctrl Pts',(2.89423295352562,-2.66558970553639,38.5061274977614));
#28223=CARTESIAN_POINT('Ctrl Pts',(2.81430366461514,-2.74984252811148,38.5002761795786));
#28224=CARTESIAN_POINT('Ctrl Pts',(2.73084318317132,-2.83036826383542,38.4944248613958));
#28225=CARTESIAN_POINT('Ctrl Pts',(2.64735500126829,-2.91092072597909,38.4885716011657));
#28226=CARTESIAN_POINT('Ctrl Pts',(2.56033359374045,-2.9877433546469,38.4827183409357));
#28227=CARTESIAN_POINT('Ctrl Pts',(2.47015540294773,-3.0605263085437,38.4768650807056));
#28228=CARTESIAN_POINT('Ctrl Pts',(2.37987461694304,-3.13339206719093,38.4710051612549));
#28229=CARTESIAN_POINT('Ctrl Pts',(2.28643020112129,-3.20220871794049,38.4651452418041));
#28230=CARTESIAN_POINT('Ctrl Pts',(2.19022966268298,-3.26670828582896,38.4592853223534));
#28231=CARTESIAN_POINT('Ctrl Pts',(2.09396434968354,-3.33125128311264,38.453421457252));
#28232=CARTESIAN_POINT('Ctrl Pts',(1.99493957121781,-3.39147119521567,38.4475575921507));
#28233=CARTESIAN_POINT('Ctrl Pts',(1.89358811684596,-3.44714563715254,38.4416937270494));
#28234=CARTESIAN_POINT('Ctrl Pts',(1.79208714493666,-3.5029022121531,38.4358212113502));
#28235=CARTESIAN_POINT('Ctrl Pts',(1.68825301608693,-3.55409975161193,38.429948695651));
#28236=CARTESIAN_POINT('Ctrl Pts',(1.58253925985012,-3.60056363518728,38.4240761799519));
#28237=CARTESIAN_POINT('Ctrl Pts',(1.55332249497194,-3.61340514617008,38.422453156454));
#28238=CARTESIAN_POINT('Ctrl Pts',(1.52396224824739,-3.62588537542524,38.4208301329561));
#28239=CARTESIAN_POINT('Ctrl Pts',(1.49446828468059,-3.63800131199589,38.4192071094581));
#28240=CARTESIAN_POINT('Ctrl Pts',(1.3877586704853,-3.68183695701326,38.4133349854589));
#28241=CARTESIAN_POINT('Ctrl Pts',(1.27893984743706,-3.72104711202814,38.4074628614597));
#28242=CARTESIAN_POINT('Ctrl Pts',(1.16845029607819,-3.75542446410453,38.4015907374605));
#28243=CARTESIAN_POINT('Ctrl Pts',(1.05810399654019,-3.78975724528511,38.3957262267826));
#28244=CARTESIAN_POINT('Ctrl Pts',(0.946091667439092,-3.81926956228804,
38.3898617161047));
#28245=CARTESIAN_POINT('Ctrl Pts',(0.832872410228218,-3.84380183519919,
38.3839972054268));
#28246=CARTESIAN_POINT('Ctrl Pts',(0.719769654429791,-3.86830886466222,
38.378138729268));
#28247=CARTESIAN_POINT('Ctrl Pts',(0.605462842355839,-3.88784595571407,
38.3722802531093));
#28248=CARTESIAN_POINT('Ctrl Pts',(0.490426265947687,-3.90230330416135,
38.3664217769505));
#28249=CARTESIAN_POINT('Ctrl Pts',(0.370853646063752,-3.91733072486869,
38.3603322933732));
#28250=CARTESIAN_POINT('Ctrl Pts',(0.250492961218796,-3.92686942434437,
38.3542428097959));
#28251=CARTESIAN_POINT('Ctrl Pts',(0.129888989964001,-3.93085459541384,
38.3481533262185));
#28252=CARTESIAN_POINT('Ctrl Pts',(0.013994696325034,-3.93468414249526,
38.3423016416473));
#28253=CARTESIAN_POINT('Ctrl Pts',(-0.102123787136036,-3.9333857459539,
38.3364499570761));
#28254=CARTESIAN_POINT('Ctrl Pts',(-0.217978600778682,-3.92695484180842,
38.3305982725049));
#28255=CARTESIAN_POINT('Ctrl Pts',(-0.333815744113324,-3.92052491851175,
38.3247474804392));
#28256=CARTESIAN_POINT('Ctrl Pts',(-0.449388884926641,-3.90896406700047,
38.3188966883736));
#28257=CARTESIAN_POINT('Ctrl Pts',(-0.564212295559321,-3.89231980771617,
38.313045896308));
#28258=CARTESIAN_POINT('Ctrl Pts',(-0.679046004600494,-3.87567405562323,
38.30719457949));
#28259=CARTESIAN_POINT('Ctrl Pts',(-0.793129440627937,-3.85394404872781,
38.3013432626721));
#28260=CARTESIAN_POINT('Ctrl Pts',(-0.905984822818731,-3.82722882786255,
38.2954919458542));
#28261=CARTESIAN_POINT('Ctrl Pts',(-1.01887766162924,-3.8005047402348,38.2896386869885));
#28262=CARTESIAN_POINT('Ctrl Pts',(-1.13054123405462,-3.76879224377626,
38.2837854281227));
#28263=CARTESIAN_POINT('Ctrl Pts',(-1.2405114170697,-3.7322406707124,38.277932169257));
#28264=CARTESIAN_POINT('Ctrl Pts',(-1.35060671270718,-3.69564751307503,
38.2720722511629));
#28265=CARTESIAN_POINT('Ctrl Pts',(-1.4590043810232,-3.65420442067761,38.2662123330687));
#28266=CARTESIAN_POINT('Ctrl Pts',(-1.56525874125782,-3.60810948737923,
38.2603524149746));
#28267=CARTESIAN_POINT('Ctrl Pts',(-1.67158464564546,-3.56198351702078,
38.2544885512271));
#28268=CARTESIAN_POINT('Ctrl Pts',(-1.77576399764922,-3.51119964960478,
38.2486246874795));
#28269=CARTESIAN_POINT('Ctrl Pts',(-1.87737581656042,-3.4560018870646,38.242760823732));
#28270=CARTESIAN_POINT('Ctrl Pts',(-1.97913753739779,-3.40072269451939,
38.236888309372));
#28271=CARTESIAN_POINT('Ctrl Pts',(-2.07832381267025,-3.34101682339705,
38.2310157950119));
#28272=CARTESIAN_POINT('Ctrl Pts',(-2.17454264603275,-3.27717153664328,
38.2251432806519));
#28273=CARTESIAN_POINT('Ctrl Pts',(-2.20113545973998,-3.25952607413459,
38.2235202441328));
#28274=CARTESIAN_POINT('Ctrl Pts',(-2.22750180237679,-3.24156465715202,
38.2218972076138));
#28275=CARTESIAN_POINT('Ctrl Pts',(-2.25363386371177,-3.2232938755769,38.2202741710947));
#28276=CARTESIAN_POINT('Ctrl Pts',(-2.34817929855874,-3.15719044168124,
38.2144020475182));
#28277=CARTESIAN_POINT('Ctrl Pts',(-2.43997235973993,-3.08681285873257,
38.2085299239417));
#28278=CARTESIAN_POINT('Ctrl Pts',(-2.52860167352299,-3.01241806140129,
38.2026578003652));
#28279=CARTESIAN_POINT('Ctrl Pts',(-2.61711607754092,-2.93811971848587,
38.1967932901201));
#28280=CARTESIAN_POINT('Ctrl Pts',(-2.70247457756168,-2.85981478214543,
38.1909287798751));
#28281=CARTESIAN_POINT('Ctrl Pts',(-2.78429482194088,-2.77780333078373,
38.18506426963));
#28282=CARTESIAN_POINT('Ctrl Pts',(-2.86603087401856,-2.69587626847383,
38.1792057939137));
#28283=CARTESIAN_POINT('Ctrl Pts',(-2.94423562201799,-2.61025056821768,
38.1733473181973));
#28284=CARTESIAN_POINT('Ctrl Pts',(-3.01856038951325,-2.52126598653566,
38.167488842481));
#28285=CARTESIAN_POINT('Ctrl Pts',(-3.09581588821695,-2.42877261633813,
38.1613993587414));
#28286=CARTESIAN_POINT('Ctrl Pts',(-3.16887877651891,-2.3326503167294,38.1553098750019));
#28287=CARTESIAN_POINT('Ctrl Pts',(-3.2374001529709,-2.23332246877695,38.1492203912623));
#28288=CARTESIAN_POINT('Ctrl Pts',(-3.30324571012527,-2.13787345960598,
38.1433687071547));
#28289=CARTESIAN_POINT('Ctrl Pts',(-3.36489754235973,-2.03946493519753,
38.1375170230471));
#28290=CARTESIAN_POINT('Ctrl Pts',(-3.42208819548022,-1.93850493482862,
38.1316653389395));
#28291=CARTESIAN_POINT('Ctrl Pts',(-3.47927012574741,-1.83756033311708,
38.1258145473446));
#28292=CARTESIAN_POINT('Ctrl Pts',(-3.53199202610027,-1.73406538882097,
38.1199637557497));
#28293=CARTESIAN_POINT('Ctrl Pts',(-3.58003142036333,-1.62845449098564,
38.1141129641547));
#28294=CARTESIAN_POINT('Ctrl Pts',(-3.62807512318259,-1.52283412112229,
38.1082616478141));
#28295=CARTESIAN_POINT('Ctrl Pts',(-3.67143531387795,-1.41509779679653,
38.1024103314735));
#28296=CARTESIAN_POINT('Ctrl Pts',(-3.7099371617375,-1.30570105918588,38.0965590151329));
#28297=CARTESIAN_POINT('Ctrl Pts',(-3.74845178829314,-1.19626801298899,
38.0907057567506));
#28298=CARTESIAN_POINT('Ctrl Pts',(-3.78210472853592,-1.08517384746374,
38.0848524983683));
#28299=CARTESIAN_POINT('Ctrl Pts',(-3.81077084899311,-0.972889786391225,
38.0789992399861));
#28300=CARTESIAN_POINT('Ctrl Pts',(-3.8394695827467,-0.860477980325405,
38.0731393223821));
#28301=CARTESIAN_POINT('Ctrl Pts',(-3.86317007027577,-0.746873977490936,
38.0672794047782));
#28302=CARTESIAN_POINT('Ctrl Pts',(-3.88179817342039,-0.632559831818427,
38.0614194871742));
#28303=CARTESIAN_POINT('Ctrl Pts',(-3.90043881939564,-0.51816871518662,
38.0555556239214));
#28304=CARTESIAN_POINT('Ctrl Pts',(-3.91400023203977,-0.403066913178866,
38.0496917606686));
#28305=CARTESIAN_POINT('Ctrl Pts',(-3.92246024878263,-0.2877405023978,38.0438278974157));
#28306=CARTESIAN_POINT('Ctrl Pts',(-3.93093274608636,-0.172243957403642,
38.0379553835533));
#28307=CARTESIAN_POINT('Ctrl Pts',(-3.93428881547625,-0.0565225540109119,
38.0320828696908));
#28308=CARTESIAN_POINT('Ctrl Pts',(-3.9325583576423,0.0589386438399231,
38.0262103558284));
#28309=CARTESIAN_POINT('Ctrl Pts',(-3.93208009498766,0.0908497241956913,
38.024587314796));
#28310=CARTESIAN_POINT('Ctrl Pts',(-3.93121359972497,0.122740967516733,
38.0229642737637));
#28311=CARTESIAN_POINT('Ctrl Pts',(-3.92996019662631,0.154602241034456,
38.0213412327313));
#28312=CARTESIAN_POINT('Ctrl Pts',(-3.92542541377613,0.269875577192431,
38.0154691085548));
#28313=CARTESIAN_POINT('Ctrl Pts',(-3.91580694316811,0.385142477371152,
38.0095969843782));
#28314=CARTESIAN_POINT('Ctrl Pts',(-3.90109869561376,0.499917960350094,
38.0037248602017));
#28315=CARTESIAN_POINT('Ctrl Pts',(-3.88640951758781,0.61454463468791,37.9978603493481));
#28316=CARTESIAN_POINT('Ctrl Pts',(-3.86664373768413,0.72868075258105,37.9919958384945));
#28317=CARTESIAN_POINT('Ctrl Pts',(-3.84184725167496,0.84184244060131,37.9861313276409));
#28318=CARTESIAN_POINT('Ctrl Pts',(-3.81707628099344,0.954887686414946,
37.9802728513083));
#28319=CARTESIAN_POINT('Ctrl Pts',(-3.787284988556,1.06696009533074,37.9744143749757));
#28320=CARTESIAN_POINT('Ctrl Pts',(-3.75257085328802,1.17758268968817,37.9685558986431));
#28321=CARTESIAN_POINT('Ctrl Pts',(-3.71648789547975,1.2925672737496,37.9624664151316));
#28322=CARTESIAN_POINT('Ctrl Pts',(-3.67508593776599,1.40598490359337,37.9563769316202));
#28323=CARTESIAN_POINT('Ctrl Pts',(-3.62853270260561,1.51731322610778,37.9502874481087));
#28324=CARTESIAN_POINT('Ctrl Pts',(-3.58379740522979,1.62429409643563,37.9444357633694));
#28325=CARTESIAN_POINT('Ctrl Pts',(-3.53430577739931,1.72934535791776,37.9385840786302));
#28326=CARTESIAN_POINT('Ctrl Pts',(-3.48025664224282,1.83202148025746,37.9327323938909));
#28327=CARTESIAN_POINT('Ctrl Pts',(-3.42621575074423,1.93468194227577,37.9268816016597));
#28328=CARTESIAN_POINT('Ctrl Pts',(-3.36761892654977,2.0349676197157,37.9210308094285));
#28329=CARTESIAN_POINT('Ctrl Pts',(-3.30471146835246,2.13245659063431,37.9151800171973));
#28330=CARTESIAN_POINT('Ctrl Pts',(-3.24179836807022,2.22995430520701,37.9093287002164));
#28331=CARTESIAN_POINT('Ctrl Pts',(-3.17457408939415,2.32465446723433,37.9034773832355));
#28332=CARTESIAN_POINT('Ctrl Pts',(-3.10332747442117,2.41616381615625,37.8976260662546));
#28333=CARTESIAN_POINT('Ctrl Pts',(-3.03205721278336,2.50770353691974,37.8917728072288));
#28334=CARTESIAN_POINT('Ctrl Pts',(-2.95676221410921,2.59605001274159,37.8859195482029));
#28335=CARTESIAN_POINT('Ctrl Pts',(-2.87777137028209,2.68084332634056,37.8800662891771));
#28336=CARTESIAN_POINT('Ctrl Pts',(-2.79869065896901,2.76573310886619,37.8742063709278));
#28337=CARTESIAN_POINT('Ctrl Pts',(-2.71590599190624,2.84706135794204,37.8683464526786));
#28338=CARTESIAN_POINT('Ctrl Pts',(-2.62978292911757,2.92450521383051,37.8624865344294));
#28339=CARTESIAN_POINT('Ctrl Pts',(-2.54360187720603,3.00200121488346,37.8566226705295));
#28340=CARTESIAN_POINT('Ctrl Pts',(-2.45407827223948,3.07560735291503,37.8507588066296));
#28341=CARTESIAN_POINT('Ctrl Pts',(-2.36160914397724,3.14504232898114,37.8448949427297));
#28342=CARTESIAN_POINT('Ctrl Pts',(-2.26900360154762,3.2145797383093,37.8390224282226));
#28343=CARTESIAN_POINT('Ctrl Pts',(-2.17344420326544,3.27993347199441,37.8331499137154));
#28344=CARTESIAN_POINT('Ctrl Pts',(-2.07535525905765,3.34086658648647,37.8272773992083));
#28345=CARTESIAN_POINT('Ctrl Pts',(-2.04824561392128,3.35770717055305,37.8256543642614));
#28346=CARTESIAN_POINT('Ctrl Pts',(-2.02094288135367,3.37421036309901,37.8240313293146));
#28347=CARTESIAN_POINT('Ctrl Pts',(-1.99345630322199,3.39037180367353,37.8224082943678));
#28348=CARTESIAN_POINT('Ctrl Pts',(-1.89401014270797,3.44884373152909,37.8165361704145));
#28349=CARTESIAN_POINT('Ctrl Pts',(-1.79182243863938,3.5030345546936,37.8106640464611));
#28350=CARTESIAN_POINT('Ctrl Pts',(-1.68729798416966,3.55267709095789,37.8047919225078));
#28351=CARTESIAN_POINT('Ctrl Pts',(-1.58290904772492,3.60225526469091,37.7989274118794));
#28352=CARTESIAN_POINT('Ctrl Pts',(-1.47618975572388,3.64729670268684,37.7930629012511));
#28353=CARTESIAN_POINT('Ctrl Pts',(-1.36757205913616,3.68757856364716,37.7871983906227));
#28354=CARTESIAN_POINT('Ctrl Pts',(-1.25906612907142,3.72781897497561,37.7813399145171));
#28355=CARTESIAN_POINT('Ctrl Pts',(-1.14866606518523,3.76330940785714,37.7754814384116));
#28356=CARTESIAN_POINT('Ctrl Pts',(-1.03682588890287,3.79387415132616,37.769622962306));
#28357=CARTESIAN_POINT('Ctrl Pts',(-0.920575705995505,3.82564410320659,
37.7635334787101));
#28358=CARTESIAN_POINT('Ctrl Pts',(-0.802769914156219,3.85209172586888,
37.7574439951142));
#28359=CARTESIAN_POINT('Ctrl Pts',(-0.683938671629199,3.87307589564807,
37.7513545115183));
#28360=CARTESIAN_POINT('Ctrl Pts',(-0.569747881856857,3.89324061722167,
37.7455028270089));
#28361=CARTESIAN_POINT('Ctrl Pts',(-0.454610673238863,3.90836050408855,
37.7396511424996));
#28362=CARTESIAN_POINT('Ctrl Pts',(-0.339009367189832,3.91836211304641,
37.7337994579902));
#28363=CARTESIAN_POINT('Ctrl Pts',(-0.22342569284546,3.92836219654214,37.7279486659896));
#28364=CARTESIAN_POINT('Ctrl Pts',(-0.107378473573039,3.93324551867752,
37.722097873989));
#28365=CARTESIAN_POINT('Ctrl Pts',(0.00864472130136986,3.93299049945377,
37.7162470819884));
#28366=CARTESIAN_POINT('Ctrl Pts',(0.124678322130959,3.93273545735771,37.7103957652385));
#28367=CARTESIAN_POINT('Ctrl Pts',(0.240687480842907,3.92734115868281,37.7045444484887));
#28368=CARTESIAN_POINT('Ctrl Pts',(0.356185216416442,3.91683814978439,37.6986931317389));
#28369=CARTESIAN_POINT('Ctrl Pts',(0.47172128554553,3.9063316549503,37.6928398729442));
#28370=CARTESIAN_POINT('Ctrl Pts',(0.58674518252168,3.8907131157734,37.6869866141496));
#28371=CARTESIAN_POINT('Ctrl Pts',(0.700776341941089,3.87006479513918,37.681133355355));
#28372=CARTESIAN_POINT('Ctrl Pts',(0.814937234059575,3.84939298301035,37.6752734373361));
#28373=CARTESIAN_POINT('Ctrl Pts',(0.928102727263476,3.82368004145433,37.6694135193172));
#28374=CARTESIAN_POINT('Ctrl Pts',(1.03980362436883,3.79305911142305,37.6635536012984));
#28375=CARTESIAN_POINT('Ctrl Pts',(1.15157973289209,3.76241756344129,37.6576897376286));
#28376=CARTESIAN_POINT('Ctrl Pts',(1.26188888917317,3.72686157322114,37.6518258739589));
#28377=CARTESIAN_POINT('Ctrl Pts',(1.37027986241766,3.68657321894637,37.6459620102891));
#28378=CARTESIAN_POINT('Ctrl Pts',(1.47883073841939,3.64622542965834,37.64008949601));
#28379=CARTESIAN_POINT('Ctrl Pts',(1.5854574043302,3.6011315032136,37.6342169817309));
#28380=CARTESIAN_POINT('Ctrl Pts',(1.68973121106261,3.55152043980615,37.6283444674517));
#28381=CARTESIAN_POINT('Ctrl Pts',(1.7185502575496,3.53780900462016,37.6267214303026));
#28382=CARTESIAN_POINT('Ctrl Pts',(1.74718974257687,3.52375278791357,37.6250983931535));
#28383=CARTESIAN_POINT('Ctrl Pts',(1.7756410032213,3.50935721004278,37.6234753560044));
#28384=CARTESIAN_POINT('Ctrl Pts',(1.87857723493968,3.45727422651714,37.6176032320885));
#28385=CARTESIAN_POINT('Ctrl Pts',(1.97939255308003,3.40057110844653,37.6117311081726));
#28386=CARTESIAN_POINT('Ctrl Pts',(2.07764341029815,3.33944409440324,37.6058589842567));
#28387=CARTESIAN_POINT('Ctrl Pts',(2.17576688331402,3.27839633275672,37.5999944736669));
#28388=CARTESIAN_POINT('Ctrl Pts',(2.27133215960027,3.21293629767389,37.5941299630771));
#28389=CARTESIAN_POINT('Ctrl Pts',(2.36391832744339,3.14330703896028,37.5882654524874));
#28390=CARTESIAN_POINT('Ctrl Pts',(2.45640922502803,3.07374942807084,37.5824069764215));
#28391=CARTESIAN_POINT('Ctrl Pts',(2.54592678312613,3.00003137372826,37.5765485003556));
#28392=CARTESIAN_POINT('Ctrl Pts',(2.63207782173528,2.92243996351152,37.5706900242897));
#28393=CARTESIAN_POINT('Ctrl Pts',(2.72162591098664,2.84178902024491,37.5646005406793));
#28394=CARTESIAN_POINT('Ctrl Pts',(2.8075361396623,2.75695321399475,37.5585110570689));
#28395=CARTESIAN_POINT('Ctrl Pts',(2.88940329059112,2.66830238622259,37.5524215734586));
#28396=CARTESIAN_POINT('Ctrl Pts',(2.96807346463353,2.583113443274,37.5465698889915));
#28397=CARTESIAN_POINT('Ctrl Pts',(3.0430100991615,2.49440217895448,37.5407182045244));
#28398=CARTESIAN_POINT('Ctrl Pts',(3.11389077470868,2.4025347537932,37.5348665200573));
#28399=CARTESIAN_POINT('Ctrl Pts',(3.18476063940591,2.31068134041921,37.5290157280998));
#28400=CARTESIAN_POINT('Ctrl Pts',(3.25157552266725,2.21567305056715,37.5231649361423));
#28401=CARTESIAN_POINT('Ctrl Pts',(3.31405380919675,2.11790848474349,37.5173141441848));
#28402=CARTESIAN_POINT('Ctrl Pts',(3.3765376993061,2.02013515056877,37.5114628274789));
#28403=CARTESIAN_POINT('Ctrl Pts',(3.43468399686684,1.91960539737308,37.505611510773));
#28404=CARTESIAN_POINT('Ctrl Pts',(3.48825526576596,1.81674549699621,37.4997601940671));
#28405=CARTESIAN_POINT('Ctrl Pts',(3.54184431489582,1.71385145755939,37.4939069353172));
#28406=CARTESIAN_POINT('Ctrl Pts',(3.59085512516964,1.60862609961033,37.4880536765674));
#28407=CARTESIAN_POINT('Ctrl Pts',(3.63509724358918,1.501518241531,37.4822004178175));
#28408=CARTESIAN_POINT('Ctrl Pts',(3.67938969604625,1.39428852737559,37.4763404998443));
#28409=CARTESIAN_POINT('Ctrl Pts',(3.71890246993564,1.28517242061843,37.4704805818711));
#28410=CARTESIAN_POINT('Ctrl Pts',(3.75349406598325,1.17463666579437,37.464620663898));
#28411=CARTESIAN_POINT('Ctrl Pts',(3.78810895354121,1.06402648408717,37.4587568002745));
#28412=CARTESIAN_POINT('Ctrl Pts',(3.81779595965542,0.951995149594837,37.4528929366511));
#28413=CARTESIAN_POINT('Ctrl Pts',(3.84246447098273,0.839020732303683,37.4470290730277));
#28414=CARTESIAN_POINT('Ctrl Pts',(3.86716937429586,0.725879650581997,37.4411565587954));
#28415=CARTESIAN_POINT('Ctrl Pts',(3.88684093685391,0.611793115212634,37.4352840445631));
#28416=CARTESIAN_POINT('Ctrl Pts',(3.90144022942924,0.497245549191858,37.4294115303309));
#28417=CARTESIAN_POINT('Ctrl Pts',(3.9054751622212,0.465587047384892,37.4277884927676));
#28418=CARTESIAN_POINT('Ctrl Pts',(3.90912295559818,0.433893334164532,37.4261654552043));
#28419=CARTESIAN_POINT('Ctrl Pts',(3.9123834894837,0.402174627761775,37.424542417641));
#28420=CARTESIAN_POINT('Ctrl Pts',(3.92602993472042,0.269421034300653,37.417749452439));
#28421=CARTESIAN_POINT('Ctrl Pts',(3.93292115709448,0.135961246390276,37.410956487237));
#28422=CARTESIAN_POINT('Ctrl Pts',(3.93299932738369,0.00230017378215415,
37.404163522035));
#28423=CARTESIAN_POINT('',(3.93121085245411,0.00231623353798856,36.1541640353064));
#28424=CARTESIAN_POINT('Ctrl Pts',(3.9378436511043,0.00226769081060172,
37.4041617293967));
#28425=CARTESIAN_POINT('Ctrl Pts',(3.92969352726255,-1.17026837568043,37.3446443126903));
#28426=CARTESIAN_POINT('Ctrl Pts',(2.75095850512379,-3.66336727924014,37.2188159165294));
#28427=CARTESIAN_POINT('Ctrl Pts',(-1.49285278529501,-4.40632793330521,
37.026676540914));
#28428=CARTESIAN_POINT('Ctrl Pts',(-4.51432818846032,-1.12480055766829,
36.8277436025506));
#28429=CARTESIAN_POINT('Ctrl Pts',(-3.38576122948677,3.19076106622442,36.6288106641873));
#28430=CARTESIAN_POINT('Ctrl Pts',(0.855351370873146,4.57304158308359,36.4298777258236));
#28431=CARTESIAN_POINT('Ctrl Pts',(3.60300821559048,2.32885918759836,36.2716625040733));
#28432=CARTESIAN_POINT('Ctrl Pts',(3.93054449524549,0.509825557930273,36.1797582617771));
#28433=CARTESIAN_POINT('Ctrl Pts',(3.92785313095816,0.00233337176097839,
36.1541649989355));
#28434=CARTESIAN_POINT('',(3.93198289809596,-0.0031156214140876,34.9041631193534));
#28435=CARTESIAN_POINT('Ctrl Pts',(3.93299932332396,0.0023071049629667,
36.154163522035));
#28436=CARTESIAN_POINT('Ctrl Pts',(3.93306815257745,-0.11502843536642,36.1482539137099));
#28437=CARTESIAN_POINT('Ctrl Pts',(3.92788182847184,-0.232374625365518,
36.1423443053847));
#28438=CARTESIAN_POINT('Ctrl Pts',(3.91746406086123,-0.349233921406056,
36.1364346970596));
#28439=CARTESIAN_POINT('Ctrl Pts',(3.90704445346722,-0.466113854861418,
36.1305240450945));
#28440=CARTESIAN_POINT('Ctrl Pts',(3.89139159917373,-0.582506322944185,
36.1246133931293));
#28441=CARTESIAN_POINT('Ctrl Pts',(3.87058107839869,-0.697919132523272,
36.1187027411642));
#28442=CARTESIAN_POINT('Ctrl Pts',(3.84976222824505,-0.813378135899996,
36.1127897234698));
#28443=CARTESIAN_POINT('Ctrl Pts',(3.82378167424935,-0.927856305137044,
36.1068767057753));
#28444=CARTESIAN_POINT('Ctrl Pts',(3.79276595892408,-1.04087241332774,36.1009636880809));
#28445=CARTESIAN_POINT('Ctrl Pts',(3.76170851327563,-1.15404057987561,36.0950427146732));
#28446=CARTESIAN_POINT('Ctrl Pts',(3.72560248091587,-1.26574236800933,36.0891217412655));
#28447=CARTESIAN_POINT('Ctrl Pts',(3.68462423432077,-1.37551199626033,36.0832007678578));
#28448=CARTESIAN_POINT('Ctrl Pts',(3.64361753378841,-1.48535784490568,36.0772756831222));
#28449=CARTESIAN_POINT('Ctrl Pts',(3.59773203505403,-1.59326849094606,36.0713505983866));
#28450=CARTESIAN_POINT('Ctrl Pts',(3.54719143757431,-1.69880013692002,36.0654255136511));
#28451=CARTESIAN_POINT('Ctrl Pts',(3.49655766018267,-1.80452634785695,36.0594895050464));
#28452=CARTESIAN_POINT('Ctrl Pts',(3.4412518234525,-1.90786443959993,36.0535534964416));
#28453=CARTESIAN_POINT('Ctrl Pts',(3.38154295267334,-2.00839643975617,36.0476174878369));
#28454=CARTESIAN_POINT('Ctrl Pts',(3.32921850769105,-2.09649526062636,36.0424156082569));
#28455=CARTESIAN_POINT('Ctrl Pts',(3.27351353645545,-2.18243944889097,36.0372137286769));
#28456=CARTESIAN_POINT('Ctrl Pts',(3.21463464360123,-2.26596847024816,36.0320118490969));
#28457=CARTESIAN_POINT('Ctrl Pts',(3.14816940685497,-2.36025992021537,36.026139725131));
#28458=CARTESIAN_POINT('Ctrl Pts',(3.07744059861696,-2.45178263820824,36.0202676011652));
#28459=CARTESIAN_POINT('Ctrl Pts',(3.00270672808036,-2.54012623803246,36.0143954771994));
#28460=CARTESIAN_POINT('Ctrl Pts',(2.92806975149084,-2.62835529862533,36.0085309665588));
#28461=CARTESIAN_POINT('Ctrl Pts',(2.84943830341971,-2.71341312508545,36.0026664559183));
#28462=CARTESIAN_POINT('Ctrl Pts',(2.7671139252641,-2.79491851842044,35.9968019452778));
#28463=CARTESIAN_POINT('Ctrl Pts',(2.68487425807463,-2.87634004351652,35.9909434691604));
#28464=CARTESIAN_POINT('Ctrl Pts',(2.59894951117365,-2.95421611717767,35.985084993043));
#28465=CARTESIAN_POINT('Ctrl Pts',(2.50968077474067,-3.02819936742894,35.9792265169256));
#28466=CARTESIAN_POINT('Ctrl Pts',(2.41689205377746,-3.1050998752419,35.9731370333342));
#28467=CARTESIAN_POINT('Ctrl Pts',(2.32049049587995,-3.17779389798758,35.9670475497429));
#28468=CARTESIAN_POINT('Ctrl Pts',(2.22090081590631,-3.24593415920698,35.9609580661516));
#28469=CARTESIAN_POINT('Ctrl Pts',(2.12520019040444,-3.31141349022082,35.9551063816313));
#28470=CARTESIAN_POINT('Ctrl Pts',(2.02655614087375,-3.37268778603635,35.9492546971111));
#28471=CARTESIAN_POINT('Ctrl Pts',(1.92537772850614,-3.42949115796681,35.9434030125909));
#28472=CARTESIAN_POINT('Ctrl Pts',(1.8242147480458,-3.48628586614828,35.9375522205798));
#28473=CARTESIAN_POINT('Ctrl Pts',(1.72051853370941,-3.53861080397351,35.9317014285687));
#28474=CARTESIAN_POINT('Ctrl Pts',(1.61472432391119,-3.58624516141459,35.9258506365576));
#28475=CARTESIAN_POINT('Ctrl Pts',(1.50892062558798,-3.63388379111019,35.9199993197976));
#28476=CARTESIAN_POINT('Ctrl Pts',(1.40101893473241,-3.67683083438635,35.9141480030377));
#28477=CARTESIAN_POINT('Ctrl Pts',(1.29147545916237,-3.71491320738202,35.9082966862778));
#28478=CARTESIAN_POINT('Ctrl Pts',(1.18189562625586,-3.75300821986755,35.9024434274734));
#28479=CARTESIAN_POINT('Ctrl Pts',(1.07067331540675,-3.78623521590995,35.8965901686691));
#28480=CARTESIAN_POINT('Ctrl Pts',(0.958280226486698,-3.81447086861659,
35.8907369098648));
#28481=CARTESIAN_POINT('Ctrl Pts',(0.845759268505086,-3.84273864488571,
35.8848769918369));
#28482=CARTESIAN_POINT('Ctrl Pts',(0.732065275031789,-3.86600364264212,
35.8790170738089));
#28483=CARTESIAN_POINT('Ctrl Pts',(0.617680580600549,-3.88419357143139,
35.873157155781));
#28484=CARTESIAN_POINT('Ctrl Pts',(0.503218867680946,-3.90239574802031,
35.8672932921026));
#28485=CARTESIAN_POINT('Ctrl Pts',(0.388065937513293,-3.91551600466352,
35.8614294284241));
#28486=CARTESIAN_POINT('Ctrl Pts',(0.272707948110416,-3.92353404152907,
35.8555655647457));
#28487=CARTESIAN_POINT('Ctrl Pts',(0.1571797779379,-3.93156390692675,35.8496930504585));
#28488=CARTESIAN_POINT('Ctrl Pts',(0.0414463565074991,-3.93447651968868,
35.8438205361713));
#28489=CARTESIAN_POINT('Ctrl Pts',(-0.0740073703216252,-3.93230363898035,
35.8379480218841));
#28490=CARTESIAN_POINT('Ctrl Pts',(-0.105916305245342,-3.93170310133619,
35.8363249848339));
#28491=CARTESIAN_POINT('Ctrl Pts',(-0.137803915726344,-3.93071441185742,
35.8347019477837));
#28492=CARTESIAN_POINT('Ctrl Pts',(-0.169660074222265,-3.929338934123,35.8330789107334));
#28493=CARTESIAN_POINT('Ctrl Pts',(-0.284915182996696,-3.92436247608846,
35.8272067867675));
#28494=CARTESIAN_POINT('Ctrl Pts',(-0.400144376111135,-3.91430239267515,
35.8213346628015));
#28495=CARTESIAN_POINT('Ctrl Pts',(-0.514862652605059,-3.89915445307729,
35.8154625388356));
#28496=CARTESIAN_POINT('Ctrl Pts',(-0.62943219457563,-3.8840261530839,35.8095980281949));
#28497=CARTESIAN_POINT('Ctrl Pts',(-0.743491731159177,-3.86382316858314,
35.8037335175543));
#28498=CARTESIAN_POINT('Ctrl Pts',(-0.856557568373406,-3.83859324910341,
35.7978690069137));
#28499=CARTESIAN_POINT('Ctrl Pts',(-0.969507061966085,-3.81338929095979,
35.7920105307961));
#28500=CARTESIAN_POINT('Ctrl Pts',(-1.08146448894426,-3.78316877600975,
35.7861520546786));
#28501=CARTESIAN_POINT('Ctrl Pts',(-1.19195324869756,-3.7480310101331,35.7802935785611));
#28502=CARTESIAN_POINT('Ctrl Pts',(-1.30679872660717,-3.71150771560258,
35.7742040949698));
#28503=CARTESIAN_POINT('Ctrl Pts',(-1.4200568803427,-3.66967146433403,35.7681146113785));
#28504=CARTESIAN_POINT('Ctrl Pts',(-1.5312060032593,-3.62269197912032,35.7620251277872));
#28505=CARTESIAN_POINT('Ctrl Pts',(-1.63801466646809,-3.57754707934744,
35.7561734432669));
#28506=CARTESIAN_POINT('Ctrl Pts',(-1.74287550973644,-3.52765327827911,
35.7503217587465));
#28507=CARTESIAN_POINT('Ctrl Pts',(-1.84534376791724,-3.47321110475724,
35.7444700742262));
#28508=CARTESIAN_POINT('Ctrl Pts',(-1.94779639746115,-3.41877723485033,
35.738619282215));
#28509=CARTESIAN_POINT('Ctrl Pts',(-2.0478568025135,-3.35979656575146,35.7327684902038));
#28510=CARTESIAN_POINT('Ctrl Pts',(-2.14510400419289,-3.29651601106314,
35.7269176981926));
#28511=CARTESIAN_POINT('Ctrl Pts',(-2.24235992782914,-3.233229780836,35.7210663814325));
#28512=CARTESIAN_POINT('Ctrl Pts',(-2.33680179998934,-3.16564312387548,
35.7152150646724));
#28513=CARTESIAN_POINT('Ctrl Pts',(-2.42803746981478,-3.09404638704326,
35.7093637479124));
#28514=CARTESIAN_POINT('Ctrl Pts',(-2.51930342063967,-3.02242588734775,
35.703510489108));
#28515=CARTESIAN_POINT('Ctrl Pts',(-2.60736072811292,-2.94679291637804,
35.6976572303035));
#28516=CARTESIAN_POINT('Ctrl Pts',(-2.69185073787341,-2.86747774272276,
35.6918039714991));
#28517=CARTESIAN_POINT('Ctrl Pts',(-2.77643687150012,-2.78807233258669,
35.6859440534711));
#28518=CARTESIAN_POINT('Ctrl Pts',(-2.85744730517025,-2.70497664130493,
35.680084135443));
#28519=CARTESIAN_POINT('Ctrl Pts',(-2.93456058230027,-2.61855746333921,
35.674224217415));
#28520=CARTESIAN_POINT('Ctrl Pts',(-3.01172578200672,-2.53208009686771,
35.6683603537365));
#28521=CARTESIAN_POINT('Ctrl Pts',(-3.08498833944942,-2.44227510737343,
35.6624964900579));
#28522=CARTESIAN_POINT('Ctrl Pts',(-3.15406847912027,-2.34954059956834,
35.6566326263794));
#28523=CARTESIAN_POINT('Ctrl Pts',(-3.22325052860603,-2.25666928606813,
35.6507601120921));
#28524=CARTESIAN_POINT('Ctrl Pts',(-3.28823761480356,-2.16086016971041,
35.6448875978048));
#28525=CARTESIAN_POINT('Ctrl Pts',(-3.34879442180649,-2.06253846521167,
35.6390150835175));
#28526=CARTESIAN_POINT('Ctrl Pts',(-3.36553102499484,-2.0353644539908,35.6373920464683));
#28527=CARTESIAN_POINT('Ctrl Pts',(-3.38192949838553,-2.00799864908361,
35.6357690094191));
#28528=CARTESIAN_POINT('Ctrl Pts',(-3.39798551695636,-1.9804503090345,35.63414597237));
#28529=CARTESIAN_POINT('Ctrl Pts',(-3.45607595395473,-1.88078082341616,
35.6282738484039));
#28530=CARTESIAN_POINT('Ctrl Pts',(-3.50987481252454,-1.77838621886318,
35.6224017244377));
#28531=CARTESIAN_POINT('Ctrl Pts',(-3.55911646351883,-1.67367230935725,
35.6165296004716));
#28532=CARTESIAN_POINT('Ctrl Pts',(-3.60829427173484,-1.56909416351423,
35.6106650898308));
#28533=CARTESIAN_POINT('Ctrl Pts',(-3.65292644795823,-1.46220306325422,
35.60480057919));
#28534=CARTESIAN_POINT('Ctrl Pts',(-3.69279180769145,-1.35343181026859,
35.5989360685492));
#28535=CARTESIAN_POINT('Ctrl Pts',(-3.73261614636621,-1.24477248181989,
35.5930775924314));
#28536=CARTESIAN_POINT('Ctrl Pts',(-3.76768328343449,-1.13423723459942,
35.5872191163137));
#28537=CARTESIAN_POINT('Ctrl Pts',(-3.79781924895605,-1.02228075999645,
35.581360640196));
#28538=CARTESIAN_POINT('Ctrl Pts',(-3.82914351551647,-0.905909693301426,
35.5752711566048));
#28539=CARTESIAN_POINT('Ctrl Pts',(-3.8551395311012,-0.788003423404034,
35.5691816730135));
#28540=CARTESIAN_POINT('Ctrl Pts',(-3.87566820456159,-0.669092645416404,
35.5630921894223));
#28541=CARTESIAN_POINT('Ctrl Pts',(-3.89539521735587,-0.554825425799626,
35.5572405049018));
#28542=CARTESIAN_POINT('Ctrl Pts',(-3.91007380593832,-0.439631125272265,
35.5513888203813));
#28543=CARTESIAN_POINT('Ctrl Pts',(-3.91963237582199,-0.323992343131811,
35.5455371358608));
#28544=CARTESIAN_POINT('Ctrl Pts',(-3.92918948781598,-0.208371198419347,
35.5396863438494));
#28545=CARTESIAN_POINT('Ctrl Pts',(-3.93362809976647,-0.0923061187816158,
35.533835551838));
#28546=CARTESIAN_POINT('Ctrl Pts',(-3.93292850011839,0.0237152473421576,
35.5279847598265));
#28547=CARTESIAN_POINT('Ctrl Pts',(-3.93222883772426,0.139747019249488,
35.5221334430663));
#28548=CARTESIAN_POINT('Ctrl Pts',(-3.92639005011987,0.255734656419345,
35.5162821263061));
#28549=CARTESIAN_POINT('Ctrl Pts',(-3.91544454946725,0.371191298452989,
35.5104308095458));
#28550=CARTESIAN_POINT('Ctrl Pts',(-3.90449541601719,0.486686260396046,
35.5045775507412));
#28551=CARTESIAN_POINT('Ctrl Pts',(-3.88843623829481,0.601649465418135,
35.4987242919365));
#28552=CARTESIAN_POINT('Ctrl Pts',(-3.86735112002908,0.715600666859522,
35.4928710331318));
#28553=CARTESIAN_POINT('Ctrl Pts',(-3.84624201332869,0.829681510018675,
35.4870111151036));
#28554=CARTESIAN_POINT('Ctrl Pts',(-3.82009562839742,0.942747644775464,
35.4811511970754));
#28555=CARTESIAN_POINT('Ctrl Pts',(-3.78904690309602,1.05433038756286,35.4752912790471));
#28556=CARTESIAN_POINT('Ctrl Pts',(-3.75797727179921,1.16598826220463,35.4694274153684));
#28557=CARTESIAN_POINT('Ctrl Pts',(-3.72199885544546,1.27616036402106,35.4635635516896));
#28558=CARTESIAN_POINT('Ctrl Pts',(-3.68129545992388,1.38439616322202,35.4576996880109));
#28559=CARTESIAN_POINT('Ctrl Pts',(-3.64053201710782,1.49279163624931,35.4518271737234));
#28560=CARTESIAN_POINT('Ctrl Pts',(-3.59502984521864,1.59924472687513,35.4459546594359));
#28561=CARTESIAN_POINT('Ctrl Pts',(-3.54501958528189,1.7033276666478,35.4400821451484));
#28562=CARTESIAN_POINT('Ctrl Pts',(-3.53119782161342,1.73209395974999,35.4384591081011));
#28563=CARTESIAN_POINT('Ctrl Pts',(-3.51703196704843,1.76067937158613,35.4368360710538));
#28564=CARTESIAN_POINT('Ctrl Pts',(-3.50252747509735,1.78907526006822,35.4352130340065));
#28565=CARTESIAN_POINT('Ctrl Pts',(-3.45005043833285,1.89181116346021,35.4293409100405));
#28566=CARTESIAN_POINT('Ctrl Pts',(-3.39296142786934,1.99240846515638,35.4234687860746));
#28567=CARTESIAN_POINT('Ctrl Pts',(-3.331458380452,2.09042437302002,35.4175966621086));
#28568=CARTESIAN_POINT('Ctrl Pts',(-3.27003507295682,2.18831320131295,35.4117321514679));
#28569=CARTESIAN_POINT('Ctrl Pts',(-3.20420932695427,2.28362694445509,35.4058676408272));
#28570=CARTESIAN_POINT('Ctrl Pts',(-3.13422580334255,2.37594562514839,35.4000031301866));
#28571=CARTESIAN_POINT('Ctrl Pts',(-3.06431429208025,2.46816931083786,35.394144654069));
#28572=CARTESIAN_POINT('Ctrl Pts',(-2.99025376121517,2.5574037366363,35.3882861779514));
#28573=CARTESIAN_POINT('Ctrl Pts',(-2.91233280283166,2.64325682549969,35.3824277018339));
#28574=CARTESIAN_POINT('Ctrl Pts',(-2.83133931784156,2.73249521538173,35.3763382182426));
#28575=CARTESIAN_POINT('Ctrl Pts',(-2.74617494034244,2.81807973566952,35.3702487346513));
#28576=CARTESIAN_POINT('Ctrl Pts',(-2.65721106180506,2.89960658935326,35.36415925106));
#28577=CARTESIAN_POINT('Ctrl Pts',(-2.57172129192485,2.97794975598523,35.3583075665397));
#28578=CARTESIAN_POINT('Ctrl Pts',(-2.48272353281795,3.05254591346051,35.3524558820193));
#28579=CARTESIAN_POINT('Ctrl Pts',(-2.39058517779383,3.12307404774726,35.346604197499));
#28580=CARTESIAN_POINT('Ctrl Pts',(-2.29846087587175,3.19359142496039,35.3407534054877));
#28581=CARTESIAN_POINT('Ctrl Pts',(-2.20319725864039,3.26004176144352,35.3349026134764));
#28582=CARTESIAN_POINT('Ctrl Pts',(-2.10519400279285,3.32214497134081,35.3290518214652));
#28583=CARTESIAN_POINT('Ctrl Pts',(-2.00718195717924,3.38425375118251,35.3232005047051));
#28584=CARTESIAN_POINT('Ctrl Pts',(-1.90643013371653,3.44201440808012,35.317349187945));
#28585=CARTESIAN_POINT('Ctrl Pts',(-1.80336571094006,3.49519114106877,35.3114978711849));
#28586=CARTESIAN_POINT('Ctrl Pts',(-1.70026708121687,3.54838552334535,35.3056446123805));
#28587=CARTESIAN_POINT('Ctrl Pts',(-1.59485469315812,3.59699276705317,35.2997913535761));
#28588=CARTESIAN_POINT('Ctrl Pts',(-1.48757809164367,3.64082414039209,35.2939380947716));
#28589=CARTESIAN_POINT('Ctrl Pts',(-1.38017944206958,3.68470538046795,35.2880781767436));
#28590=CARTESIAN_POINT('Ctrl Pts',(-1.27091272869601,3.72379974862621,35.2822182587155));
#28591=CARTESIAN_POINT('Ctrl Pts',(-1.16024523484106,3.75796753512169,35.2763583406874));
#28592=CARTESIAN_POINT('Ctrl Pts',(-1.04950322539493,3.79215832776579,35.2704944770088));
#28593=CARTESIAN_POINT('Ctrl Pts',(-0.937358956447254,3.82141582942803,
35.2646306133302));
#28594=CARTESIAN_POINT('Ctrl Pts',(-0.824290841697528,3.84565125931793,
35.2587667496516));
#28595=CARTESIAN_POINT('Ctrl Pts',(-0.711055924294302,3.86992244229369,
35.2528942353643));
#28596=CARTESIAN_POINT('Ctrl Pts',(-0.596894847145015,3.88915669855326,
35.2470217210769));
#28597=CARTESIAN_POINT('Ctrl Pts',(-0.482292178867151,3.90331695538597,
35.2411492067896));
#28598=CARTESIAN_POINT('Ctrl Pts',(-0.450618458309539,3.90723054679429,
35.2395261697408));
#28599=CARTESIAN_POINT('Ctrl Pts',(-0.418911010076204,3.9107568669515,35.237903132692));
#28600=CARTESIAN_POINT('Ctrl Pts',(-0.387180052773377,3.91389583493664,
35.2362800956432));
#28601=CARTESIAN_POINT('Ctrl Pts',(-0.272377919957184,3.92525257454261,
35.2304079716771));
#28602=CARTESIAN_POINT('Ctrl Pts',(-0.156883226493117,3.93157301805287,
35.2245358477111));
#28603=CARTESIAN_POINT('Ctrl Pts',(-0.0411755108716569,3.93278445599355,
35.2186637237451));
#28604=CARTESIAN_POINT('Ctrl Pts',(0.0743821873989408,3.93399432328088,
35.2127992131043));
#28605=CARTESIAN_POINT('Ctrl Pts',(0.190151949021274,3.93010835329838,35.2069347024636));
#28606=CARTESIAN_POINT('Ctrl Pts',(0.305648185573892,3.92110548017461,35.2010701918229));
#28607=CARTESIAN_POINT('Ctrl Pts',(0.421025577648148,3.91211187091772,35.1952117157053));
#28608=CARTESIAN_POINT('Ctrl Pts',(0.536129594798534,3.89801186327134,35.1893532395877));
#28609=CARTESIAN_POINT('Ctrl Pts',(0.650474386927082,3.87883643274009,35.1834947634701));
#28610=CARTESIAN_POINT('Ctrl Pts',(0.769327945674206,3.85890488958256,35.1774052798788));
#28611=CARTESIAN_POINT('Ctrl Pts',(0.887360718078583,3.83348942291054,35.1713157962875));
#28612=CARTESIAN_POINT('Ctrl Pts',(1.00403225191212,3.80268434623757,35.1652263126963));
#28613=CARTESIAN_POINT('Ctrl Pts',(1.11614767159814,3.77308223176998,35.1593746281758));
#28614=CARTESIAN_POINT('Ctrl Pts',(1.22700573513248,3.73850366057662,35.1535229436554));
#28615=CARTESIAN_POINT('Ctrl Pts',(1.33613780774355,3.69908431354548,35.147671259135));
#28616=CARTESIAN_POINT('Ctrl Pts',(1.44525323534139,3.65967097882162,35.1418204671237));
#28617=CARTESIAN_POINT('Ctrl Pts',(1.55264280672405,3.61541847668629,35.1359696751124));
#28618=CARTESIAN_POINT('Ctrl Pts',(1.65785488154545,3.56651176806357,35.1301188831011));
#28619=CARTESIAN_POINT('Ctrl Pts',(1.76307639268116,3.51760067307098,35.1242675663409));
#28620=CARTESIAN_POINT('Ctrl Pts',(1.86611964411228,3.46403471605469,35.1184162495808));
#28621=CARTESIAN_POINT('Ctrl Pts',(1.9665553980936,3.40604592837926,35.1125649328206));
#28622=CARTESIAN_POINT('Ctrl Pts',(2.06702448656943,3.34803789430154,35.1067116740162));
#28623=CARTESIAN_POINT('Ctrl Pts',(2.16488399892109,3.2856043172812,35.1008584152117));
#28624=CARTESIAN_POINT('Ctrl Pts',(2.25973221776311,3.21902148237682,35.0950051564072));
#28625=CARTESIAN_POINT('Ctrl Pts',(2.35468834495526,3.15236289651,35.0891452383791));
#28626=CARTESIAN_POINT('Ctrl Pts',(2.44662600199921,3.08154586825698,35.083285320351));
#28627=CARTESIAN_POINT('Ctrl Pts',(2.53517513579142,3.00688809749631,35.0774254023229));
#28628=CARTESIAN_POINT('Ctrl Pts',(2.6237838922495,2.93218005752203,35.0715615386443));
#28629=CARTESIAN_POINT('Ctrl Pts',(2.70899927913946,2.85362640516535,35.0656976749657));
#28630=CARTESIAN_POINT('Ctrl Pts',(2.7904880828334,2.77158172521843,35.059833811287));
#28631=CARTESIAN_POINT('Ctrl Pts',(2.87209710210524,2.68941600964248,35.0539612969996));
#28632=CARTESIAN_POINT('Ctrl Pts',(2.94996828894454,2.60374929259172,35.0480887827122));
#28633=CARTESIAN_POINT('Ctrl Pts',(3.02380861326784,2.51496927820743,35.0422162684248));
#28634=CARTESIAN_POINT('Ctrl Pts',(3.04421649585048,2.49043238558347,35.0405932313765));
#28635=CARTESIAN_POINT('Ctrl Pts',(3.06431673688239,2.46565785193998,35.0389701943281));
#28636=CARTESIAN_POINT('Ctrl Pts',(3.08410374667262,2.44065423191404,35.0373471572797));
#28637=CARTESIAN_POINT('Ctrl Pts',(3.1556087869851,2.35029773657354,35.0314819289908));
#28638=CARTESIAN_POINT('Ctrl Pts',(3.22326457165389,2.25663831851123,35.0256167007019));
#28639=CARTESIAN_POINT('Ctrl Pts',(3.28674987154625,2.16003802788068,35.019751472413));
#28640=CARTESIAN_POINT('Ctrl Pts',(3.35015504965811,2.06355965188702,35.0138936463501));
#28641=CARTESIAN_POINT('Ctrl Pts',(3.40939998051885,1.96414812317378,35.0080358202871));
#28642=CARTESIAN_POINT('Ctrl Pts',(3.46420333166326,1.86219877480713,35.0021779942242));
#28643=CARTESIAN_POINT('Ctrl Pts',(3.51895084127202,1.76035330709835,34.9963261369569));
#28644=CARTESIAN_POINT('Ctrl Pts',(3.56926557482931,1.65597552318575,34.9904742796896));
#28645=CARTESIAN_POINT('Ctrl Pts',(3.61490963089598,1.54948938700964,34.9846224224223));
#28646=CARTESIAN_POINT('Ctrl Pts',(3.66051827221708,1.44308587231251,34.9787751055498));
#28647=CARTESIAN_POINT('Ctrl Pts',(3.70146328114283,1.33457763772048,34.9729277886773));
#28648=CARTESIAN_POINT('Ctrl Pts',(3.73755316320159,1.22441224766898,34.9670804718048));
#28649=CARTESIAN_POINT('Ctrl Pts',(3.7736264771196,1.1142974323377,34.9612358393182));
#28650=CARTESIAN_POINT('Ctrl Pts',(3.80484896667096,1.00252736656861,34.9553912068316));
#28651=CARTESIAN_POINT('Ctrl Pts',(3.8310778916543,0.889567978334213,34.949546574345));
#28652=CARTESIAN_POINT('Ctrl Pts',(3.85729952992758,0.77663997157318,34.9437035655674));
#28653=CARTESIAN_POINT('Ctrl Pts',(3.8785302727413,0.662523703250463,34.9378605567898));
#28654=CARTESIAN_POINT('Ctrl Pts',(3.89467792205645,0.54769780303198,34.9320175480122));
#28655=CARTESIAN_POINT('Ctrl Pts',(3.91082899833729,0.432847533667717,34.9261732991909));
#28656=CARTESIAN_POINT('Ctrl Pts',(3.92189476648159,0.317287741314481,34.9203290503697));
#28657=CARTESIAN_POINT('Ctrl Pts',(3.92783464354237,0.201504374613492,34.9144848015484));
#28658=CARTESIAN_POINT('Ctrl Pts',(3.93133136503697,0.133344346566134,34.9110443750439));
#28659=CARTESIAN_POINT('Ctrl Pts',(3.93305268568233,0.0651069405325119,
34.9076039485395));
#28660=CARTESIAN_POINT('Ctrl Pts',(3.93299877161876,-0.00310844740720695,
34.904163522035));
#28661=CARTESIAN_POINT('',(3.9391332139622,-0.00113435864636278,33.654163522035));
#28662=CARTESIAN_POINT('Ctrl Pts',(3.92939779249061,-0.0031338771959184,
34.9041620946445));
#28663=CARTESIAN_POINT('Ctrl Pts',(3.93258331200376,-0.437279526977727,
34.8822461360685));
#28664=CARTESIAN_POINT('Ctrl Pts',(3.66567225937177,-2.18120492678934,34.7940191980378));
#28665=CARTESIAN_POINT('Ctrl Pts',(1.1074941219487,-4.51860510079755,34.6394812805529));
#28666=CARTESIAN_POINT('Ctrl Pts',(-3.20371133310602,-3.37350989049275,
34.4405483421894));
#28667=CARTESIAN_POINT('Ctrl Pts',(-4.5697304411889,0.872868250080218,34.2416154038258));
#28668=CARTESIAN_POINT('Ctrl Pts',(-1.73477564576997,4.31681465272121,34.0426824654626));
#28669=CARTESIAN_POINT('Ctrl Pts',(2.62558860763858,3.80050871419932,33.8468651715321));
#28670=CARTESIAN_POINT('Ctrl Pts',(3.93440149740121,1.24278092515243,33.7173588570563));
#28671=CARTESIAN_POINT('Ctrl Pts',(3.9391332139622,-0.00113435864636278,
33.654163522035));
#28672=CARTESIAN_POINT('',(3.9329983150557,0.00364057262290602,32.404163522035));
#28673=CARTESIAN_POINT('Ctrl Pts',(3.9391332139622,-0.00113435864636278,
33.654163522035));
#28674=CARTESIAN_POINT('Ctrl Pts',(3.93936649615554,-0.0624616342740536,
33.6510478776019));
#28675=CARTESIAN_POINT('Ctrl Pts',(3.91022907276817,-1.42880496523826,33.5816212537148));
#28676=CARTESIAN_POINT('Ctrl Pts',(2.32725627739605,-4.02842568585283,33.4458836503718));
#28677=CARTESIAN_POINT('Ctrl Pts',(-2.13215816018169,-4.13500143495696,
33.2469507120089));
#28678=CARTESIAN_POINT('Ctrl Pts',(-4.63146993867469,-0.44025162607551,
33.0480177736453));
#28679=CARTESIAN_POINT('Ctrl Pts',(-2.8730504138422,3.65922349777118,32.8490848352818));
#28680=CARTESIAN_POINT('Ctrl Pts',(1.52657737641075,4.3947578773988,32.6501518969184));
#28681=CARTESIAN_POINT('Ctrl Pts',(3.76031183336374,1.93114587073444,32.5018448144934));
#28682=CARTESIAN_POINT('Ctrl Pts',(3.93572306029363,0.313664098688633,32.4198487115227));
#28683=CARTESIAN_POINT('Ctrl Pts',(3.93286077649292,0.00364174925168429,
32.4041635880065));
#28684=CARTESIAN_POINT('',(3.93054987827653,-0.000439589250792058,31.1541634039922));
#28685=CARTESIAN_POINT('Ctrl Pts',(3.9329983150557,0.00364057262290602,
32.404163522035));
#28686=CARTESIAN_POINT('Ctrl Pts',(3.93310415105304,-0.110696605159677,
32.3983789491121));
#28687=CARTESIAN_POINT('Ctrl Pts',(3.92821989213574,-0.225172602477814,
32.3925943761891));
#28688=CARTESIAN_POINT('Ctrl Pts',(3.91833602088708,-0.3393108124107,32.3868098032662));
#28689=CARTESIAN_POINT('Ctrl Pts',(3.90845907876316,-0.453369005326499,
32.3810292856396));
#28690=CARTESIAN_POINT('Ctrl Pts',(3.89358952894702,-0.567089459903584,
32.3752487680131));
#28691=CARTESIAN_POINT('Ctrl Pts',(3.87376992155456,-0.679996760918176,
32.3694682503865));
#28692=CARTESIAN_POINT('Ctrl Pts',(3.8539574981122,-0.792863136782181,32.3636898280058));
#28693=CARTESIAN_POINT('Ctrl Pts',(3.82919865527693,-0.904916526835692,
32.3579114056251));
#28694=CARTESIAN_POINT('Ctrl Pts',(3.79958757305406,-1.01568857170551,32.3521329832444));
#28695=CARTESIAN_POINT('Ctrl Pts',(3.76997962428042,-1.12644889466065,32.3463551723372));
#28696=CARTESIAN_POINT('Ctrl Pts',(3.73552056656729,-1.23592773163399,32.3405773614301));
#28697=CARTESIAN_POINT('Ctrl Pts',(3.69635507222063,-1.34366966925238,32.3347995505229));
#28698=CARTESIAN_POINT('Ctrl Pts',(3.65718367016728,-1.4514278586193,32.3290208680931));
#28699=CARTESIAN_POINT('Ctrl Pts',(3.61330456664536,-1.55744822906134,32.3232421856634));
#28700=CARTESIAN_POINT('Ctrl Pts',(3.56491110023304,-1.66129402799,32.3174635032337));
#28701=CARTESIAN_POINT('Ctrl Pts',(3.51646806002748,-1.76524620553847,32.3116789011782));
#28702=CARTESIAN_POINT('Ctrl Pts',(3.46350160308214,-1.86701897811158,32.3058942991228));
#28703=CARTESIAN_POINT('Ctrl Pts',(3.40625170290018,-1.96619895648677,32.3001096970673));
#28704=CARTESIAN_POINT('Ctrl Pts',(3.34897105225448,-2.06543220710031,32.2943219879463));
#28705=CARTESIAN_POINT('Ctrl Pts',(3.28740260695837,-2.16206953360629,32.2885342788252));
#28706=CARTESIAN_POINT('Ctrl Pts',(3.22182939718089,-2.25572700818628,32.2827465697042));
#28707=CARTESIAN_POINT('Ctrl Pts',(3.15615129373913,-2.3495343012017,32.2769496023202));
#28708=CARTESIAN_POINT('Ctrl Pts',(3.08645589152145,-2.4403518869279,32.2711526349362));
#28709=CARTESIAN_POINT('Ctrl Pts',(3.01306632916588,-2.52782916670546,32.2653556675522));
#28710=CARTESIAN_POINT('Ctrl Pts',(2.95791245091571,-2.59357027598109,32.260999118432));
#28711=CARTESIAN_POINT('Ctrl Pts',(2.90067299541346,-2.65742553068555,32.2566425693117));
#28712=CARTESIAN_POINT('Ctrl Pts',(2.84149790413252,-2.71926068276112,32.2522860201915));
#28713=CARTESIAN_POINT('Ctrl Pts',(2.76173673029731,-2.80260731065918,32.2464138962254));
#28714=CARTESIAN_POINT('Ctrl Pts',(2.67817165199454,-2.88258136840731,32.2405417722594));
#28715=CARTESIAN_POINT('Ctrl Pts',(2.59111938936618,-2.95881552484278,32.2346696482934));
#28716=CARTESIAN_POINT('Ctrl Pts',(2.50417999172485,-3.0349508421807,32.2288051376527));
#28717=CARTESIAN_POINT('Ctrl Pts',(2.41376270892944,-3.1073556309769,32.222940627012));
#28718=CARTESIAN_POINT('Ctrl Pts',(2.320222468961,-3.17569782796294,32.2170761163713));
#28719=CARTESIAN_POINT('Ctrl Pts',(2.22677848096878,-3.24396970150827,32.2112176402537));
#28720=CARTESIAN_POINT('Ctrl Pts',(2.13021825939134,-3.30818705577219,32.2053591641361));
#28721=CARTESIAN_POINT('Ctrl Pts',(2.03093080474347,-3.36805716494599,32.1995006880185));
#28722=CARTESIAN_POINT('Ctrl Pts',(1.92772831423915,-3.43028803183059,32.1934112044272));
#28723=CARTESIAN_POINT('Ctrl Pts',(1.82157943140423,-3.48782146541949,32.1873217208359));
#28724=CARTESIAN_POINT('Ctrl Pts',(1.71295583545349,-3.54037728297223,32.1812322372447));
#28725=CARTESIAN_POINT('Ctrl Pts',(1.60857407541615,-3.59088075496964,32.1753805527243));
#28726=CARTESIAN_POINT('Ctrl Pts',(1.50190766141388,-3.63678787816653,32.1695288682039));
#28727=CARTESIAN_POINT('Ctrl Pts',(1.3934006777869,-3.67789662050784,32.1636771836835));
#28728=CARTESIAN_POINT('Ctrl Pts',(1.28491024383368,-3.71899909287232,32.1578263916722));
#28729=CARTESIAN_POINT('Ctrl Pts',(1.17458018491985,-3.75530449311771,32.1519755996609));
#28730=CARTESIAN_POINT('Ctrl Pts',(1.06287376039485,-3.78665926239266,32.1461248076496));
#28731=CARTESIAN_POINT('Ctrl Pts',(0.95115731708683,-3.81801684383021,32.1402734908895));
#28732=CARTESIAN_POINT('Ctrl Pts',(0.838064660825857,-3.8444227999075,32.1344221741293));
#28733=CARTESIAN_POINT('Ctrl Pts',(0.724072682062405,-3.86577388773464,
32.1285708573692));
#28734=CARTESIAN_POINT('Ctrl Pts',(0.610042869510037,-3.88713206195994,
32.1227175985647));
#28735=CARTESIAN_POINT('Ctrl Pts',(0.495113547070775,-3.90343195585995,
32.1168643397602));
#28736=CARTESIAN_POINT('Ctrl Pts',(0.379769517664681,-3.91462183530577,
32.1110110809556));
#28737=CARTESIAN_POINT('Ctrl Pts',(0.264294261927041,-3.92582444542207,
32.1051511629275));
#28738=CARTESIAN_POINT('Ctrl Pts',(0.148403769228592,-3.93190539727357,
32.0992912448994));
#28739=CARTESIAN_POINT('Ctrl Pts',(0.0325857612234615,-3.93286500762046,
32.0934313268713));
#28740=CARTESIAN_POINT('Ctrl Pts',(-0.0833102303607444,-3.93382526410046,
32.0875674631927));
#28741=CARTESIAN_POINT('Ctrl Pts',(-0.199133227932258,-3.92965732757556,
32.0817035995141));
#28742=CARTESIAN_POINT('Ctrl Pts',(-0.314399468437188,-3.9204134953148,
32.0758397358355));
#28743=CARTESIAN_POINT('Ctrl Pts',(-0.429835754360515,-3.91115602617895,
32.0699672215482));
#28744=CARTESIAN_POINT('Ctrl Pts',(-0.544713235264734,-3.89680776736262,
32.0640947072608));
#28745=CARTESIAN_POINT('Ctrl Pts',(-0.658557096399692,-3.87747231463767,
32.0582221929734));
#28746=CARTESIAN_POINT('Ctrl Pts',(-0.69002109892269,-3.87212841003661,
32.056599155925));
#28747=CARTESIAN_POINT('Ctrl Pts',(-0.721406233175616,-3.86640385287236,
32.0549761188766));
#28748=CARTESIAN_POINT('Ctrl Pts',(-0.752702687445247,-3.8603014991465,
32.0533530818282));
#28749=CARTESIAN_POINT('Ctrl Pts',(-0.86593279476183,-3.83822327388462,
32.0474809578621));
#28750=CARTESIAN_POINT('Ctrl Pts',(-0.978380511693693,-3.81112192370885,
32.0416088338961));
#28751=CARTESIAN_POINT('Ctrl Pts',(-1.08956561142989,-3.77906546362846,
32.0357367099301));
#28752=CARTESIAN_POINT('Ctrl Pts',(-1.20060655747657,-3.74705056538509,
32.0298721992893));
#28753=CARTESIAN_POINT('Ctrl Pts',(-1.31038774818272,-3.71009344650441,
32.0240076886486));
#28754=CARTESIAN_POINT('Ctrl Pts',(-1.41843798709904,-3.66831332859591,
32.0181431780079));
#28755=CARTESIAN_POINT('Ctrl Pts',(-1.52637704339427,-3.62657620201317,
32.0122847018903));
#28756=CARTESIAN_POINT('Ctrl Pts',(-1.63258830738749,-3.58002609588318,
32.0064262257727));
#28757=CARTESIAN_POINT('Ctrl Pts',(-1.73661527179651,-3.52883215777729,
32.0005677496551));
#28758=CARTESIAN_POINT('Ctrl Pts',(-1.8447441572099,-3.47561957487862,31.9944782660638));
#28759=CARTESIAN_POINT('Ctrl Pts',(-1.9505125022498,-3.41738952683523,31.9883887824725));
#28760=CARTESIAN_POINT('Ctrl Pts',(-2.05342967864792,-3.35438750815225,
31.9822992988813));
#28761=CARTESIAN_POINT('Ctrl Pts',(-2.1523278592552,-3.29384576730398,31.9764476143609));
#28762=CARTESIAN_POINT('Ctrl Pts',(-2.24859298738348,-3.22889799641962,
31.9705959298404));
#28763=CARTESIAN_POINT('Ctrl Pts',(-2.3418151048469,-3.15980869906881,31.96474424532));
#28764=CARTESIAN_POINT('Ctrl Pts',(-2.43502300391103,-3.09072993933764,
31.9588934533087));
#28765=CARTESIAN_POINT('Ctrl Pts',(-2.52518848308879,-3.01751115519268,
31.9530426612974));
#28766=CARTESIAN_POINT('Ctrl Pts',(-2.61193201040197,-2.94045917724384,
31.947191869286));
#28767=CARTESIAN_POINT('Ctrl Pts',(-2.69868331761289,-2.86340028861788,
31.9413405525259));
#28768=CARTESIAN_POINT('Ctrl Pts',(-2.78201175374955,-2.78250779732479,
31.9354892357657));
#28769=CARTESIAN_POINT('Ctrl Pts',(-2.86157275925305,-2.69812719186863,
31.9296379190056));
#28770=CARTESIAN_POINT('Ctrl Pts',(-2.9411601709504,-2.61371858059968,31.923784660201));
#28771=CARTESIAN_POINT('Ctrl Pts',(-3.01697738220466,-2.52581985378752,
31.9179314013965));
#28772=CARTESIAN_POINT('Ctrl Pts',(-3.0887188995972,-2.43481099046128,31.912078142592));
#28773=CARTESIAN_POINT('Ctrl Pts',(-3.16054203695916,-2.34369858680147,
31.9062182245638));
#28774=CARTESIAN_POINT('Ctrl Pts',(-3.22827996925133,-2.24946930896179,
31.9003583065357));
#28775=CARTESIAN_POINT('Ctrl Pts',(-3.29166942371827,-2.15253371749626,
31.8944983885076));
#28776=CARTESIAN_POINT('Ctrl Pts',(-3.35510156011908,-2.05553285652273,
31.8886345248289));
#28777=CARTESIAN_POINT('Ctrl Pts',(-3.41417917834624,-1.9558224082933,31.8827706611503));
#28778=CARTESIAN_POINT('Ctrl Pts',(-3.46868488323865,-1.85383768998035,
31.8769067974716));
#28779=CARTESIAN_POINT('Ctrl Pts',(-3.52327099715044,-1.75170251968798,
31.8710342831842));
#28780=CARTESIAN_POINT('Ctrl Pts',(-3.57327155873323,-1.64728675463577,
31.8651617688968));
#28781=CARTESIAN_POINT('Ctrl Pts',(-3.61851717272685,-1.54104590154897,
31.8592892546094));
#28782=CARTESIAN_POINT('Ctrl Pts',(-3.63102209041432,-1.5116832074526,31.8576662175612));
#28783=CARTESIAN_POINT('Ctrl Pts',(-3.64316409482757,-1.48218119166648,
31.8560431805129));
#28784=CARTESIAN_POINT('Ctrl Pts',(-3.65494028738876,-1.45254965341036,
31.8544201434647));
#28785=CARTESIAN_POINT('Ctrl Pts',(-3.69754637739869,-1.34534318752482,
31.8485480194986));
#28786=CARTESIAN_POINT('Ctrl Pts',(-3.73550303719789,-1.23608082345837,
31.8426758955326));
#28787=CARTESIAN_POINT('Ctrl Pts',(-3.76860800799001,-1.12520339588607,
31.8368037715666));
#28788=CARTESIAN_POINT('Ctrl Pts',(-3.80167005753017,-1.01446972310021,
31.8309392609258));
#28789=CARTESIAN_POINT('Ctrl Pts',(-3.82989281002862,-0.902125543410319,
31.8250747502851));
#28790=CARTESIAN_POINT('Ctrl Pts',(-3.85312197359904,-0.788631762337931,
31.8192102396444));
#28791=CARTESIAN_POINT('Ctrl Pts',(-3.87632723459117,-0.675254765237539,
31.8133517635268));
#28792=CARTESIAN_POINT('Ctrl Pts',(-3.89454904468726,-0.560730922233132,
31.8074932874092));
#28793=CARTESIAN_POINT('Ctrl Pts',(-3.90768305905102,-0.445535756147207,
31.8016348112916));
#28794=CARTESIAN_POINT('Ctrl Pts',(-3.92133496499895,-0.325798292070669,
31.7955453277004));
#28795=CARTESIAN_POINT('Ctrl Pts',(-3.92948945333206,-0.205335909445877,
31.7894558441091));
#28796=CARTESIAN_POINT('Ctrl Pts',(-3.932087983519,-0.0846940958124628,
31.7833663605178));
#28797=CARTESIAN_POINT('Ctrl Pts',(-3.9345850390809,0.031236561159069,31.7775146759974));
#28798=CARTESIAN_POINT('Ctrl Pts',(-3.93195191279619,0.147332446022961,
31.771662991477));
#28799=CARTESIAN_POINT('Ctrl Pts',(-3.92418964905146,0.263105678915161,
31.7658113069566));
#28800=CARTESIAN_POINT('Ctrl Pts',(-3.91642856922069,0.378861253872504,
31.7599605149453));
#28801=CARTESIAN_POINT('Ctrl Pts',(-3.90353993504566,0.494293862333126,
31.754109722934));
#28802=CARTESIAN_POINT('Ctrl Pts',(-3.88557684738688,0.608918354996007,
31.7482589309227));
#28803=CARTESIAN_POINT('Ctrl Pts',(-3.86761214864552,0.723553128158945,
31.7424076141625));
#28804=CARTESIAN_POINT('Ctrl Pts',(-3.8445721556929,0.837379232991023,31.7365562974024));
#28805=CARTESIAN_POINT('Ctrl Pts',(-3.81656139502567,0.949920058741654,
31.7307049806423));
#28806=CARTESIAN_POINT('Ctrl Pts',(-3.78854133762356,1.0624982366453,31.7248517218377));
#28807=CARTESIAN_POINT('Ctrl Pts',(-3.75554733180139,1.17378988627484,31.7189984630332));
#28808=CARTESIAN_POINT('Ctrl Pts',(-3.71773403512612,1.28333263188655,31.7131452042287));
#28809=CARTESIAN_POINT('Ctrl Pts',(-3.67987771845016,1.3930000037384,31.7072852862006));
#28810=CARTESIAN_POINT('Ctrl Pts',(-3.63719130220763,1.50091410912668,31.7014253681725));
#28811=CARTESIAN_POINT('Ctrl Pts',(-3.58987799037896,1.60663157388142,31.6955654501443));
#28812=CARTESIAN_POINT('Ctrl Pts',(-3.54253282114334,1.7124202212308,31.6897015864657));
#28813=CARTESIAN_POINT('Ctrl Pts',(-3.49055473786379,1.81600891424349,31.6838377227871));
#28814=CARTESIAN_POINT('Ctrl Pts',(-3.43419256562877,1.91697950489307,31.6779738591084));
#28815=CARTESIAN_POINT('Ctrl Pts',(-3.37774724563876,2.01809905143983,31.672101344821));
#28816=CARTESIAN_POINT('Ctrl Pts',(-3.31690514504655,2.11659243672795,31.6662288305336));
#28817=CARTESIAN_POINT('Ctrl Pts',(-3.25195801391227,2.21207099247555,31.6603563162462));
#28818=CARTESIAN_POINT('Ctrl Pts',(-3.23400801926684,2.23845921832157,31.6587332791979));
#28819=CARTESIAN_POINT('Ctrl Pts',(-3.21574469416063,2.26461735592319,31.6571102421496));
#28820=CARTESIAN_POINT('Ctrl Pts',(-3.19717471782691,2.2905376713096,31.6554872051012));
#28821=CARTESIAN_POINT('Ctrl Pts',(-3.12998881890394,2.38431698789608,31.6496150811352));
#28822=CARTESIAN_POINT('Ctrl Pts',(-3.05856069220708,2.47529497941596,31.6437429571692));
#28823=CARTESIAN_POINT('Ctrl Pts',(-2.98315198438263,2.56306325284297,31.6378708332032));
#28824=CARTESIAN_POINT('Ctrl Pts',(-2.90784104544492,2.65071773296107,31.6320063225625));
#28825=CARTESIAN_POINT('Ctrl Pts',(-2.8285600554653,2.73517045995463,31.6261418119217));
#28826=CARTESIAN_POINT('Ctrl Pts',(-2.7456134683507,2.81604255692474,31.620277301281));
#28827=CARTESIAN_POINT('Ctrl Pts',(-2.66275223244944,2.89683143731124,31.6144188251634));
#28828=CARTESIAN_POINT('Ctrl Pts',(-2.57623319605064,2.97404672932177,31.6085603490459));
#28829=CARTESIAN_POINT('Ctrl Pts',(-2.48640010144476,3.04734368516836,31.6027018729283));
#28830=CARTESIAN_POINT('Ctrl Pts',(-2.39302476892212,3.12353083707601,31.596612389337));
#28831=CARTESIAN_POINT('Ctrl Pts',(-2.2960689424696,3.19548394002888,31.5905229057457));
#28832=CARTESIAN_POINT('Ctrl Pts',(-2.19595998586853,3.26285898262004,31.5844334221545));
#28833=CARTESIAN_POINT('Ctrl Pts',(-2.09976036189145,3.32760297739104,31.5785817376341));
#28834=CARTESIAN_POINT('Ctrl Pts',(-2.00064962612047,3.38811950316052,31.5727300531137));
#28835=CARTESIAN_POINT('Ctrl Pts',(-1.89903886540533,3.44414581393994,31.5668783685933));
#28836=CARTESIAN_POINT('Ctrl Pts',(-1.79744360253997,3.5001635794891,31.561027576582));
#28837=CARTESIAN_POINT('Ctrl Pts',(-1.69334943481795,3.55169229219511,31.5551767845707));
#28838=CARTESIAN_POINT('Ctrl Pts',(-1.58719328007681,3.59851448401684,31.5493259925594));
#28839=CARTESIAN_POINT('Ctrl Pts',(-1.48102760434829,3.64534087525122,31.5434746757993));
#28840=CARTESIAN_POINT('Ctrl Pts',(-1.3727999522399,3.68745973961803,31.5376233590392));
#28841=CARTESIAN_POINT('Ctrl Pts',(-1.26296784462179,3.72470149454307,31.5317720422791));
#28842=CARTESIAN_POINT('Ctrl Pts',(-1.15309928387005,3.76195560995812,31.5259187834745));
#28843=CARTESIAN_POINT('Ctrl Pts',(-1.04162560004453,3.79432926455435,31.52006552467));
#28844=CARTESIAN_POINT('Ctrl Pts',(-0.929019424295612,3.82170274999004,
31.5142122658655));
#28845=CARTESIAN_POINT('Ctrl Pts',(-0.816285137058031,3.84910737810459,
31.5083523478374));
#28846=CARTESIAN_POINT('Ctrl Pts',(-0.702416188177486,3.87150038491752,
31.5024924298093));
#28847=CARTESIAN_POINT('Ctrl Pts',(-0.587895452030208,3.8888131785266,31.4966325117812));
#28848=CARTESIAN_POINT('Ctrl Pts',(-0.473297605793603,3.90613762933514,
31.4907686481026));
#28849=CARTESIAN_POINT('Ctrl Pts',(-0.358047508518624,3.91837501220579,
31.4849047844239));
#28850=CARTESIAN_POINT('Ctrl Pts',(-0.242631459511845,3.92550875363374,
31.4790409207453));
#28851=CARTESIAN_POINT('Ctrl Pts',(-0.127045144083723,3.93265301904545,
31.4731684064579));
#28852=CARTESIAN_POINT('Ctrl Pts',(-0.0112928001129308,3.93467860912626,
31.4672958921706));
#28853=CARTESIAN_POINT('Ctrl Pts',(0.104140884172505,3.93162099855057,31.4614233778832));
#28854=CARTESIAN_POINT('Ctrl Pts',(0.136044279731012,3.93077594053943,31.4598003408348));
#28855=CARTESIAN_POINT('Ctrl Pts',(0.167923376824294,3.92954290551545,31.4581773037863));
#28856=CARTESIAN_POINT('Ctrl Pts',(0.199768058657367,3.9279233346312,31.4565542667379));
#28857=CARTESIAN_POINT('Ctrl Pts',(0.31498164516342,3.92206375119576,31.4506821427718));
#28858=CARTESIAN_POINT('Ctrl Pts',(0.430130357789259,3.91112089027485,31.4448100188058));
#28859=CARTESIAN_POINT('Ctrl Pts',(0.544729177393587,3.89509423805074,31.4389378948398));
#28860=CARTESIAN_POINT('Ctrl Pts',(0.65917941735272,3.87908836469949,31.433073384199));
#28861=CARTESIAN_POINT('Ctrl Pts',(0.773080776439822,3.85801186435209,31.4272088735583));
#28862=CARTESIAN_POINT('Ctrl Pts',(0.885949940811049,3.8319161919824,31.4213443629176));
#28863=CARTESIAN_POINT('Ctrl Pts',(0.998702963935036,3.80584737179996,31.4154858868));
#28864=CARTESIAN_POINT('Ctrl Pts',(1.11042550458441,3.7747697449502,31.4096274106824));
#28865=CARTESIAN_POINT('Ctrl Pts',(1.22064173718731,3.73878626688346,31.4037689345648));
#28866=CARTESIAN_POINT('Ctrl Pts',(1.33520394183798,3.70138391261158,31.3976794509735));
#28867=CARTESIAN_POINT('Ctrl Pts',(1.4481381524379,3.65868092227371,31.3915899673823));
#28868=CARTESIAN_POINT('Ctrl Pts',(1.55892397835393,3.610851011841,31.385500483791));
#28869=CARTESIAN_POINT('Ctrl Pts',(1.6653835315949,3.56488889661443,31.3796487992706));
#28870=CARTESIAN_POINT('Ctrl Pts',(1.76985892831247,3.51419294690338,31.3737971147502));
#28871=CARTESIAN_POINT('Ctrl Pts',(1.87190695319767,3.4589670941728,31.3679454302297));
#28872=CARTESIAN_POINT('Ctrl Pts',(1.97393941354089,3.40374966458519,31.3620946382184));
#28873=CARTESIAN_POINT('Ctrl Pts',(2.07354487469399,3.34400390242997,31.3562438462071));
#28874=CARTESIAN_POINT('Ctrl Pts',(2.17030426239046,3.27997994028162,31.3503930541957));
#28875=CARTESIAN_POINT('Ctrl Pts',(2.26707232829195,3.21595023591969,31.3445417374356));
#28876=CARTESIAN_POINT('Ctrl Pts',(2.36099346851151,3.1476417969362,31.3386904206755));
#28877=CARTESIAN_POINT('Ctrl Pts',(2.45167776881482,3.07534796696231,31.3328391039153));
#28878=CARTESIAN_POINT('Ctrl Pts',(2.54239216711855,3.00303014276098,31.3269858451108));
#28879=CARTESIAN_POINT('Ctrl Pts',(2.62986726623403,2.92672455494401,31.3211325863063));
#28880=CARTESIAN_POINT('Ctrl Pts',(2.71374695338587,2.8467642109927,31.3152793275019));
#28881=CARTESIAN_POINT('Ctrl Pts',(2.79772207004357,2.76671289655293,31.3094194094737));
#28882=CARTESIAN_POINT('Ctrl Pts',(2.87809331083021,2.68299881214748,31.3035594914456));
#28883=CARTESIAN_POINT('Ctrl Pts',(2.95454203957614,2.59599120498843,31.2976995734174));
#28884=CARTESIAN_POINT('Ctrl Pts',(3.03104224343875,2.5089250131177,31.2918357097388));
#28885=CARTESIAN_POINT('Ctrl Pts',(3.1036144179988,2.41856120431654,31.2859718460602));
#28886=CARTESIAN_POINT('Ctrl Pts',(3.17198184688789,2.32530001569984,31.2801079823816));
#28887=CARTESIAN_POINT('Ctrl Pts',(3.24045013417226,2.23190124440702,31.2742354680942));
#28888=CARTESIAN_POINT('Ctrl Pts',(3.30470106714808,2.13559690513932,31.2683629538067));
#28889=CARTESIAN_POINT('Ctrl Pts',(3.36450259550393,2.03681400349844,31.2624904395193));
#28890=CARTESIAN_POINT('Ctrl Pts',(3.38103045585764,2.00951252728967,31.260867402471));
#28891=CARTESIAN_POINT('Ctrl Pts',(3.39721872650933,1.9820218543258,31.2592443654227));
#28892=CARTESIAN_POINT('Ctrl Pts',(3.41306315351778,1.95435127602468,31.2576213283744));
#28893=CARTESIAN_POINT('Ctrl Pts',(3.47282941894242,1.84997595678364,31.2514991213061));
#28894=CARTESIAN_POINT('Ctrl Pts',(3.52788579428435,1.74271420706082,31.2453769142378));
#28895=CARTESIAN_POINT('Ctrl Pts',(3.57795569987535,1.63301010705062,31.2392547071696));
#28896=CARTESIAN_POINT('Ctrl Pts',(3.62794038119396,1.52349273501587,31.2331429207449));
#28897=CARTESIAN_POINT('Ctrl Pts',(3.67295534489491,1.41154161984525,31.2270311343203));
#28898=CARTESIAN_POINT('Ctrl Pts',(3.71276900053987,1.29762681408415,31.2209193478957));
#28899=CARTESIAN_POINT('Ctrl Pts',(3.75249823434007,1.18395355605065,31.2148205210518));
#28900=CARTESIAN_POINT('Ctrl Pts',(3.7870480245688,1.06832524865232,31.2087216942079));
#28901=CARTESIAN_POINT('Ctrl Pts',(3.81623451173568,0.951232438175632,31.202622867364));
#28902=CARTESIAN_POINT('Ctrl Pts',(3.84538425142669,0.834287054321492,31.1965317192959));
#28903=CARTESIAN_POINT('Ctrl Pts',(3.86918404490673,0.715881189403285,31.1904405712279));
#28904=CARTESIAN_POINT('Ctrl Pts',(3.88749925303357,0.596522051280121,31.1843494231598));
#28905=CARTESIAN_POINT('Ctrl Pts',(3.90578672503263,0.47734366787643,31.1782674993856));
#28906=CARTESIAN_POINT('Ctrl Pts',(3.91860611103049,0.357215246689481,31.1721855756113));
#28907=CARTESIAN_POINT('Ctrl Pts',(3.92587358486372,0.236655014037924,31.1661036518371));
#28908=CARTESIAN_POINT('Ctrl Pts',(3.93062945839558,0.157759756535824,31.1621236085697));
#28909=CARTESIAN_POINT('Ctrl Pts',(3.93300877692551,0.0786798389978914,
31.1581435653024));
#28910=CARTESIAN_POINT('Ctrl Pts',(3.9329999756645,-0.000437519150454106,
31.154163522035));
#28911=CARTESIAN_POINT('',(3.93299844479652,-0.00349760319678261,29.904163522035));
#28912=CARTESIAN_POINT('Ctrl Pts',(3.92653051012146,-0.000442985236362668,
31.1541632103437));
#28913=CARTESIAN_POINT('Ctrl Pts',(3.92715270988084,-0.632035046566581,
31.1223382702328));
#28914=CARTESIAN_POINT('Ctrl Pts',(3.48464175740125,-2.57879812069702,31.024202350667));
#28915=CARTESIAN_POINT('Ctrl Pts',(0.42250134717443,-4.63312290995347,30.8597554516478));
#28916=CARTESIAN_POINT('Ctrl Pts',(-3.67020569990779,-2.85900776625179,
30.6608225132839));
#28917=CARTESIAN_POINT('Ctrl Pts',(-4.38887601457751,1.54340617330452,30.4618895749206));
#28918=CARTESIAN_POINT('Ctrl Pts',(-1.07283271971807,4.52695982339219,30.2629566365571));
#28919=CARTESIAN_POINT('Ctrl Pts',(2.94779101406056,3.42599118849705,30.0770481958641));
#28920=CARTESIAN_POINT('Ctrl Pts',(3.92473384533602,1.0486395575314,29.9574507346254));
#28921=CARTESIAN_POINT('Ctrl Pts',(3.93446900659642,-0.00348448155303831,
29.9041642528413));
#28922=CARTESIAN_POINT('',(3.93485131529986,0.00199336934087166,28.6541629095192));
#28923=CARTESIAN_POINT('Ctrl Pts',(3.93299844479652,-0.00349760319678261,
29.904163522035));
#28924=CARTESIAN_POINT('Ctrl Pts',(3.93284906009518,-0.171478293121667,
29.8956526164004));
#28925=CARTESIAN_POINT('Ctrl Pts',(3.92193455469223,-0.338999641682638,
29.8871417107657));
#28926=CARTESIAN_POINT('Ctrl Pts',(3.90045004247335,-0.504953924798754,
29.8786308051311));
#28927=CARTESIAN_POINT('Ctrl Pts',(3.88905676733525,-0.592959777043594,
29.8741174566975));
#28928=CARTESIAN_POINT('Ctrl Pts',(3.8746917325344,-0.680525562943774,29.8696041082638));
#28929=CARTESIAN_POINT('Ctrl Pts',(3.85738892320343,-0.76748921500402,29.8650907598302));
#28930=CARTESIAN_POINT('Ctrl Pts',(3.83487698049658,-0.880633890837322,
29.8592186358641));
#28931=CARTESIAN_POINT('Ctrl Pts',(3.80734494774706,-0.992976934224231,
29.853346511898));
#28932=CARTESIAN_POINT('Ctrl Pts',(3.77486267961663,-1.10403838250195,29.8474743879319));
#28933=CARTESIAN_POINT('Ctrl Pts',(3.74242252539182,-1.21495583740668,29.8416098772911));
#28934=CARTESIAN_POINT('Ctrl Pts',(3.7050450139926,-1.32459460842593,29.8357453666504));
#28935=CARTESIAN_POINT('Ctrl Pts',(3.66285117170211,-1.43248395940774,29.8298808560096));
#28936=CARTESIAN_POINT('Ctrl Pts',(3.62070074645552,-1.54026229332085,29.8240223798919));
#28937=CARTESIAN_POINT('Ctrl Pts',(3.57374399761799,-1.64629440505415,29.8181639037743));
#28938=CARTESIAN_POINT('Ctrl Pts',(3.52215182078143,-1.75012443882314,29.8123054276566));
#28939=CARTESIAN_POINT('Ctrl Pts',(3.46852529607209,-1.85804862835917,29.8062159440653));
#28940=CARTESIAN_POINT('Ctrl Pts',(3.4098903882644,-1.96359306873341,29.8001264604741));
#28941=CARTESIAN_POINT('Ctrl Pts',(3.34649447006966,-2.06626807597494,29.7940369768829));
#28942=CARTESIAN_POINT('Ctrl Pts',(3.28557421179136,-2.1649335443205,29.7881852923624));
#28943=CARTESIAN_POINT('Ctrl Pts',(3.22025804525689,-2.26094909632023,29.782333607842));
#28944=CARTESIAN_POINT('Ctrl Pts',(3.15081204298773,-2.35390579033306,29.7764819233215));
#28945=CARTESIAN_POINT('Ctrl Pts',(3.0813766327435,-2.4468483064294,29.7706311313102));
#28946=CARTESIAN_POINT('Ctrl Pts',(3.00781288654246,-2.53673256106863,29.7647803392988));
#28947=CARTESIAN_POINT('Ctrl Pts',(2.93042908704734,-2.62318020078433,29.7589295472875));
#28948=CARTESIAN_POINT('Ctrl Pts',(2.85303834711451,-2.70963559386006,29.7530782305273));
#28949=CARTESIAN_POINT('Ctrl Pts',(2.7718271485496,-2.79265345124264,29.7472269137671));
#28950=CARTESIAN_POINT('Ctrl Pts',(2.68714229761701,-2.87189053975906,29.741375597007));
#28951=CARTESIAN_POINT('Ctrl Pts',(2.60242933989278,-2.95115392696188,29.7355223382024));
#28952=CARTESIAN_POINT('Ctrl Pts',(2.51424073904886,-3.02663376783994,29.7296690793978));
#28953=CARTESIAN_POINT('Ctrl Pts',(2.42295764192634,-3.09802602723585,29.7238158205932));
#28954=CARTESIAN_POINT('Ctrl Pts',(2.33157069247588,-3.16949950925204,29.7179559025651));
#28955=CARTESIAN_POINT('Ctrl Pts',(2.23708254557593,-3.23687587283017,29.7120959845369));
#28956=CARTESIAN_POINT('Ctrl Pts',(2.13990476758515,-3.29989342034957,29.7062360665088));
#28957=CARTESIAN_POINT('Ctrl Pts',(2.0426615570153,-3.36295339938721,29.7003722028301));
#28958=CARTESIAN_POINT('Ctrl Pts',(1.94272546489425,-3.421648509518,29.6945083391514));
#28959=CARTESIAN_POINT('Ctrl Pts',(1.84053263822175,-3.47576302524215,29.6886444754728));
#28960=CARTESIAN_POINT('Ctrl Pts',(1.73818905255997,-3.5299573728876,29.6827719611853));
#28961=CARTESIAN_POINT('Ctrl Pts',(1.63358245997928,-3.57955746299714,29.6768994468979));
#28962=CARTESIAN_POINT('Ctrl Pts',(1.52716901295618,-3.6243956469826,29.6710269326105));
#28963=CARTESIAN_POINT('Ctrl Pts',(1.49775861760391,-3.6367879597474,29.6694038955626));
#28964=CARTESIAN_POINT('Ctrl Pts',(1.46821029221,-3.64881682804423,29.6677808585148));
#28965=CARTESIAN_POINT('Ctrl Pts',(1.43853384702914,-3.66047939086557,29.666157821467));
#28966=CARTESIAN_POINT('Ctrl Pts',(1.33116490852846,-3.70267437017299,29.660285697501));
#28967=CARTESIAN_POINT('Ctrl Pts',(1.22175790280795,-3.74021207553294,29.654413573535));
#28968=CARTESIAN_POINT('Ctrl Pts',(1.11075443632941,-3.77289193884141,29.648541449569));
#28969=CARTESIAN_POINT('Ctrl Pts',(0.999894888049307,-3.8055294320582,29.6426769389283));
#28970=CARTESIAN_POINT('Ctrl Pts',(0.887443388095505,-3.83332149255809,
29.6368124282876));
#28971=CARTESIAN_POINT('Ctrl Pts',(0.77386142982746,-3.85611559570319,29.6309479176469));
#28972=CARTESIAN_POINT('Ctrl Pts',(0.660396346264503,-3.87888624394293,
29.6250894415293));
#28973=CARTESIAN_POINT('Ctrl Pts',(0.545803520998237,-3.89666908334398,
29.6192309654117));
#28974=CARTESIAN_POINT('Ctrl Pts',(0.430558873192705,-3.90936159196294,
29.6133724892941));
#28975=CARTESIAN_POINT('Ctrl Pts',(0.310769976266677,-3.92255458300974,
29.6072830057028));
#28976=CARTESIAN_POINT('Ctrl Pts',(0.190277231333197,-3.93024741903001,
29.6011935221116));
#28977=CARTESIAN_POINT('Ctrl Pts',(0.0696263462450617,-3.93238365014256,
29.5951040385203));
#28978=CARTESIAN_POINT('Ctrl Pts',(-0.0463130279333092,-3.93443645976852,
29.5892523539999));
#28979=CARTESIAN_POINT('Ctrl Pts',(-0.162397970760541,-3.93135849208458,
29.5834006694795));
#28980=CARTESIAN_POINT('Ctrl Pts',(-0.278140609956272,-3.9231526609467,
29.5775489849591));
#28981=CARTESIAN_POINT('Ctrl Pts',(-0.393865595883609,-3.91494808137644,
29.5716981929478));
#28982=CARTESIAN_POINT('Ctrl Pts',(-0.509247969722975,-3.90161722266158,
29.5658474009365));
#28983=CARTESIAN_POINT('Ctrl Pts',(-0.623802789209033,-3.88321504428676,
29.5599966089252));
#28984=CARTESIAN_POINT('Ctrl Pts',(-0.738367882946152,-3.86481121544799,
29.554145292165));
#28985=CARTESIAN_POINT('Ctrl Pts',(-0.85210486657937,-3.84133522834515,
29.5482939754049));
#28986=CARTESIAN_POINT('Ctrl Pts',(-0.964537533385841,-3.81289343500313,
29.5424426586448));
#28987=CARTESIAN_POINT('Ctrl Pts',(-1.07700751644763,-3.78444220186703,
29.5365893998403));
#28988=CARTESIAN_POINT('Ctrl Pts',(-1.18817192131121,-3.75102198659634,
29.5307361410357));
#28989=CARTESIAN_POINT('Ctrl Pts',(-1.29756896825033,-3.712789217372,29.5248828822312));
#28990=CARTESIAN_POINT('Ctrl Pts',(-1.40709047566875,-3.67451295091518,
29.5190229642031));
#28991=CARTESIAN_POINT('Ctrl Pts',(-1.51484022133172,-3.63141333858677,
29.513163046175));
#28992=CARTESIAN_POINT('Ctrl Pts',(-1.62037561296927,-3.5836952818138,29.5073031281469));
#28993=CARTESIAN_POINT('Ctrl Pts',(-1.72598206460632,-3.53594509510755,
29.5014392644682));
#28994=CARTESIAN_POINT('Ctrl Pts',(-1.82937082547736,-3.4835704582407,29.4955754007896));
#28995=CARTESIAN_POINT('Ctrl Pts',(-1.93012470408345,-3.42682179675086,
29.489711537111));
#28996=CARTESIAN_POINT('Ctrl Pts',(-2.03102721888446,-3.36998941734139,
29.4838390228236));
#28997=CARTESIAN_POINT('Ctrl Pts',(-2.12928674395181,-3.30877035263574,
29.4779665085362));
#28998=CARTESIAN_POINT('Ctrl Pts',(-2.22451573179629,-3.2434578398664,29.4720939942488));
#28999=CARTESIAN_POINT('Ctrl Pts',(-2.25083498242682,-3.22540686156877,
29.4704709572004));
#29000=CARTESIAN_POINT('Ctrl Pts',(-2.27692294587023,-3.20704343677172,
29.4688479201519));
#29001=CARTESIAN_POINT('Ctrl Pts',(-2.30277191380627,-3.18837427429481,
29.4672248831034));
#29002=CARTESIAN_POINT('Ctrl Pts',(-2.3962930963675,-3.1208295213829,29.4613527591374));
#29003=CARTESIAN_POINT('Ctrl Pts',(-2.48699671889459,-3.04905330606792,
29.4554806351713));
#29004=CARTESIAN_POINT('Ctrl Pts',(-2.57447539394731,-2.97330883797157,
29.4496085112053));
#29005=CARTESIAN_POINT('Ctrl Pts',(-2.66184065116091,-2.89766257408203,
29.4437440005646));
#29006=CARTESIAN_POINT('Ctrl Pts',(-2.7459889661596,-2.81805855689906,29.4378794899239));
#29007=CARTESIAN_POINT('Ctrl Pts',(-2.82654263144434,-2.73480268988965,
29.4320149792831));
#29008=CARTESIAN_POINT('Ctrl Pts',(-2.90701340780886,-2.65163249233916,
29.4261565031655));
#29009=CARTESIAN_POINT('Ctrl Pts',(-2.98389660593065,-2.56481821455995,
29.4202980270479));
#29010=CARTESIAN_POINT('Ctrl Pts',(-3.05684879771777,-2.4747049173369,29.4144395509303));
#29011=CARTESIAN_POINT('Ctrl Pts',(-3.13267759106207,-2.38103833343712,
29.4083500673391));
#29012=CARTESIAN_POINT('Ctrl Pts',(-3.20425864665995,-2.28380750608733,
29.4022605837478));
#29013=CARTESIAN_POINT('Ctrl Pts',(-3.27124959321922,-2.18344111412766,
29.3961711001565));
#29014=CARTESIAN_POINT('Ctrl Pts',(-3.3356244912073,-2.08699410784274,29.3903194156361));
#29015=CARTESIAN_POINT('Ctrl Pts',(-3.39576079631841,-1.98765221011616,
29.3844677311157));
#29016=CARTESIAN_POINT('Ctrl Pts',(-3.45139733971157,-1.88582751157997,
29.3786160465953));
#29017=CARTESIAN_POINT('Ctrl Pts',(-3.50702539732247,-1.78401834352369,
29.372765254584));
#29018=CARTESIAN_POINT('Ctrl Pts',(-3.55815485964579,-1.67972749028393,
29.3669144625727));
#29019=CARTESIAN_POINT('Ctrl Pts',(-3.60456993443571,-1.57339269979307,
29.3610636705614));
#29020=CARTESIAN_POINT('Ctrl Pts',(-3.65098917212453,-1.4670483722933,29.3552123538013));
#29021=CARTESIAN_POINT('Ctrl Pts',(-3.69269301634483,-1.35866012203639,
29.3493610370412));
#29022=CARTESIAN_POINT('Ctrl Pts',(-3.72951363891366,-1.24868611634668,
29.343509720281));
#29023=CARTESIAN_POINT('Ctrl Pts',(-3.76634648219906,-1.13867561042808,
29.3376564614765));
#29024=CARTESIAN_POINT('Ctrl Pts',(-3.79829274992259,-1.02707869435946,
29.331803202672));
#29025=CARTESIAN_POINT('Ctrl Pts',(-3.82523454566782,-0.914368454524485,
29.3259499438675));
#29026=CARTESIAN_POINT('Ctrl Pts',(-3.85220699296083,-0.801529984807069,
29.3200900258394));
#29027=CARTESIAN_POINT('Ctrl Pts',(-3.87416350790446,-0.687576065502403,
29.3142301078113));
#29028=CARTESIAN_POINT('Ctrl Pts',(-3.8910373493969,-0.572989830274792,
29.3083701897832));
#29029=CARTESIAN_POINT('Ctrl Pts',(-3.90792255252973,-0.458326440855689,
29.3025063261045));
#29030=CARTESIAN_POINT('Ctrl Pts',(-3.91971822575057,-0.343030298011647,
29.2966424624259));
#29031=CARTESIAN_POINT('Ctrl Pts',(-3.92640965909689,-0.227587760986074,
29.2907785987473));
#29032=CARTESIAN_POINT('Ctrl Pts',(-3.9331109639162,-0.111974918462815,
29.2849060844599));
#29033=CARTESIAN_POINT('Ctrl Pts',(-3.93469299478883,0.00378433744485622,
29.2790335701725));
#29034=CARTESIAN_POINT('Ctrl Pts',(-3.93119308337595,0.119205458000484,
29.2731610558851));
#29035=CARTESIAN_POINT('Ctrl Pts',(-3.93022578289592,0.151105381212052,
29.2715380188368));
#29036=CARTESIAN_POINT('Ctrl Pts',(-3.92887060135923,0.182979519471364,
29.2699149817884));
#29037=CARTESIAN_POINT('Ctrl Pts',(-3.92712901867379,0.214817761579978,
29.26829194474));
#29038=CARTESIAN_POINT('Ctrl Pts',(-3.92082799835126,0.330008049263163,
29.262419820774));
#29039=CARTESIAN_POINT('Ctrl Pts',(-3.9094439864485,0.44511398524188,29.2565476968079));
#29040=CARTESIAN_POINT('Ctrl Pts',(-3.89297832766679,0.559650551966735,
29.2506755728419));
#29041=CARTESIAN_POINT('Ctrl Pts',(-3.87653401693863,0.674038619758618,
29.2448110622012));
#29042=CARTESIAN_POINT('Ctrl Pts',(-3.85502121966352,0.787858380882195,
29.2389465515604));
#29043=CARTESIAN_POINT('Ctrl Pts',(-3.82849324241835,0.900626722209053,
29.2330820409197));
#29044=CARTESIAN_POINT('Ctrl Pts',(-3.80199256219786,1.01327902603453,29.2272235648021));
#29045=CARTESIAN_POINT('Ctrl Pts',(-3.77048706072516,1.12488166201034,29.2213650886845));
#29046=CARTESIAN_POINT('Ctrl Pts',(-3.73408151598168,1.23495920256662,29.2155066125669));
#29047=CARTESIAN_POINT('Ctrl Pts',(-3.69624045238501,1.34937724635927,29.2094171289756));
#29048=CARTESIAN_POINT('Ctrl Pts',(-3.65310502984808,1.46214699686952,29.2033276453843));
#29049=CARTESIAN_POINT('Ctrl Pts',(-3.60485095711975,1.57274873293632,29.1972381617931));
#29050=CARTESIAN_POINT('Ctrl Pts',(-3.55848124346512,1.67903138517994,29.1913864772726));
#29051=CARTESIAN_POINT('Ctrl Pts',(-3.50738533304776,1.78331175617564,29.1855347927522));
#29052=CARTESIAN_POINT('Ctrl Pts',(-3.45176885416513,1.88514741530087,29.1796831082318));
#29053=CARTESIAN_POINT('Ctrl Pts',(-3.3961608580045,1.98696754227442,29.1738323162205));
#29054=CARTESIAN_POINT('Ctrl Pts',(-3.33603386239109,2.08634333603473,29.1679815242092));
#29055=CARTESIAN_POINT('Ctrl Pts',(-3.27163960388811,2.18285668385967,29.1621307321978));
#29056=CARTESIAN_POINT('Ctrl Pts',(-3.20723956995999,2.27937868782305,29.1562794154377));
#29057=CARTESIAN_POINT('Ctrl Pts',(-3.13857174178334,2.3730373915834,29.1504280986775));
#29058=CARTESIAN_POINT('Ctrl Pts',(-3.06593095492429,2.46344400781447,29.1445767819174));
#29059=CARTESIAN_POINT('Ctrl Pts',(-2.99326605868294,2.55388062988341,29.1387235231128));
#29060=CARTESIAN_POINT('Ctrl Pts',(-2.91662584057487,2.64106269607758,29.1328702643083));
#29061=CARTESIAN_POINT('Ctrl Pts',(-2.83634467020339,2.72463537226706,29.1270170055037));
#29062=CARTESIAN_POINT('Ctrl Pts',(-2.75597216434142,2.8083031286769,29.1211570874756));
#29063=CARTESIAN_POINT('Ctrl Pts',(-2.67195072487592,2.8883530005291,29.1152971694475));
#29064=CARTESIAN_POINT('Ctrl Pts',(-2.58465081727061,2.96446776888911,29.1094372514193));
#29065=CARTESIAN_POINT('Ctrl Pts',(-2.49729212813907,3.04063378750099,29.1035733877407));
#29066=CARTESIAN_POINT('Ctrl Pts',(-2.40665089786219,3.11285916971107,29.097709524062));
#29067=CARTESIAN_POINT('Ctrl Pts',(-2.31312842094905,3.18086873482666,29.0918456603834));
#29068=CARTESIAN_POINT('Ctrl Pts',(-2.21946797589712,3.24897863040214,29.085973146096));
#29069=CARTESIAN_POINT('Ctrl Pts',(-2.122918144424,3.31286006896241,29.0801006318086));
#29070=CARTESIAN_POINT('Ctrl Pts',(-2.02390681817594,3.37228263811634,29.0742281175212));
#29071=CARTESIAN_POINT('Ctrl Pts',(-1.99654221030443,3.38870576227026,29.072605080473));
#29072=CARTESIAN_POINT('Ctrl Pts',(-1.96898970831987,3.40478857424379,29.0709820434247));
#29073=CARTESIAN_POINT('Ctrl Pts',(-1.94125861987231,3.42052685573019,29.0693590063765));
#29074=CARTESIAN_POINT('Ctrl Pts',(-1.84092795320357,3.47746772470245,29.0634868824105));
#29075=CARTESIAN_POINT('Ctrl Pts',(-1.73792168060312,3.53008597276691,29.0576147584445));
#29076=CARTESIAN_POINT('Ctrl Pts',(-1.63264864272382,3.57812065327765,29.0517426344785));
#29077=CARTESIAN_POINT('Ctrl Pts',(-1.52751209342835,3.62609305587136,29.0458781238377));
#29078=CARTESIAN_POINT('Ctrl Pts',(-1.42011499590566,3.66949353873066,29.0400136131971));
#29079=CARTESIAN_POINT('Ctrl Pts',(-1.31089266583091,3.70810590715405,29.0341491025563));
#29080=CARTESIAN_POINT('Ctrl Pts',(-1.2017827244472,3.74667854383446,29.0282906264388));
#29081=CARTESIAN_POINT('Ctrl Pts',(-1.09085167365963,3.7804727289979,29.0224321503212));
#29082=CARTESIAN_POINT('Ctrl Pts',(-0.978556174649823,3.80931973100903,
29.0165736742036));
#29083=CARTESIAN_POINT('Ctrl Pts',(-0.861832715363183,3.83930420852128,
29.0104841906123));
#29084=CARTESIAN_POINT('Ctrl Pts',(-0.743635404108951,3.86394313950291,
29.004394707021));
#29085=CARTESIAN_POINT('Ctrl Pts',(-0.624496499827956,3.88310354249055,
28.9983052234298));
#29086=CARTESIAN_POINT('Ctrl Pts',(-0.510010062430147,3.90151571683778,
28.9924535389094));
#29087=CARTESIAN_POINT('Ctrl Pts',(-0.394654638485822,3.91486914347265,
28.986601854389));
#29088=CARTESIAN_POINT('Ctrl Pts',(-0.278913618405177,3.92309778025837,
28.9807501698686));
#29089=CARTESIAN_POINT('Ctrl Pts',(-0.16319025134603,3.9313251619981,28.9748993778573));
#29090=CARTESIAN_POINT('Ctrl Pts',(-0.0470818173448765,3.93442927872797,
28.969048585846));
#29091=CARTESIAN_POINT('Ctrl Pts',(0.0689238407894238,3.93239602585635,
28.9631977938347));
#29092=CARTESIAN_POINT('Ctrl Pts',(0.184939903298399,3.93036259062531,28.9573464770746));
#29093=CARTESIAN_POINT('Ctrl Pts',(0.300852758242594,3.92319087708354,28.9514951603145));
#29094=CARTESIAN_POINT('Ctrl Pts',(0.416175949978906,3.91091889185383,28.9456438435544));
#29095=CARTESIAN_POINT('Ctrl Pts',(0.531537417332094,3.89864283356822,28.9397905847499));
#29096=CARTESIAN_POINT('Ctrl Pts',(0.646308421449583,3.88126318134766,28.9339373259454));
#29097=CARTESIAN_POINT('Ctrl Pts',(0.760009714199924,3.85886955393957,28.9280840671409));
#29098=CARTESIAN_POINT('Ctrl Pts',(0.873840364348574,3.83645044941235,28.9222241491128));
#29099=CARTESIAN_POINT('Ctrl Pts',(0.986598468157101,3.80900606385187,28.9163642310847));
#29100=CARTESIAN_POINT('Ctrl Pts',(1.0978169241759,3.77667671385743,28.9105043130566));
#29101=CARTESIAN_POINT('Ctrl Pts',(1.20911026676409,3.74432559558641,28.904640449378));
#29102=CARTESIAN_POINT('Ctrl Pts',(1.31886150678038,3.70708309598909,28.8987765856994));
#29103=CARTESIAN_POINT('Ctrl Pts',(1.42662225710485,3.66513818778134,28.8929127220207));
#29104=CARTESIAN_POINT('Ctrl Pts',(1.5345419804447,3.62313140074927,28.8870402077334));
#29105=CARTESIAN_POINT('Ctrl Pts',(1.64046497664927,3.57640852599884,28.881167693446));
#29106=CARTESIAN_POINT('Ctrl Pts',(1.7439661568167,3.52520510663961,28.8752951791586));
#29107=CARTESIAN_POINT('Ctrl Pts',(1.77257166405825,3.51105357927631,28.8736721421101));
#29108=CARTESIAN_POINT('Ctrl Pts',(1.80099234655962,3.49656006303404,28.8720491050617));
#29109=CARTESIAN_POINT('Ctrl Pts',(1.8292196254935,3.48173011040623,28.8704260680132));
#29110=CARTESIAN_POINT('Ctrl Pts',(1.93134550196597,3.42807556177944,28.8645539440471));
#29111=CARTESIAN_POINT('Ctrl Pts',(2.03127990206342,3.36983392803109,28.8586818200811));
#29112=CARTESIAN_POINT('Ctrl Pts',(2.12858233824638,3.30720822285286,28.8528096961151));
#29113=CARTESIAN_POINT('Ctrl Pts',(2.22575861988876,3.24466371314491,28.8469451854744));
#29114=CARTESIAN_POINT('Ctrl Pts',(2.32030937920909,3.17774665716709,28.8410806748336));
#29115=CARTESIAN_POINT('Ctrl Pts',(2.41181747910689,3.10670652741363,28.8352161641929));
#29116=CARTESIAN_POINT('Ctrl Pts',(2.50323141808017,3.03573949724703,28.8293576880753));
#29117=CARTESIAN_POINT('Ctrl Pts',(2.59160860048117,2.96065808403047,28.8234992119577));
#29118=CARTESIAN_POINT('Ctrl Pts',(2.67656029262184,2.88175536782012,28.8176407358401));
#29119=CARTESIAN_POINT('Ctrl Pts',(2.76486174251365,2.79974141299225,28.8115512522488));
#29120=CARTESIAN_POINT('Ctrl Pts',(2.84946161860741,2.71359884353586,28.8054617686576));
#29121=CARTESIAN_POINT('Ctrl Pts',(2.92996041982669,2.62370366814718,28.7993722850663));
#29122=CARTESIAN_POINT('Ctrl Pts',(3.00731568024349,2.53731896928115,28.7935206005459));
#29123=CARTESIAN_POINT('Ctrl Pts',(3.08088385372034,2.44746958593525,28.7876689160255));
#29124=CARTESIAN_POINT('Ctrl Pts',(3.15034817072902,2.35452657729411,28.7818172315051));
#29125=CARTESIAN_POINT('Ctrl Pts',(3.2198018929194,2.26159774448211,28.7759664394938));
#29126=CARTESIAN_POINT('Ctrl Pts',(3.28515275575619,2.16557655560454,28.7701156474824));
#29127=CARTESIAN_POINT('Ctrl Pts',(3.34612528628986,2.06686588061528,28.7642648554711));
#29128=CARTESIAN_POINT('Ctrl Pts',(3.407103285359,1.96814635241258,28.758413538711));
#29129=CARTESIAN_POINT('Ctrl Pts',(3.46370195423207,1.8667372103279,28.7525622219508));
#29130=CARTESIAN_POINT('Ctrl Pts',(3.51569041806618,1.76306831527246,28.7467109051907));
#29131=CARTESIAN_POINT('Ctrl Pts',(3.5676961368035,1.65936501264622,28.7408576463862));
#29132=CARTESIAN_POINT('Ctrl Pts',(3.61508842273111,1.55340083505744,28.7350043875816));
#29133=CARTESIAN_POINT('Ctrl Pts',(3.6576837241685,1.4456274672103,28.7291511287771));
#29134=CARTESIAN_POINT('Ctrl Pts',(3.70032748606968,1.33773148613555,28.723291210749));
#29135=CARTESIAN_POINT('Ctrl Pts',(3.73816321839806,1.22802259117911,28.7174312927208));
#29136=CARTESIAN_POINT('Ctrl Pts',(3.77105659219758,1.11696964078851,28.7115713746927));
#29137=CARTESIAN_POINT('Ctrl Pts',(3.80397211404706,1.00584191526814,28.7057075110141));
#29138=CARTESIAN_POINT('Ctrl Pts',(3.83193855149017,0.893368732516753,28.6998436473354));
#29139=CARTESIAN_POINT('Ctrl Pts',(3.85487262910747,0.7800294951847,28.6939797836568));
#29140=CARTESIAN_POINT('Ctrl Pts',(3.87784054000324,0.666523055227682,28.6881072693694));
#29141=CARTESIAN_POINT('Ctrl Pts',(3.89576121051136,0.552148417660778,28.682234755082));
#29142=CARTESIAN_POINT('Ctrl Pts',(3.90860314062828,0.437390545246166,28.6763622407945));
#29143=CARTESIAN_POINT('Ctrl Pts',(3.91215237479467,0.405673929602851,28.6747392037462));
#29144=CARTESIAN_POINT('Ctrl Pts',(3.91531397558892,0.373928040308329,28.6731161666979));
#29145=CARTESIAN_POINT('Ctrl Pts',(3.91808797956127,0.342163096223857,28.6714931296496));
#29146=CARTESIAN_POINT('Ctrl Pts',(3.92796091097148,0.229108782920413,28.6657165937781));
#29147=CARTESIAN_POINT('Ctrl Pts',(3.93294158348204,0.115621047768071,28.6599400579065));
#29148=CARTESIAN_POINT('Ctrl Pts',(3.93299948919698,0.00200448904475932,
28.654163522035));
#29149=CARTESIAN_POINT('',(3.9313993161518,0.00256731592070132,27.4041640341379));
#29150=CARTESIAN_POINT('Ctrl Pts',(3.93827238435518,0.00197282676680643,
28.6541617779557));
#29151=CARTESIAN_POINT('Ctrl Pts',(3.93085187581135,-1.19024594622667,28.5936279157326));
#29152=CARTESIAN_POINT('Ctrl Pts',(2.71699568782789,-3.70151452867356,28.466783074055));
#29153=CARTESIAN_POINT('Ctrl Pts',(-1.56021230829742,-4.38292970969908,
28.2736272529227));
#29154=CARTESIAN_POINT('Ctrl Pts',(-4.5310375107926,-1.05547826263657,28.0746943145594));
#29155=CARTESIAN_POINT('Ctrl Pts',(-3.33645939605003,3.24227913444184,27.8757613761959));
#29156=CARTESIAN_POINT('Ctrl Pts',(0.925340961511961,4.55939462999849,27.6768284378326));
#29157=CARTESIAN_POINT('Ctrl Pts',(3.62084980531289,2.28804957005642,27.5196296619495));
#29158=CARTESIAN_POINT('Ctrl Pts',(3.93111323275754,0.489805113098635,27.4287418655209));
#29159=CARTESIAN_POINT('Ctrl Pts',(3.92823021849111,0.00258536452941557,
27.4041650485469));
#29160=CARTESIAN_POINT('',(3.93299891753245,-0.00291799392896185,26.1541635219892));
#29161=CARTESIAN_POINT('Ctrl Pts',(3.93299916801287,0.00255820446269878,
27.404163522035));
#29162=CARTESIAN_POINT('Ctrl Pts',(3.93307519995185,-0.114333762974888,
27.3982742678373));
#29163=CARTESIAN_POINT('Ctrl Pts',(3.9279357123882,-0.231251489364913,27.3923850136396));
#29164=CARTESIAN_POINT('Ctrl Pts',(3.91760045126501,-0.347700595697167,
27.3864957594419));
#29165=CARTESIAN_POINT('Ctrl Pts',(3.90726448546451,-0.46415764174605,27.3806061037039));
#29166=CARTESIAN_POINT('Ctrl Pts',(3.89173207666385,-0.580145599958414,
27.3747164479659));
#29167=CARTESIAN_POINT('Ctrl Pts',(3.87107488587756,-0.695174962098055,
27.3688267922279));
#29168=CARTESIAN_POINT('Ctrl Pts',(3.85041152868984,-0.810238661782951,
27.362935378362));
#29169=CARTESIAN_POINT('Ctrl Pts',(3.82462041725161,-0.924342796774363,
27.3570439644962));
#29170=CARTESIAN_POINT('Ctrl Pts',(3.79382426704607,-1.03700840438847,27.3511525506304));
#29171=CARTESIAN_POINT('Ctrl Pts',(3.76237774431294,-1.15205335537857,27.34513671817));
#29172=CARTESIAN_POINT('Ctrl Pts',(3.72571251901386,-1.26559790615674,27.3391208857096));
#29173=CARTESIAN_POINT('Ctrl Pts',(3.68401224682527,-1.37715023335924,27.3331050532492));
#29174=CARTESIAN_POINT('Ctrl Pts',(3.64309724419288,-1.48660188730765,27.3272025066222));
#29175=CARTESIAN_POINT('Ctrl Pts',(3.59733538762402,-1.59413534420948,27.3212999599951));
#29176=CARTESIAN_POINT('Ctrl Pts',(3.54694774865305,-1.69930887961109,27.3153974133681));
#29177=CARTESIAN_POINT('Ctrl Pts',(3.49510949708227,-1.80751026189607,27.309324937991));
#29178=CARTESIAN_POINT('Ctrl Pts',(3.4383753150512,-1.91321337510273,27.3032524626139));
#29179=CARTESIAN_POINT('Ctrl Pts',(3.37703446391673,-2.01596806262367,27.2971799872368));
#29180=CARTESIAN_POINT('Ctrl Pts',(3.31569361278226,-2.11872275014462,27.2911075118597));
#29181=CARTESIAN_POINT('Ctrl Pts',(3.24974640496889,-2.21852866757598,27.2850350364827));
#29182=CARTESIAN_POINT('Ctrl Pts',(3.17952701572385,-2.31497234460419,27.2789625611056));
#29183=CARTESIAN_POINT('Ctrl Pts',(3.11162440058551,-2.40823401996453,27.2730904371395));
#29184=CARTESIAN_POINT('Ctrl Pts',(3.03950115054566,-2.49866194169357,27.2672183131735));
#29185=CARTESIAN_POINT('Ctrl Pts',(2.9634220343367,-2.58584973391876,27.2613461892074));
#29186=CARTESIAN_POINT('Ctrl Pts',(2.88744155621256,-2.6729244854401,27.2554816785667));
#29187=CARTESIAN_POINT('Ctrl Pts',(2.8075156806553,-2.75676715289067,27.249617167926));
#29188=CARTESIAN_POINT('Ctrl Pts',(2.72395175620044,-2.83700120371714,27.2437526572853));
#29189=CARTESIAN_POINT('Ctrl Pts',(2.64047381819258,-2.91715269450347,27.2378941811677));
#29190=CARTESIAN_POINT('Ctrl Pts',(2.55336557373104,-2.99370266985687,27.23203570505));
#29191=CARTESIAN_POINT('Ctrl Pts',(2.46297339702857,-3.06630902642404,27.2261772289324));
#29192=CARTESIAN_POINT('Ctrl Pts',(2.36901693706222,-3.14177834780746,27.2200877453412));
#29193=CARTESIAN_POINT('Ctrl Pts',(2.27151253645968,-3.21298630502254,27.2139982617499));
#29194=CARTESIAN_POINT('Ctrl Pts',(2.17089018282556,-3.27959217191888,27.2079087781587));
#29195=CARTESIAN_POINT('Ctrl Pts',(2.07419721036827,-3.34359702790466,27.2020570936382));
#29196=CARTESIAN_POINT('Ctrl Pts',(1.9746256093274,-3.40335222937345,27.1962054091178));
#29197=CARTESIAN_POINT('Ctrl Pts',(1.87258846806653,-3.45859818846657,27.1903537245974));
#29198=CARTESIAN_POINT('Ctrl Pts',(1.77056688968782,-3.51383572134998,27.1845029325861));
#29199=CARTESIAN_POINT('Ctrl Pts',(1.66608088223749,-3.56456518255443,27.1786521405748));
#29200=CARTESIAN_POINT('Ctrl Pts',(1.55956901731533,-3.61057245879793,27.1728013485634));
#29201=CARTESIAN_POINT('Ctrl Pts',(1.45304759950266,-3.6565838613655,27.1669500318033));
#29202=CARTESIAN_POINT('Ctrl Pts',(1.34450034256658,-3.69787207309991,27.1610987150432));
#29203=CARTESIAN_POINT('Ctrl Pts',(1.23438605355836,-3.73427102267372,27.155247398283));
#29204=CARTESIAN_POINT('Ctrl Pts',(1.12423521776118,-3.77068205301144,27.1493941394785));
#29205=CARTESIAN_POINT('Ctrl Pts',(1.0125167080311,-3.80220046479399,27.1435408806739));
#29206=CARTESIAN_POINT('Ctrl Pts',(0.899704059038655,-3.82871017526129,
27.1376876218694));
#29207=CARTESIAN_POINT('Ctrl Pts',(0.786763063653723,-3.85525004569501,
27.1318277038413));
#29208=CARTESIAN_POINT('Ctrl Pts',(0.67272584711545,-3.87676974638077,27.1259677858131));
#29209=CARTESIAN_POINT('Ctrl Pts',(0.558075795282372,-3.89320438799711,
27.120107867785));
#29210=CARTESIAN_POINT('Ctrl Pts',(0.443348546288052,-3.90965009552802,
27.1142440041064));
#29211=CARTESIAN_POINT('Ctrl Pts',(0.328008050772991,-3.9210038859026,27.1083801404277));
#29212=CARTESIAN_POINT('Ctrl Pts',(0.212540720776185,-3.9272529129166,27.1025162767491));
#29213=CARTESIAN_POINT('Ctrl Pts',(0.0969030487063048,-3.93351115874788,
27.0966437624617));
#29214=CARTESIAN_POINT('Ctrl Pts',(-0.0188614194399131,-3.93464960718321,
27.0907712481743));
#29215=CARTESIAN_POINT('Ctrl Pts',(-0.134268281532253,-3.9307074463224,
27.0848987338869));
#29216=CARTESIAN_POINT('Ctrl Pts',(-0.166164264007384,-3.92961791757644,
27.0832756968387));
#29217=CARTESIAN_POINT('Ctrl Pts',(-0.198032975421836,-3.92814060942531,
27.0816526597904));
#29218=CARTESIAN_POINT('Ctrl Pts',(-0.229864310322165,-3.92627704051053,
27.0800296227422));
#29219=CARTESIAN_POINT('Ctrl Pts',(-0.345029607838136,-3.91953467581914,
27.0741574987762));
#29220=CARTESIAN_POINT('Ctrl Pts',(-0.460091077063926,-3.90770968008658,
27.0682853748102));
#29221=CARTESIAN_POINT('Ctrl Pts',(-0.574563709163602,-3.89080525651338,
27.0624132508441));
#29222=CARTESIAN_POINT('Ctrl Pts',(-0.688887925223019,-3.87392274986097,
27.0565487402034));
#29223=CARTESIAN_POINT('Ctrl Pts',(-0.802624417162336,-3.85197397153163,
27.0506842295627));
#29224=CARTESIAN_POINT('Ctrl Pts',(-0.915290279662149,-3.82501407892258,
27.044819718922));
#29225=CARTESIAN_POINT('Ctrl Pts',(-1.02784021010985,-3.79808192777493,
27.0389612428044));
#29226=CARTESIAN_POINT('Ctrl Pts',(-1.1393213027452,-3.76614901427624,27.0331027666868));
#29227=CARTESIAN_POINT('Ctrl Pts',(-1.24925853498102,-3.72932193740056,
27.0272442905692));
#29228=CARTESIAN_POINT('Ctrl Pts',(-1.36353073791085,-3.69104272010116,
27.0211548069779));
#29229=CARTESIAN_POINT('Ctrl Pts',(-1.47613437252862,-3.64747549872449,
27.0150653233866));
#29230=CARTESIAN_POINT('Ctrl Pts',(-1.58655039477642,-3.59879797221722,
27.0089758397954));
#29231=CARTESIAN_POINT('Ctrl Pts',(-1.69265458546978,-3.55202134098325,
27.003124155275));
#29232=CARTESIAN_POINT('Ctrl Pts',(-1.79673839959033,-3.50052622010324,
26.9972724707546));
#29233=CARTESIAN_POINT('Ctrl Pts',(-1.89836019769812,-3.44451993168795,
26.9914207862342));
#29234=CARTESIAN_POINT('Ctrl Pts',(-1.99996649627277,-3.38852218544903,
26.9855699942228));
#29235=CARTESIAN_POINT('Ctrl Pts',(-2.09911116350132,-3.32801483922482,
26.9797192022115));
#29236=CARTESIAN_POINT('Ctrl Pts',(-2.19537705434519,-3.26325122987101,
26.9738684102002));
#29237=CARTESIAN_POINT('Ctrl Pts',(-2.29165157913323,-3.19848181196566,
26.9680170934401));
#29238=CARTESIAN_POINT('Ctrl Pts',(-2.38504647123913,-3.12945560284909,
26.9621657766799));
#29239=CARTESIAN_POINT('Ctrl Pts',(-2.47517407595333,-3.05646892569327,
26.9563144599198));
#29240=CARTESIAN_POINT('Ctrl Pts',(-2.5653315939017,-2.98345802435473,26.9504612011153));
#29241=CARTESIAN_POINT('Ctrl Pts',(-2.65221934707568,-2.90648430126828,
26.9446079423108));
#29242=CARTESIAN_POINT('Ctrl Pts',(-2.73548378520081,-2.8258834832497,26.9387546835063));
#29243=CARTESIAN_POINT('Ctrl Pts',(-2.81884295286556,-2.74519096607892,
26.9328947654781));
#29244=CARTESIAN_POINT('Ctrl Pts',(-2.89857028040766,-2.6608634052442,26.92703484745));
#29245=CARTESIAN_POINT('Ctrl Pts',(-2.97434997078541,-2.57327247902137,
26.9211749294219));
#29246=CARTESIAN_POINT('Ctrl Pts',(-3.05018068579772,-2.48562257532082,
26.9153110657433));
#29247=CARTESIAN_POINT('Ctrl Pts',(-3.12205821516957,-2.39470525445772,
26.9094472020646));
#29248=CARTESIAN_POINT('Ctrl Pts',(-3.18970891792442,-2.30092286244311,
26.903583338386));
#29249=CARTESIAN_POINT('Ctrl Pts',(-3.25745942173073,-2.20700211885269,
26.8977108240986));
#29250=CARTESIAN_POINT('Ctrl Pts',(-3.3209704279018,-2.11020821281976,26.8918383098112));
#29251=CARTESIAN_POINT('Ctrl Pts',(-3.38001316534995,-2.01096991575235,
26.8859657955238));
#29252=CARTESIAN_POINT('Ctrl Pts',(-3.39633131216491,-1.98354257801018,
26.8843427584754));
#29253=CARTESIAN_POINT('Ctrl Pts',(-3.41230842931787,-1.95592865155582,
26.8827197214271));
#29254=CARTESIAN_POINT('Ctrl Pts',(-3.42794033419846,-1.92813746013487,
26.8810966843787));
#29255=CARTESIAN_POINT('Ctrl Pts',(-3.48449633418438,-1.82758934180772,
26.8752245604127));
#29256=CARTESIAN_POINT('Ctrl Pts',(-3.53671949250614,-1.72438220077894,
26.8693524364467));
#29257=CARTESIAN_POINT('Ctrl Pts',(-3.58435043104511,-1.61892587460535,
26.8634803124806));
#29258=CARTESIAN_POINT('Ctrl Pts',(-3.63191961512657,-1.51360627465245,
26.8576158018399));
#29259=CARTESIAN_POINT('Ctrl Pts',(-3.67490825098176,-1.40604366192818,
26.8517512911992));
#29260=CARTESIAN_POINT('Ctrl Pts',(-3.71310181355593,-1.2966741773351,26.8458867805585));
#29261=CARTESIAN_POINT('Ctrl Pts',(-3.75125607533416,-1.18741723285364,
26.8400283044409));
#29262=CARTESIAN_POINT('Ctrl Pts',(-3.78462494247863,-1.07635750259455,
26.8341698283233));
#29263=CARTESIAN_POINT('Ctrl Pts',(-3.8130414344448,-0.963952290939315,
26.8283113522057));
#29264=CARTESIAN_POINT('Ctrl Pts',(-3.84257842633071,-0.847114792892496,
26.8222218686144));
#29265=CARTESIAN_POINT('Ctrl Pts',(-3.86676426336712,-0.728823936971667,
26.8161323850232));
#29266=CARTESIAN_POINT('Ctrl Pts',(-3.88546800459745,-0.609612487773617,
26.8100429014319));
#29267=CARTESIAN_POINT('Ctrl Pts',(-3.90344135018425,-0.495056338393972,
26.8041912169115));
#29268=CARTESIAN_POINT('Ctrl Pts',(-3.9163526553811,-0.379650593153888,
26.7983395323911));
#29269=CARTESIAN_POINT('Ctrl Pts',(-3.92413773081026,-0.263878891977561,
26.7924878478707));
#29270=CARTESIAN_POINT('Ctrl Pts',(-3.93192161884617,-0.14812484850251,
26.7866370558594));
#29271=CARTESIAN_POINT('Ctrl Pts',(-3.93458080397028,-0.0320053724387077,
26.7807862638481));
#29272=CARTESIAN_POINT('Ctrl Pts',(-3.93210305102959,0.0839916429399632,
26.7749354718369));
#29273=CARTESIAN_POINT('Ctrl Pts',(-3.92962507586293,0.199999061918414,
26.7690841550767));
#29274=CARTESIAN_POINT('Ctrl Pts',(-3.92200925558307,0.315883585034949,
26.7632328383166));
#29275=CARTESIAN_POINT('Ctrl Pts',(-3.90929546055342,0.431158905853051,
26.7573815215565));
#29276=CARTESIAN_POINT('Ctrl Pts',(-3.89657744583184,0.546472486399326,
26.751528262752));
#29277=CARTESIAN_POINT('Ctrl Pts',(-3.87875813720348,0.661176051894913,
26.7456750039475));
#29278=CARTESIAN_POINT('Ctrl Pts',(-3.85592898915947,0.774790701131377,
26.739821745143));
#29279=CARTESIAN_POINT('Ctrl Pts',(-3.8330738685066,0.88853460919251,26.7339618271149));
#29280=CARTESIAN_POINT('Ctrl Pts',(-3.8051976135385,1.00118672272018,26.7281019090868));
#29281=CARTESIAN_POINT('Ctrl Pts',(-3.77244232968183,1.11228048136462,26.7222419910587));
#29282=CARTESIAN_POINT('Ctrl Pts',(-3.73966499075515,1.22344904261603,26.7163781273801));
#29283=CARTESIAN_POINT('Ctrl Pts',(-3.70200221550103,1.33305676963155,26.7105142637015));
#29284=CARTESIAN_POINT('Ctrl Pts',(-3.65964469339519,1.44065600269614,26.7046504000229));
#29285=CARTESIAN_POINT('Ctrl Pts',(-3.61722468376027,1.54841397049948,26.6987778857355));
#29286=CARTESIAN_POINT('Ctrl Pts',(-3.570096272167,1.65415715453806,26.6929053714481));
#29287=CARTESIAN_POINT('Ctrl Pts',(-3.51849662886788,1.75746137159409,26.6870328571607));
#29288=CARTESIAN_POINT('Ctrl Pts',(-3.50423559370246,1.78601244245387,26.6854098201123));
#29289=CARTESIAN_POINT('Ctrl Pts',(-3.48963328038741,1.81437737948408,26.6837867830638));
#29290=CARTESIAN_POINT('Ctrl Pts',(-3.47469527424812,1.84254762519664,26.6821637460153));
#29291=CARTESIAN_POINT('Ctrl Pts',(-3.42064978961872,1.94446715632202,26.6762916220493));
#29292=CARTESIAN_POINT('Ctrl Pts',(-3.36202565092841,2.04417765018983,26.6704194980833));
#29293=CARTESIAN_POINT('Ctrl Pts',(-3.29902755825575,2.14123940041022,26.6645473741172));
#29294=CARTESIAN_POINT('Ctrl Pts',(-3.23611114386123,2.23817530814402,26.6586828634765));
#29295=CARTESIAN_POINT('Ctrl Pts',(-3.16883227587662,2.33246895793811,26.6528183528358));
#29296=CARTESIAN_POINT('Ctrl Pts',(-3.09744202336682,2.42370417169284,26.6469538421951));
#29297=CARTESIAN_POINT('Ctrl Pts',(-3.02612523071658,2.51484550532033,26.6410953660774));
#29298=CARTESIAN_POINT('Ctrl Pts',(-2.95070572158423,2.60293433901684,26.6352368899598));
#29299=CARTESIAN_POINT('Ctrl Pts',(-2.87147806343919,2.68758306498376,26.6293784138422));
#29300=CARTESIAN_POINT('Ctrl Pts',(-2.78912635378587,2.77556960234411,26.623288930251));
#29301=CARTESIAN_POINT('Ctrl Pts',(-2.70266024364889,2.85983877289536,26.6171994466597));
#29302=CARTESIAN_POINT('Ctrl Pts',(-2.61245726978781,2.93999251929879,26.6111099630684));
#29303=CARTESIAN_POINT('Ctrl Pts',(-2.52577679221898,3.01701619955882,26.605258278548));
#29304=CARTESIAN_POINT('Ctrl Pts',(-2.43564616711349,3.09023954456902,26.5994065940276));
#29305=CARTESIAN_POINT('Ctrl Pts',(-2.34243766474161,3.15934720896578,26.5935549095072));
#29306=CARTESIAN_POINT('Ctrl Pts',(-2.24924337869259,3.2284443329414,26.5877041174958));
#29307=CARTESIAN_POINT('Ctrl Pts',(-2.15297248077676,3.29342677827433,26.5818533254845));
#29308=CARTESIAN_POINT('Ctrl Pts',(-2.05402889355832,3.3540206177702,26.5760025334732));
#29309=CARTESIAN_POINT('Ctrl Pts',(-1.95507643223684,3.41461989183732,26.5701512167131));
#29310=CARTESIAN_POINT('Ctrl Pts',(-1.85345115766715,3.47082956169215,26.5642998999529));
#29311=CARTESIAN_POINT('Ctrl Pts',(-1.74958381227985,3.52242040134455,26.5584485831928));
#29312=CARTESIAN_POINT('Ctrl Pts',(-1.64568199345628,3.57402836392925,26.5525953243882));
#29313=CARTESIAN_POINT('Ctrl Pts',(-1.53953699419985,3.62101426426516,26.5467420655837));
#29314=CARTESIAN_POINT('Ctrl Pts',(-1.43160119923916,3.66319628280236,26.5408888067792));
#29315=CARTESIAN_POINT('Ctrl Pts',(-1.32354260625827,3.70542629161346,26.535028888751));
#29316=CARTESIAN_POINT('Ctrl Pts',(-1.2136895363001,3.74284135935602,26.5291689707229));
#29317=CARTESIAN_POINT('Ctrl Pts',(-1.10251135909697,3.77530895465022,26.5233090526948));
#29318=CARTESIAN_POINT('Ctrl Pts',(-0.991258322445518,3.80779841130546,
26.5174451890161));
#29319=CARTESIAN_POINT('Ctrl Pts',(-0.878678802535022,3.83533366431276,
26.5115813253375));
#29320=CARTESIAN_POINT('Ctrl Pts',(-0.765252517594276,3.85783327585779,
26.5057174616589));
#29321=CARTESIAN_POINT('Ctrl Pts',(-0.651658901612614,3.88036607973933,
26.4998449473715));
#29322=CARTESIAN_POINT('Ctrl Pts',(-0.537216434607124,3.89784835349429,
26.4939724330841));
#29323=CARTESIAN_POINT('Ctrl Pts',(-0.422410196482577,3.91025045564955,
26.4880999187967));
#29324=CARTESIAN_POINT('Ctrl Pts',(-0.390680213593883,3.91367813079682,
26.4864768817484));
#29325=CARTESIAN_POINT('Ctrl Pts',(-0.35892244261754,3.91671806324583,26.4848538447001));
#29326=CARTESIAN_POINT('Ctrl Pts',(-0.327147102199726,3.91937032870362,
26.4832308076518));
#29327=CARTESIAN_POINT('Ctrl Pts',(-0.212184391895869,3.92896618578849,
26.4773586836858));
#29328=CARTESIAN_POINT('Ctrl Pts',(-0.0966063925619334,3.9335157236183,
26.4714865597197));
#29329=CARTESIAN_POINT('Ctrl Pts',(0.019106299236193,3.932953591047,26.4656144357537));
#29330=CARTESIAN_POINT('Ctrl Pts',(0.134668967232153,3.93239218729174,26.459749925113));
#29331=CARTESIAN_POINT('Ctrl Pts',(0.250365570827072,3.92673229458373,26.4538854144722));
#29332=CARTESIAN_POINT('Ctrl Pts',(0.365710255765519,3.91596029203922,26.4480209038315));
#29333=CARTESIAN_POINT('Ctrl Pts',(0.480936252170543,3.90519937377818,26.4421624277139));
#29334=CARTESIAN_POINT('Ctrl Pts',(0.595810641051473,3.88933684689728,26.4363039515963));
#29335=CARTESIAN_POINT('Ctrl Pts',(0.70984810413449,3.86841112978658,26.4304454754786));
#29336=CARTESIAN_POINT('Ctrl Pts',(0.828382215444494,3.84666028393134,26.4243559918874));
#29337=CARTESIAN_POINT('Ctrl Pts',(0.946011585862198,3.81943873873772,26.4182665082961));
#29338=CARTESIAN_POINT('Ctrl Pts',(1.06219727216592,3.78684908004046,26.4121770247049));
#29339=CARTESIAN_POINT('Ctrl Pts',(1.1738458170463,3.75553207286468,26.4063253401845));
#29340=CARTESIAN_POINT('Ctrl Pts',(1.28416088034434,3.71925846474617,26.400473655664));
#29341=CARTESIAN_POINT('Ctrl Pts',(1.39267596188823,3.67817110330374,26.3946219711436));
#29342=CARTESIAN_POINT('Ctrl Pts',(1.50117449252341,3.63709000857705,26.3887711791323));
#29343=CARTESIAN_POINT('Ctrl Pts',(1.60787320074873,3.59119676669917,26.382920387121));
#29344=CARTESIAN_POINT('Ctrl Pts',(1.71232333412656,3.5406832390664,26.3770695951096));
#29345=CARTESIAN_POINT('Ctrl Pts',(1.81678283548105,3.49016518095067,26.3712182783495));
#29346=CARTESIAN_POINT('Ctrl Pts',(1.91899298888713,3.43502619331729,26.3653669615894));
#29347=CARTESIAN_POINT('Ctrl Pts',(2.01852816331547,3.37550485911401,26.3595156448292));
#29348=CARTESIAN_POINT('Ctrl Pts',(2.11809637333762,3.315963769858,26.3536623860248));
#29349=CARTESIAN_POINT('Ctrl Pts',(2.2149874843812,3.25203765392655,26.3478091272203));
#29350=CARTESIAN_POINT('Ctrl Pts',(2.30880406081129,3.18400892096447,26.3419558684158));
#29351=CARTESIAN_POINT('Ctrl Pts',(2.40272737189701,3.11590279204889,26.3360959503876));
#29352=CARTESIAN_POINT('Ctrl Pts',(2.49356883180467,3.04368497267418,26.3302360323595));
#29353=CARTESIAN_POINT('Ctrl Pts',(2.5809633002183,2.96767879712853,26.3243761143314));
#29354=CARTESIAN_POINT('Ctrl Pts',(2.66841661382838,2.8916214444499,26.3185122506528));
#29355=CARTESIAN_POINT('Ctrl Pts',(2.75241801555775,2.8117709405761,26.3126483869742));
#29356=CARTESIAN_POINT('Ctrl Pts',(2.83263976556624,2.72848693574531,26.3067845232955));
#29357=CARTESIAN_POINT('Ctrl Pts',(2.91297986194377,2.64508006698336,26.3009120090081));
#29358=CARTESIAN_POINT('Ctrl Pts',(2.98952890581758,2.55822989696614,26.2950394947207));
#29359=CARTESIAN_POINT('Ctrl Pts',(3.06199984378537,2.46832857550578,26.2891669804333));
#29360=CARTESIAN_POINT('Ctrl Pts',(3.08202925733651,2.44348177764697,26.287543943385));
#29361=CARTESIAN_POINT('Ctrl Pts',(3.1017474231985,2.41840208184086,26.2859209063367));
#29362=CARTESIAN_POINT('Ctrl Pts',(3.12114888345207,2.39309812739175,26.2842978692884));
#29363=CARTESIAN_POINT('Ctrl Pts',(3.19146659825775,2.30138769791101,26.2784154122573));
#29364=CARTESIAN_POINT('Ctrl Pts',(3.25785940517396,2.20641799845255,26.2725329552262));
#29365=CARTESIAN_POINT('Ctrl Pts',(3.32001064603812,2.10855834877614,26.2666504981952));
#29366=CARTESIAN_POINT('Ctrl Pts',(3.3820820487949,2.01082440743814,26.2607755976381));
#29367=CARTESIAN_POINT('Ctrl Pts',(3.43992249984967,1.91020823968535,26.254900697081));
#29368=CARTESIAN_POINT('Ctrl Pts',(3.49325579813117,1.80711176434191,26.2490257965239));
#29369=CARTESIAN_POINT('Ctrl Pts',(3.54653333138522,1.70412308615265,26.2431570387332));
#29370=CARTESIAN_POINT('Ctrl Pts',(3.59531289573926,1.59865962005353,26.2372882809425));
#29371=CARTESIAN_POINT('Ctrl Pts',(3.63936218127963,1.4911512040942,26.2314195231518));
#29372=CARTESIAN_POINT('Ctrl Pts',(3.68337593372531,1.38372951160104,26.2255554994929));
#29373=CARTESIAN_POINT('Ctrl Pts',(3.72266684230552,1.27426652932657,26.2196914758341));
#29374=CARTESIAN_POINT('Ctrl Pts',(3.75704936513723,1.1632149706404,26.2138274521752));
#29375=CARTESIAN_POINT('Ctrl Pts',(3.79141352010128,1.05222273803521,26.2079665612013));
#29376=CARTESIAN_POINT('Ctrl Pts',(3.82087438444825,0.939644009115514,26.2021056702274));
#29377=CARTESIAN_POINT('Ctrl Pts',(3.84529545264423,0.825949079467748,26.1962447792534));
#29378=CARTESIAN_POINT('Ctrl Pts',(3.86970896790326,0.712289313336499,26.1903857009332));
#29379=CARTESIAN_POINT('Ctrl Pts',(3.88908570448811,0.597514435383587,26.184526622613));
#29380=CARTESIAN_POINT('Ctrl Pts',(3.90333986373395,0.482106739410929,26.1786675442928));
#29381=CARTESIAN_POINT('Ctrl Pts',(3.91759541092605,0.366687806038893,26.1728078954664));
#29382=CARTESIAN_POINT('Ctrl Pts',(3.92672733196767,0.250636339225301,26.16694824664));
#29383=CARTESIAN_POINT('Ctrl Pts',(3.93070153722025,0.134441159227153,26.1610885978136));
#29384=CARTESIAN_POINT('Ctrl Pts',(3.93226714142562,0.0886670607880611,
26.1587802392207));
#29385=CARTESIAN_POINT('Ctrl Pts',(3.93303288933878,0.0428706959530158,
26.1564718806279));
#29386=CARTESIAN_POINT('Ctrl Pts',(3.93299891753312,-0.00291799302117128,
26.154163522035));
#29387=CARTESIAN_POINT('',(3.93448863940243,-0.00148071873010509,24.904163522035));
#29388=CARTESIAN_POINT('Ctrl Pts',(3.93299891753245,-0.00291799392893486,
26.1541635219892));
#29389=CARTESIAN_POINT('Ctrl Pts',(3.93289966337747,-0.136697053654407,
26.1474192790553));
#29390=CARTESIAN_POINT('Ctrl Pts',(3.92597081494,-0.270198098326926,26.1406750361215));
#29391=CARTESIAN_POINT('Ctrl Pts',(3.91232098998049,-0.402782163654324,
26.1339307931876));
#29392=CARTESIAN_POINT('Ctrl Pts',(3.89859623802565,-0.536094013086838,
26.1271495295696));
#29393=CARTESIAN_POINT('Ctrl Pts',(3.87807663698307,-0.668478652679353,
26.1203682659515));
#29394=CARTESIAN_POINT('Ctrl Pts',(3.85092187812462,-0.799305754127397,
26.1135870023335));
#29395=CARTESIAN_POINT('Ctrl Pts',(3.8235914984607,-0.930978967339932,26.1067618815417));
#29396=CARTESIAN_POINT('Ctrl Pts',(3.78953995026768,-1.06107429835095,26.0999367607498));
#29397=CARTESIAN_POINT('Ctrl Pts',(3.74897826520204,-1.18897054927476,26.093111639958));
#29398=CARTESIAN_POINT('Ctrl Pts',(3.73363203755879,-1.23735919432781,26.0905294036137));
#29399=CARTESIAN_POINT('Ctrl Pts',(3.71735441033018,-1.28543328393037,26.0879471672693));
#29400=CARTESIAN_POINT('Ctrl Pts',(3.70015855625265,-1.33316002737492,26.085364930925));
#29401=CARTESIAN_POINT('Ctrl Pts',(3.66105439482825,-1.44169283252097,26.079492806959));
#29402=CARTESIAN_POINT('Ctrl Pts',(3.617105411396,-1.54868563171675,26.0736206829929));
#29403=CARTESIAN_POINT('Ctrl Pts',(3.5684521309445,-1.65367420889293,26.0677485590269));
#29404=CARTESIAN_POINT('Ctrl Pts',(3.51986193043716,-1.75852666629416,26.0618840483862));
#29405=CARTESIAN_POINT('Ctrl Pts',(3.46657973425262,-1.86137969755,26.0560195377455));
#29406=CARTESIAN_POINT('Ctrl Pts',(3.40879529535264,-1.96178582785728,26.0501550271048));
#29407=CARTESIAN_POINT('Ctrl Pts',(3.35107031606528,-2.06208864125563,26.0442965509872));
#29408=CARTESIAN_POINT('Ctrl Pts',(3.28885251381732,-2.15994920564826,26.0384380748695));
#29409=CARTESIAN_POINT('Ctrl Pts',(3.22237874009188,-2.25494218449251,26.0325795987519));
#29410=CARTESIAN_POINT('Ctrl Pts',(3.15328381741514,-2.35368086232338,26.0264901151607));
#29411=CARTESIAN_POINT('Ctrl Pts',(3.07959057234702,-2.44932074385272,26.0204006315694));
#29412=CARTESIAN_POINT('Ctrl Pts',(3.00161651713324,-2.54141442588038,26.0143111479781));
#29413=CARTESIAN_POINT('Ctrl Pts',(2.92668740942666,-2.629911777991,26.0084594634577));
#29414=CARTESIAN_POINT('Ctrl Pts',(2.84780584776093,-2.71513435167606,26.0026077789373));
#29415=CARTESIAN_POINT('Ctrl Pts',(2.76529581629403,-2.79671737012998,25.9967560944169));
#29416=CARTESIAN_POINT('Ctrl Pts',(2.68279836940049,-2.87828794540017,25.9909053024056));
#29417=CARTESIAN_POINT('Ctrl Pts',(2.5966738469717,-2.95621977858374,25.9850545103943));
#29418=CARTESIAN_POINT('Ctrl Pts',(2.50728341954857,-3.03018462375757,25.979203718383));
#29419=CARTESIAN_POINT('Ctrl Pts',(2.41788497483111,-3.10415610272824,25.9733524016228));
#29420=CARTESIAN_POINT('Ctrl Pts',(2.32522036136615,-3.1741596228391,25.9675010848627));
#29421=CARTESIAN_POINT('Ctrl Pts',(2.22968361594949,-3.23990740188148,25.9616497681026));
#29422=CARTESIAN_POINT('Ctrl Pts',(2.13411516201201,-3.30567700252571,25.955796509298));
#29423=CARTESIAN_POINT('Ctrl Pts',(2.03567302101281,-3.36718781924058,25.9499432504935));
#29424=CARTESIAN_POINT('Ctrl Pts',(1.93477935256376,-3.42419594312197,25.944089991689));
#29425=CARTESIAN_POINT('Ctrl Pts',(1.83377089788687,-3.48126892486408,25.9382300736609));
#29426=CARTESIAN_POINT('Ctrl Pts',(1.73030570895415,-3.53382878552301,25.9323701556328));
#29427=CARTESIAN_POINT('Ctrl Pts',(1.62482972346511,-3.58167801033877,25.9265102376046));
#29428=CARTESIAN_POINT('Ctrl Pts',(1.51928271797639,-3.62955945340701,25.920646373926));
#29429=CARTESIAN_POINT('Ctrl Pts',(1.41172260273298,-3.67272379135267,25.9147825102474));
#29430=CARTESIAN_POINT('Ctrl Pts',(1.30261277864833,-3.7110226284546,25.9089186465687));
#29431=CARTESIAN_POINT('Ctrl Pts',(1.1933419913402,-3.74937796554932,25.9030461322813));
#29432=CARTESIAN_POINT('Ctrl Pts',(1.08251732664487,-3.78285335718474,25.8971736179939));
#29433=CARTESIAN_POINT('Ctrl Pts',(0.970614811177254,-3.81135092694485,
25.8913011037065));
#29434=CARTESIAN_POINT('Ctrl Pts',(0.939687354977304,-3.81922704426784,
25.8896780666582));
#29435=CARTESIAN_POINT('Ctrl Pts',(0.908677608991107,-3.826723234007,25.8880550296099));
#29436=CARTESIAN_POINT('Ctrl Pts',(0.877595700063934,-3.83383812741609,
25.8864319925615));
#29437=CARTESIAN_POINT('Ctrl Pts',(0.765141814610416,-3.85957970623335,
25.8805598685955));
#29438=CARTESIAN_POINT('Ctrl Pts',(0.651365865963002,-3.88041251050638,
25.8746877446294));
#29439=CARTESIAN_POINT('Ctrl Pts',(0.536734397292292,-3.89620394573529,
25.8688156206634));
#29440=CARTESIAN_POINT('Ctrl Pts',(0.422251550596811,-3.91197490705488,
25.8629511100227));
#29441=CARTESIAN_POINT('Ctrl Pts',(0.306915795431241,-3.92271744163368,
25.857086599382));
#29442=CARTESIAN_POINT('Ctrl Pts',(0.191206188388593,-3.92834942355207,
25.8512220887413));
#29443=CARTESIAN_POINT('Ctrl Pts',(0.0756156453804744,-3.9339756102171,
25.8453636126236));
#29444=CARTESIAN_POINT('Ctrl Pts',(-0.0403475739007709,-3.9345016840641,
25.839505136506));
#29445=CARTESIAN_POINT('Ctrl Pts',(-0.156197591340927,-3.92989711219763,
25.8336466603884));
#29446=CARTESIAN_POINT('Ctrl Pts',(-0.276615728427646,-3.92511097596309,
25.8275571767972));
#29447=CARTESIAN_POINT('Ctrl Pts',(-0.396911101818345,-3.91478119143449,
25.8214676932059));
#29448=CARTESIAN_POINT('Ctrl Pts',(-0.516535680730198,-3.89893317338636,
25.8153782096146));
#29449=CARTESIAN_POINT('Ctrl Pts',(-0.631488826787159,-3.88370403277017,
25.8095265250942));
#29450=CARTESIAN_POINT('Ctrl Pts',(-0.745822136886534,-3.86337961302313,
25.8036748405738));
#29451=CARTESIAN_POINT('Ctrl Pts',(-0.8590536084657,-3.83803542164244,25.7978231560534));
#29452=CARTESIAN_POINT('Ctrl Pts',(-0.972267809784176,-3.81269509580184,
25.7919723640421));
#29453=CARTESIAN_POINT('Ctrl Pts',(-1.08438010340781,-3.78233661090202,
25.7861215720308));
#29454=CARTESIAN_POINT('Ctrl Pts',(-1.19491913180823,-3.74708650399729,
25.7802707800195));
#29455=CARTESIAN_POINT('Ctrl Pts',(-1.3054680742894,-3.71183323556301,25.7744194632594));
#29456=CARTESIAN_POINT('Ctrl Pts',(-1.41444307715194,-3.67168759859424,
25.7685681464992));
#29457=CARTESIAN_POINT('Ctrl Pts',(-1.52138907152239,-3.62682564966283,
25.7627168297391));
#29458=CARTESIAN_POINT('Ctrl Pts',(-1.62837056112883,-3.58194881110911,
25.7568635709346));
#29459=CARTESIAN_POINT('Ctrl Pts',(-1.73332132215295,-3.53235270785515,
25.75101031213));
#29460=CARTESIAN_POINT('Ctrl Pts',(-1.83580800645435,-3.47826076702683,
25.7451570533255));
#29461=CARTESIAN_POINT('Ctrl Pts',(-1.93841128934952,-3.42410728606501,
25.7392971352974));
#29462=CARTESIAN_POINT('Ctrl Pts',(-2.03854453424244,-3.3654479514235,25.7334372172693));
#29463=CARTESIAN_POINT('Ctrl Pts',(-2.13580058252971,-3.30255126707607,
25.7275772992412));
#29464=CARTESIAN_POINT('Ctrl Pts',(-2.23312211609763,-3.23961223259105,
25.7217134355625));
#29465=CARTESIAN_POINT('Ctrl Pts',(-2.3275622594692,-3.1724304063178,25.7158495718839));
#29466=CARTESIAN_POINT('Ctrl Pts',(-2.41874574864605,-3.10131552786985,
25.7099857082053));
#29467=CARTESIAN_POINT('Ctrl Pts',(-2.51006375539251,-3.03009573787817,
25.7041131939179));
#29468=CARTESIAN_POINT('Ctrl Pts',(-2.59811520610508,-2.95493158300759,
25.6982406796305));
#29469=CARTESIAN_POINT('Ctrl Pts',(-2.68256052357199,-2.87617072465686,
25.6923681653431));
#29470=CARTESIAN_POINT('Ctrl Pts',(-2.70589939889837,-2.85440291196118,
25.6907451282948));
#29471=CARTESIAN_POINT('Ctrl Pts',(-2.728963052369,-2.83236056418945,25.6891220912465));
#29472=CARTESIAN_POINT('Ctrl Pts',(-2.75174486024567,-2.81005146289379,
25.6874990541981));
#29473=CARTESIAN_POINT('Ctrl Pts',(-2.83416910321691,-2.72933746532088,
25.6816269302321));
#29474=CARTESIAN_POINT('Ctrl Pts',(-2.91317727188268,-2.6448585832937,25.6757548062661));
#29475=CARTESIAN_POINT('Ctrl Pts',(-2.98840570014136,-2.5569357386064,25.6698826823001));
#29476=CARTESIAN_POINT('Ctrl Pts',(-3.06353659324907,-2.46912688763302,
25.6640181716593));
#29477=CARTESIAN_POINT('Ctrl Pts',(-3.13489722499802,-2.37788326481389,
25.6581536610186));
#29478=CARTESIAN_POINT('Ctrl Pts',(-3.2021596340609,-2.28356359184302,25.6522891503779));
#29479=CARTESIAN_POINT('Ctrl Pts',(-3.26935283077402,-2.18934097287727,
25.6464306742603));
#29480=CARTESIAN_POINT('Ctrl Pts',(-3.33245595408606,-2.09204893410727,
25.6405721981427));
#29481=CARTESIAN_POINT('Ctrl Pts',(-3.39118076920397,-1.99207981531392,
25.6347137220251));
#29482=CARTESIAN_POINT('Ctrl Pts',(-3.45222118157091,-1.888168781744,25.6286242384338));
#29483=CARTESIAN_POINT('Ctrl Pts',(-3.50853060137652,-1.78136554888669,
25.6225347548426));
#29484=CARTESIAN_POINT('Ctrl Pts',(-3.55983428648306,-1.67214498557381,
25.6164452712513));
#29485=CARTESIAN_POINT('Ctrl Pts',(-3.60913452278029,-1.56718957021407,
25.6105935867309));
#29486=CARTESIAN_POINT('Ctrl Pts',(-3.65381245120797,-1.46000248821375,
25.6047419022105));
#29487=CARTESIAN_POINT('Ctrl Pts',(-3.69367115793895,-1.35103011698849,
25.5988902176901));
#29488=CARTESIAN_POINT('Ctrl Pts',(-3.73352378535073,-1.24207436641863,
25.5930394256788));
#29489=CARTESIAN_POINT('Ctrl Pts',(-3.76855851057502,-1.13133425618119,
25.5871886336675));
#29490=CARTESIAN_POINT('Ctrl Pts',(-3.79862711020792,-1.01927478022045,
25.5813378416562));
#29491=CARTESIAN_POINT('Ctrl Pts',(-3.82869840664872,-0.907205253812249,
25.575486524896));
#29492=CARTESIAN_POINT('Ctrl Pts',(-3.85380258492889,-0.793816525759676,
25.5696352081359));
#29493=CARTESIAN_POINT('Ctrl Pts',(-3.87384189097495,-0.679586641810747,
25.5637838913758));
#29494=CARTESIAN_POINT('Ctrl Pts',(-3.89388784804053,-0.565318845112445,
25.5579306325712));
#29495=CARTESIAN_POINT('Ctrl Pts',(-3.90886551886826,-0.450209744368547,
25.5520773737667));
#29496=CARTESIAN_POINT('Ctrl Pts',(-3.91872874569848,-0.334744705165609,
25.5462241149622));
#29497=CARTESIAN_POINT('Ctrl Pts',(-3.92860319387308,-0.219148301958656,
25.5403641969341));
#29498=CARTESIAN_POINT('Ctrl Pts',(-3.93335154891644,-0.103195564182696,
25.5345042789059));
#29499=CARTESIAN_POINT('Ctrl Pts',(-3.93297973407051,0.0126258223746364,
25.5286443608778));
#29500=CARTESIAN_POINT('Ctrl Pts',(-3.93260766887101,0.128525194786199,
25.5227804971992));
#29501=CARTESIAN_POINT('Ctrl Pts',(-3.92710858858938,0.244292627933414,
25.5169166335206));
#29502=CARTESIAN_POINT('Ctrl Pts',(-3.91654034803666,0.359444991898466,
25.5110527698419));
#29503=CARTESIAN_POINT('Ctrl Pts',(-3.90595651678822,0.474767233286212,
25.5051802555545));
#29504=CARTESIAN_POINT('Ctrl Pts',(-3.89028865584999,0.58947218646435,25.4993077412671));
#29505=CARTESIAN_POINT('Ctrl Pts',(-3.86964581228303,0.703086258918789,
25.4934352269798));
#29506=CARTESIAN_POINT('Ctrl Pts',(-3.86394057288252,0.734486752775978,
25.4918121899314));
#29507=CARTESIAN_POINT('Ctrl Pts',(-3.85785561268348,0.765804007861907,
25.4901891528831));
#29508=CARTESIAN_POINT('Ctrl Pts',(-3.85139390028731,0.797028245942219,
25.4885661158347));
#29509=CARTESIAN_POINT('Ctrl Pts',(-3.82801552068608,0.909997076160167,
25.4826939918687));
#29510=CARTESIAN_POINT('Ctrl Pts',(-3.79962334186986,1.02212582540209,25.4768218679026));
#29511=CARTESIAN_POINT('Ctrl Pts',(-3.76629089470126,1.13293508043946,25.4709497439366));
#29512=CARTESIAN_POINT('Ctrl Pts',(-3.73300166371225,1.2436006690775,25.4650852332959));
#29513=CARTESIAN_POINT('Ctrl Pts',(-3.69478501988866,1.3529497733429,25.4592207226552));
#29514=CARTESIAN_POINT('Ctrl Pts',(-3.6517655935033,1.46051259840697,25.4533562120144));
#29515=CARTESIAN_POINT('Ctrl Pts',(-3.60879043367971,1.56796474239413,25.4474977358968));
#29516=CARTESIAN_POINT('Ctrl Pts',(-3.56102247379366,1.67363388163584,25.4416392597792));
#29517=CARTESIAN_POINT('Ctrl Pts',(-3.50863609792475,1.77706548341342,25.4357807836616));
#29518=CARTESIAN_POINT('Ctrl Pts',(-3.45418405786254,1.88457553025815,25.4296913000703));
#29519=CARTESIAN_POINT('Ctrl Pts',(-3.39474201927504,1.98966751547195,25.4236018164791));
#29520=CARTESIAN_POINT('Ctrl Pts',(-3.33056110036188,2.0918536652348,25.4175123328878));
#29521=CARTESIAN_POINT('Ctrl Pts',(-3.26888649625454,2.1900493663653,25.4116606483674));
#29522=CARTESIAN_POINT('Ctrl Pts',(-3.20283642093734,2.28556154039003,25.405808963847));
#29523=CARTESIAN_POINT('Ctrl Pts',(-3.13268007309228,2.37798329675601,25.3999572793266));
#29524=CARTESIAN_POINT('Ctrl Pts',(-3.06253442561529,2.47039095679511,25.3941064873153));
#29525=CARTESIAN_POINT('Ctrl Pts',(-2.9882840007727,2.55970880718147,25.388255695304));
#29526=CARTESIAN_POINT('Ctrl Pts',(-2.91023997173198,2.64556086812105,25.3824049032927));
#29527=CARTESIAN_POINT('Ctrl Pts',(-2.83218894303857,2.73142062900408,25.3765535865325));
#29528=CARTESIAN_POINT('Ctrl Pts',(-2.75034391187737,2.81381367659142,25.3707022697724));
#29529=CARTESIAN_POINT('Ctrl Pts',(-2.66505430473762,2.89239944558138,25.3648509530123));
#29530=CARTESIAN_POINT('Ctrl Pts',(-2.57973639008858,2.97101129708551,25.3589976942077));
#29531=CARTESIAN_POINT('Ctrl Pts',(-2.49097193005286,3.04581307735888,25.3531444354032));
#29532=CARTESIAN_POINT('Ctrl Pts',(-2.39914439028916,3.11650368113757,25.3472911765987));
#29533=CARTESIAN_POINT('Ctrl Pts',(-2.30721237878769,3.18727470926652,25.3414312585706));
#29534=CARTESIAN_POINT('Ctrl Pts',(-2.21221065967174,3.2539249728697,25.3355713405424));
#29535=CARTESIAN_POINT('Ctrl Pts',(-2.11455279276547,3.31619593610024,25.3297114225143));
#29536=CARTESIAN_POINT('Ctrl Pts',(-2.01682917002254,3.37850882815246,25.3238475588357));
#29537=CARTESIAN_POINT('Ctrl Pts',(-1.9164461955111,3.4364363422514,25.3179836951571));
#29538=CARTESIAN_POINT('Ctrl Pts',(-1.81384165666161,3.4897661016978,25.3121198314784));
#29539=CARTESIAN_POINT('Ctrl Pts',(-1.71108575144835,3.54317453536134,25.306247317191));
#29540=CARTESIAN_POINT('Ctrl Pts',(-1.60610211442283,3.59197150357526,25.3003748029036));
#29541=CARTESIAN_POINT('Ctrl Pts',(-1.49934816946151,3.63599285845454,25.2945022886162));
#29542=CARTESIAN_POINT('Ctrl Pts',(-1.46984366776945,3.64815941717041,25.2928792515679));
#29543=CARTESIAN_POINT('Ctrl Pts',(-1.44020402538699,3.65996148504733,25.2912562145196));
#29544=CARTESIAN_POINT('Ctrl Pts',(-1.41043907420642,3.67139627634388,25.2896331774712));
#29545=CARTESIAN_POINT('Ctrl Pts',(-1.30274992234525,3.71276718164,25.2837610535052));
#29546=CARTESIAN_POINT('Ctrl Pts',(-1.19305845469924,3.74946533077809,25.2778889295392));
#29547=CARTESIAN_POINT('Ctrl Pts',(-1.08180780184001,3.78129354584884,25.2720168055731));
#29548=CARTESIAN_POINT('Ctrl Pts',(-0.970701387661206,3.81308049500677,
25.2661522949324));
#29549=CARTESIAN_POINT('Ctrl Pts',(-0.85804020212067,3.84000995362343,25.2602877842917));
#29550=CARTESIAN_POINT('Ctrl Pts',(-0.744286893916767,3.86193293825045,
25.254423273651));
#29551=CARTESIAN_POINT('Ctrl Pts',(-0.630650636735293,3.88383336434439,
25.2485647975334));
#29552=CARTESIAN_POINT('Ctrl Pts',(-0.515924895647223,3.90073748548584,
25.2427063214157));
#29553=CARTESIAN_POINT('Ctrl Pts',(-0.400586361530146,3.91254643000643,
25.2368478452981));
#29554=CARTESIAN_POINT('Ctrl Pts',(-0.280699876231519,3.92482101685199,
25.2307583617069));
#29555=CARTESIAN_POINT('Ctrl Pts',(-0.160151714701411,3.93159021616369,
25.2246688781156));
#29556=CARTESIAN_POINT('Ctrl Pts',(-0.0394880013778991,3.93280176181653,
25.2185793945244));
#29557=CARTESIAN_POINT('Ctrl Pts',(0.0764637000837605,3.93396599566923,
25.2127277100039));
#29558=CARTESIAN_POINT('Ctrl Pts',(0.192521645583772,3.92999848729926,25.2068760254835));
#29559=CARTESIAN_POINT('Ctrl Pts',(0.308197999499315,3.92090588934555,25.2010243409631));
#29560=CARTESIAN_POINT('Ctrl Pts',(0.423856710256336,3.91181467821068,25.1951735489518));
#29561=CARTESIAN_POINT('Ctrl Pts',(0.53913353312302,3.89759996411879,25.1893227569405));
#29562=CARTESIAN_POINT('Ctrl Pts',(0.653543961263525,3.87832042135458,25.1834719649292));
#29563=CARTESIAN_POINT('Ctrl Pts',(0.767964650704958,3.85903914943689,25.1776206481691));
#29564=CARTESIAN_POINT('Ctrl Pts',(0.881518383259193,3.83469221452647,25.1717693314089));
#29565=CARTESIAN_POINT('Ctrl Pts',(0.99372978122933,3.80538961499318,25.1659180146488));
#29566=CARTESIAN_POINT('Ctrl Pts',(1.10597842201578,3.7760772899654,25.1600647558443));
#29567=CARTESIAN_POINT('Ctrl Pts',(1.21688344254487,3.74180613417929,25.1542114970398));
#29568=CARTESIAN_POINT('Ctrl Pts',(1.32598427545732,3.7027361101272,25.1483582382352));
#29569=CARTESIAN_POINT('Ctrl Pts',(1.4352092318479,3.66362163630194,25.1424983202071));
#29570=CARTESIAN_POINT('Ctrl Pts',(1.54262551421503,3.61969753635897,25.136638402179));
#29571=CARTESIAN_POINT('Ctrl Pts',(1.64779211357284,3.57117209756785,25.1307784841509));
#29572=CARTESIAN_POINT('Ctrl Pts',(1.75302952461166,3.52261398521009,25.1249146204722));
#29573=CARTESIAN_POINT('Ctrl Pts',(1.85601386997303,3.46944855403605,25.1190507567936));
#29574=CARTESIAN_POINT('Ctrl Pts',(1.95632988957584,3.4119294194271,25.113186893115));
#29575=CARTESIAN_POINT('Ctrl Pts',(2.05679389942638,3.35432543026538,25.1073143788276));
#29576=CARTESIAN_POINT('Ctrl Pts',(2.1545813792611,3.29235513949992,25.1014418645402));
#29577=CARTESIAN_POINT('Ctrl Pts',(2.24930704023069,3.22631474576933,25.0955693502528));
#29578=CARTESIAN_POINT('Ctrl Pts',(2.27548718210135,3.20806259678073,25.0939463132045));
#29579=CARTESIAN_POINT('Ctrl Pts',(2.30143364910518,3.18949978296553,25.0923232761561));
#29580=CARTESIAN_POINT('Ctrl Pts',(2.32713878456213,3.17063307201995,25.0907002391078));
#29581=CARTESIAN_POINT('Ctrl Pts',(2.41929313316304,3.10299485784508,25.0848815604942));
#29582=CARTESIAN_POINT('Ctrl Pts',(2.50866441508414,3.03121193412896,25.0790628818805));
#29583=CARTESIAN_POINT('Ctrl Pts',(2.59485131254487,2.95554320993352,25.0732442032669));
#29584=CARTESIAN_POINT('Ctrl Pts',(2.68092610598529,2.87997290868223,25.0674330930573));
#29585=CARTESIAN_POINT('Ctrl Pts',(2.76382443478544,2.80052712962886,25.0616219828477));
#29586=CARTESIAN_POINT('Ctrl Pts',(2.8431746241309,2.71750750812175,25.0558108726382));
#29587=CARTESIAN_POINT('Ctrl Pts',(2.92244380484517,2.63457264137019,25.0500056949927));
#29588=CARTESIAN_POINT('Ctrl Pts',(2.9981717587886,2.54807148956562,25.0442005173472));
#29589=CARTESIAN_POINT('Ctrl Pts',(3.07002114095011,2.45834480781671,25.0383953397017));
#29590=CARTESIAN_POINT('Ctrl Pts',(3.14181856355304,2.36868301401307,25.032594360206));
#29591=CARTESIAN_POINT('Ctrl Pts',(3.2097427294854,2.27580065696699,25.0267933807103));
#29592=CARTESIAN_POINT('Ctrl Pts',(3.27349484603802,2.18007350632095,25.0209924012146));
#29593=CARTESIAN_POINT('Ctrl Pts',(3.33722298896874,2.08438235332706,25.0151936031443));
#29594=CARTESIAN_POINT('Ctrl Pts',(3.3967819668782,1.98584888317275,25.0093948050741));
#29595=CARTESIAN_POINT('Ctrl Pts',(3.45191522647188,1.88487937790502,25.0035960070038));
#29596=CARTESIAN_POINT('Ctrl Pts',(3.50704170690549,1.78392228780088,24.9977979219511));
#29597=CARTESIAN_POINT('Ctrl Pts',(3.55774334901334,1.68053012824946,24.9919998368983));
#29598=CARTESIAN_POINT('Ctrl Pts',(3.60380905841642,1.57513468328133,24.9862017518456));
#29599=CARTESIAN_POINT('Ctrl Pts',(3.64988076245597,1.46972552296207,24.9804029122747));
#29600=CARTESIAN_POINT('Ctrl Pts',(3.69131516671325,1.36231294586496,24.9746040727039));
#29601=CARTESIAN_POINT('Ctrl Pts',(3.72794924521417,1.25334888403312,24.968805233133));
#29602=CARTESIAN_POINT('Ctrl Pts',(3.76461888331469,1.14427905405952,24.9630007648028));
#29603=CARTESIAN_POINT('Ctrl Pts',(3.79647875699002,1.0336551325787,24.9571962964725));
#29604=CARTESIAN_POINT('Ctrl Pts',(3.82341568735235,0.92194440272066,24.9513918281423));
#29605=CARTESIAN_POINT('Ctrl Pts',(3.85036646612251,0.810176241829282,24.9455843757065));
#29606=CARTESIAN_POINT('Ctrl Pts',(3.87238918170624,0.697320573739987,24.9397769232706));
#29607=CARTESIAN_POINT('Ctrl Pts',(3.88942211602274,0.583853237888747,24.9339694708348));
#29608=CARTESIAN_POINT('Ctrl Pts',(3.90648102119818,0.470212893434376,24.9281531635226));
#29609=CARTESIAN_POINT('Ctrl Pts',(3.91853490722703,0.355959437785159,24.9223368562104));
#29610=CARTESIAN_POINT('Ctrl Pts',(3.92557406855906,0.241572416175038,24.9165205488981));
#29611=CARTESIAN_POINT('Ctrl Pts',(3.93055908173005,0.160565491852631,24.9124015399438));
#29612=CARTESIAN_POINT('Ctrl Pts',(3.93303019466974,0.0794916235615288,
24.9082825309894));
#29613=CARTESIAN_POINT('Ctrl Pts',(3.93299972147611,-0.00148015838570855,
24.904163522035));
#29614=CARTESIAN_POINT('',(3.93299834039037,0.00361309930207936,23.654163522035));
#29615=CARTESIAN_POINT('Ctrl Pts',(3.93885394375624,-0.00148236158347574,
24.904163522035));
#29616=CARTESIAN_POINT('Ctrl Pts',(3.93924552707134,-0.082832039204855,
24.9000314482714));
#29617=CARTESIAN_POINT('Ctrl Pts',(3.90002134205164,-1.46928590995256,24.8295883950541));
#29618=CARTESIAN_POINT('Ctrl Pts',(2.26524006589229,-4.06362187352642,24.6928343623803));
#29619=CARTESIAN_POINT('Ctrl Pts',(-2.19528402354312,-4.10183658171443,
24.4939014240179));
#29620=CARTESIAN_POINT('Ctrl Pts',(-4.63767356163746,-0.369214331799999,
24.2949684856538));
#29621=CARTESIAN_POINT('Ctrl Pts',(-2.81662877770042,3.70282832652962,24.0960355472907));
#29622=CARTESIAN_POINT('Ctrl Pts',(1.59375560585921,4.37084412395475,23.897102608927));
#29623=CARTESIAN_POINT('Ctrl Pts',(3.77442032009617,1.89040227389705,23.749811933842));
#29624=CARTESIAN_POINT('Ctrl Pts',(3.93617122324185,0.293430403295199,23.6688322382112));
#29625=CARTESIAN_POINT('Ctrl Pts',(3.93347523015726,0.00361353740297166,
23.654163522035));
#29626=CARTESIAN_POINT('',(3.9329999986383,-0.000103494422979276,22.404163521994));
#29627=CARTESIAN_POINT('Ctrl Pts',(3.93299834039037,0.00361309930207936,
23.654163522035));
#29628=CARTESIAN_POINT('Ctrl Pts',(3.93310324074698,-0.110574996279411,
23.6483832801292));
#29629=CARTESIAN_POINT('Ctrl Pts',(3.92823105114043,-0.224912019346994,
23.6426030382233));
#29630=CARTESIAN_POINT('Ctrl Pts',(3.91836963887632,-0.338922370362654,
23.6368227963175));
#29631=CARTESIAN_POINT('Ctrl Pts',(3.90851599762897,-0.452842878633289,
23.6310471093735));
#29632=CARTESIAN_POINT('Ctrl Pts',(3.89368098718194,-0.56643680435109,23.6252714224295));
#29633=CARTESIAN_POINT('Ctrl Pts',(3.87390454030067,-0.679229425627184,
23.6194957354855));
#29634=CARTESIAN_POINT('Ctrl Pts',(3.85413638626874,-0.791974749619789,
23.6137224704579));
#29635=CARTESIAN_POINT('Ctrl Pts',(3.82943098567734,-0.903919018186908,
23.6079492054304));
#29636=CARTESIAN_POINT('Ctrl Pts',(3.79987994024537,-1.01459422417083,23.6021759404028));
#29637=CARTESIAN_POINT('Ctrl Pts',(3.77033367427634,-1.12525153000818,23.5964036091191));
#29638=CARTESIAN_POINT('Ctrl Pts',(3.73594343083082,-1.23463977005716,23.5906312778354));
#29639=CARTESIAN_POINT('Ctrl Pts',(3.69685138311993,-1.34230356146597,23.5848589465517));
#29640=CARTESIAN_POINT('Ctrl Pts',(3.65775558785716,-1.44997767404414,23.5790860619045));
#29641=CARTESIAN_POINT('Ctrl Pts',(3.61395723875769,-1.55592660967396,23.5733131772573));
#29642=CARTESIAN_POINT('Ctrl Pts',(3.56564729055769,-1.65971334854505,23.5675402926101));
#29643=CARTESIAN_POINT('Ctrl Pts',(3.51728957372828,-1.76360271121209,23.5617616997641));
#29644=CARTESIAN_POINT('Ctrl Pts',(3.46441152820581,-1.86532522057124,23.5559831069181));
#29645=CARTESIAN_POINT('Ctrl Pts',(3.40725089991998,-1.96446692641909,23.5502045140722));
#29646=CARTESIAN_POINT('Ctrl Pts',(3.35006228571326,-2.06365717218017,23.5444230920193));
#29647=CARTESIAN_POINT('Ctrl Pts',(3.28858714318448,-2.16026374001438,23.5386416699665));
#29648=CARTESIAN_POINT('Ctrl Pts',(3.22310645749673,-2.25390189751969,23.5328602479136));
#29649=CARTESIAN_POINT('Ctrl Pts',(3.15751781001056,-2.3476944416778,23.5270692936955));
#29650=CARTESIAN_POINT('Ctrl Pts',(3.08791068603683,-2.4385084610394,23.5212783394773));
#29651=CARTESIAN_POINT('Ctrl Pts',(3.01460647383614,-2.52599224224961,23.5154873852591));
#29652=CARTESIAN_POINT('Ctrl Pts',(2.94603738744473,-2.60782496061002,23.5100705009062));
#29653=CARTESIAN_POINT('Ctrl Pts',(2.87423399507358,-2.68674392815123,23.5046536165532));
#29654=CARTESIAN_POINT('Ctrl Pts',(2.79948658977658,-2.76249232282392,23.4992367322003));
#29655=CARTESIAN_POINT('Ctrl Pts',(2.71845734834484,-2.84460667763814,23.4933646082343));
#29656=CARTESIAN_POINT('Ctrl Pts',(2.63367633994529,-2.92329055679529,23.4874924842682));
#29657=CARTESIAN_POINT('Ctrl Pts',(2.54546587752598,-2.99818152658422,23.4816203603022));
#29658=CARTESIAN_POINT('Ctrl Pts',(2.45736978172267,-3.07297539874381,23.4757558496615));
#29659=CARTESIAN_POINT('Ctrl Pts',(2.36585338632428,-3.14398587573166,23.4698913390208));
#29660=CARTESIAN_POINT('Ctrl Pts',(2.27127666708625,-3.21088637319193,23.4640268283801));
#29661=CARTESIAN_POINT('Ctrl Pts',(2.17679726635115,-3.27771803070604,23.4581683522625));
#29662=CARTESIAN_POINT('Ctrl Pts',(2.07926414084847,-3.34044788332413,23.4523098761448));
#29663=CARTESIAN_POINT('Ctrl Pts',(1.97907073194804,-3.3987892017521,23.4464514000272));
#29664=CARTESIAN_POINT('Ctrl Pts',(1.87492656421521,-3.45943099564649,23.4403619164359));
#29665=CARTESIAN_POINT('Ctrl Pts',(1.76790834682957,-3.51533074927043,23.4342724328447));
#29666=CARTESIAN_POINT('Ctrl Pts',(1.6584919979043,-3.56621554212409,23.4281829492534));
#29667=CARTESIAN_POINT('Ctrl Pts',(1.5533484425126,-3.61511324423675,23.422331264733));
#29668=CARTESIAN_POINT('Ctrl Pts',(1.44599094880336,-3.65938012102753,23.4164795802126));
#29669=CARTESIAN_POINT('Ctrl Pts',(1.33686664545719,-3.6988209705613,23.4106278956922));
#29670=CARTESIAN_POINT('Ctrl Pts',(1.22775898593937,-3.73825580450817,23.4047771036809));
#29671=CARTESIAN_POINT('Ctrl Pts',(1.11688544127904,-3.77286593425945,23.3989263116696));
#29672=CARTESIAN_POINT('Ctrl Pts',(1.00471156997488,-3.80250491928132,23.3930755196583));
#29673=CARTESIAN_POINT('Ctrl Pts',(0.892527637963276,-3.83214656257961,
23.3872242028981));
#29674=CARTESIAN_POINT('Ctrl Pts',(0.77904354718896,-3.85681606921526,23.381372886138));
#29675=CARTESIAN_POINT('Ctrl Pts',(0.664737714468218,-3.87641751762675,
23.3755215693778));
#29676=CARTESIAN_POINT('Ctrl Pts',(0.55039394379119,-3.89602547173332,23.3696683105733));
#29677=CARTESIAN_POINT('Ctrl Pts',(0.435228296101503,-3.91056195306942,
23.3638150517688));
#29678=CARTESIAN_POINT('Ctrl Pts',(0.319726310291494,-3.919982664057,23.3579617929643));
#29679=CARTESIAN_POINT('Ctrl Pts',(0.204092918443143,-3.92941409294089,
23.3521018749362));
#29680=CARTESIAN_POINT('Ctrl Pts',(0.0881228370050104,-3.9337181009102,
23.3462419569081));
#29681=CARTESIAN_POINT('Ctrl Pts',(-0.0276962745125356,-3.93290247989676,
23.3403820388799));
#29682=CARTESIAN_POINT('Ctrl Pts',(-0.14359337035263,-3.93208630970236,
23.3345181752013));
#29683=CARTESIAN_POINT('Ctrl Pts',(-0.259338882001057,-3.92614366763592,
23.3286543115227));
#29684=CARTESIAN_POINT('Ctrl Pts',(-0.374449904777226,-3.91513425935974,
23.322790447844));
#29685=CARTESIAN_POINT('Ctrl Pts',(-0.489730743987692,-3.9041086095594,
23.3169179335566));
#29686=CARTESIAN_POINT('Ctrl Pts',(-0.604374818337527,-3.88800133274279,
23.3110454192692));
#29687=CARTESIAN_POINT('Ctrl Pts',(-0.717908956640308,-3.86692328990059,
23.3051729049819));
#29688=CARTESIAN_POINT('Ctrl Pts',(-0.749287358411539,-3.86109777075066,
23.3035498679335));
#29689=CARTESIAN_POINT('Ctrl Pts',(-0.780581066993679,-3.8548928525475,
23.3019268308852));
#29690=CARTESIAN_POINT('Ctrl Pts',(-0.811780315599351,-3.84831154133932,
23.3003037938368));
#29691=CARTESIAN_POINT('Ctrl Pts',(-0.924658734269251,-3.82450045501019,
23.2944316698708));
#29692=CARTESIAN_POINT('Ctrl Pts',(-1.03667786605961,-3.79567882532997,
23.2885595459048));
#29693=CARTESIAN_POINT('Ctrl Pts',(-1.14735858301995,-3.7619220196557,23.2826874219387));
#29694=CARTESIAN_POINT('Ctrl Pts',(-1.25789580023323,-3.72820898035023,
23.276822911298));
#29695=CARTESIAN_POINT('Ctrl Pts',(-1.36709766168658,-3.68957360894093,
23.2709584006573));
#29696=CARTESIAN_POINT('Ctrl Pts',(-1.47449485356344,-3.64614233496375,
23.2650938900166));
#29697=CARTESIAN_POINT('Ctrl Pts',(-1.58178153479815,-3.60275575133548,
23.259235413899));
#29698=CARTESIAN_POINT('Ctrl Pts',(-1.68726685913955,-3.55458323501818,
23.2533769377813));
#29699=CARTESIAN_POINT('Ctrl Pts',(-1.79049696541762,-3.50180091050738,
23.2475184616637));
#29700=CARTESIAN_POINT('Ctrl Pts',(-1.89779757152842,-3.44693730902381,
23.2414289780725));
#29701=CARTESIAN_POINT('Ctrl Pts',(-2.00266101288997,-3.38709301127182,
23.2353394944812));
#29702=CARTESIAN_POINT('Ctrl Pts',(-2.10460048150773,-3.32252100267815,
23.2292500108899));
#29703=CARTESIAN_POINT('Ctrl Pts',(-2.20255913458384,-3.26047058124646,
23.2233983263695));
#29704=CARTESIAN_POINT('Ctrl Pts',(-2.29781751415447,-3.19405500357113,
23.2175466418491));
#29705=CARTESIAN_POINT('Ctrl Pts',(-2.3899697641798,-3.12354502549689,23.2116949573287));
#29706=CARTESIAN_POINT('Ctrl Pts',(-2.48210795898371,-3.05304580172712,
23.2058441653174));
#29707=CARTESIAN_POINT('Ctrl Pts',(-2.57114063797309,-2.97845367037996,
23.1999933733061));
#29708=CARTESIAN_POINT('Ctrl Pts',(-2.65669301647964,-2.90008124303239,
23.1941425812948));
#29709=CARTESIAN_POINT('Ctrl Pts',(-2.74225306805148,-2.82170178657866,
23.1882912645347));
#29710=CARTESIAN_POINT('Ctrl Pts',(-2.82433189377224,-2.73954163939785,
23.1824399477745));
#29711=CARTESIAN_POINT('Ctrl Pts',(-2.90259026978656,-2.65395153040526,
23.1765886310144));
#29712=CARTESIAN_POINT('Ctrl Pts',(-2.98087461965353,-2.56833301416742,
23.1707353722099));
#29713=CARTESIAN_POINT('Ctrl Pts',(-3.05533571965474,-2.47928257742505,
23.1648821134054));
#29714=CARTESIAN_POINT('Ctrl Pts',(-3.12567393611546,-2.38718483680851,
23.1590288546009));
#29715=CARTESIAN_POINT('Ctrl Pts',(-3.19609217601749,-2.29498231704755,
23.1531689365728));
#29716=CARTESIAN_POINT('Ctrl Pts',(-3.2623779190213,-2.19972590231434,23.1473090185447));
#29717=CARTESIAN_POINT('Ctrl Pts',(-3.3242742158727,-2.10183014006459,23.1414491005165));
#29718=CARTESIAN_POINT('Ctrl Pts',(-3.38621218927206,-2.00386846179664,
23.1355852368379));
#29719=CARTESIAN_POINT('Ctrl Pts',(-3.44375462670587,-1.90326425534581,
23.1297213731593));
#29720=CARTESIAN_POINT('Ctrl Pts',(-3.49669083056497,-1.80045611872183,
23.1238575094807));
#29721=CARTESIAN_POINT('Ctrl Pts',(-3.54970512805217,-1.69749631537825,
23.1179849951933));
#29722=CARTESIAN_POINT('Ctrl Pts',(-3.59809945763546,-1.59232646697015,
23.1121124809059));
#29723=CARTESIAN_POINT('Ctrl Pts',(-3.64171142540951,-1.48540462300406,
23.1062399666185));
#29724=CARTESIAN_POINT('Ctrl Pts',(-3.65376483830642,-1.45585371762645,
23.1046169295701));
#29725=CARTESIAN_POINT('Ctrl Pts',(-3.66545324520294,-1.42616906922076,
23.1029938925218));
#29726=CARTESIAN_POINT('Ctrl Pts',(-3.67677389805233,-1.3963605202816,23.1013708554734));
#29727=CARTESIAN_POINT('Ctrl Pts',(-3.71773185213932,-1.28851363237739,
23.0954987315074));
#29728=CARTESIAN_POINT('Ctrl Pts',(-3.75400941182185,-1.1786823486373,23.0896266075413));
#29729=CARTESIAN_POINT('Ctrl Pts',(-3.78541109864318,-1.06731055193371,
23.0837544835753));
#29730=CARTESIAN_POINT('Ctrl Pts',(-3.81677207255405,-0.956083150975862,
23.0778899729346));
#29731=CARTESIAN_POINT('Ctrl Pts',(-3.84326963395159,-0.843319603191997,
23.0720254622938));
#29732=CARTESIAN_POINT('Ctrl Pts',(-3.86475657327649,-0.729483124764508,
23.0661609516531));
#29733=CARTESIAN_POINT('Ctrl Pts',(-3.88622140275456,-0.615763782940909,
23.0603024755355));
#29734=CARTESIAN_POINT('Ctrl Pts',(-3.90268578923377,-0.500974110244972,
23.0544439994179));
#29735=CARTESIAN_POINT('Ctrl Pts',(-3.9140526883743,-0.385591172914964,
23.0485855233003));
#29736=CARTESIAN_POINT('Ctrl Pts',(-3.92586779940491,-0.265658533525941,
23.042496039709));
#29737=CARTESIAN_POINT('Ctrl Pts',(-3.93217502788284,-0.145085318521391,
23.0364065561177));
#29738=CARTESIAN_POINT('Ctrl Pts',(-3.93292420072768,-0.024417848605377,
23.0303170725265));
#29739=CARTESIAN_POINT('Ctrl Pts',(-3.9336441177902,0.0915374627510185,
23.0244653880061));
#29740=CARTESIAN_POINT('Ctrl Pts',(-3.92923192319479,0.207579353356176,
23.0186137034857));
#29741=CARTESIAN_POINT('Ctrl Pts',(-3.91969613883907,0.323220016660573,
23.0127620189652));
#29742=CARTESIAN_POINT('Ctrl Pts',(-3.91016180889777,0.438843042249969,
23.0069112269539));
#29743=CARTESIAN_POINT('Ctrl Pts',(-3.89550547694663,0.554064550314612,
23.0010604349426));
#29744=CARTESIAN_POINT('Ctrl Pts',(-3.87578767339176,0.668400262406079,
22.9952096429313));
#29745=CARTESIAN_POINT('Ctrl Pts',(-3.85606810137642,0.782746229097468,
22.9893583261711));
#29746=CARTESIAN_POINT('Ctrl Pts',(-3.83128622559715,0.896205834461808,
22.983507009411));
#29747=CARTESIAN_POINT('Ctrl Pts',(-3.80155386518703,1.00830412578823,22.9776556926508));
#29748=CARTESIAN_POINT('Ctrl Pts',(-3.7718116366453,1.1204396223912,22.9718024338463));
#29749=CARTESIAN_POINT('Ctrl Pts',(-3.73711576228698,1.23121250716029,22.9659491750418));
#29750=CARTESIAN_POINT('Ctrl Pts',(-3.69762796824997,1.34016282906801,22.9600959162372));
#29751=CARTESIAN_POINT('Ctrl Pts',(-3.65809524914506,1.44923710321792,22.9542359982091));
#29752=CARTESIAN_POINT('Ctrl Pts',(-3.61375986977994,1.55648428691021,22.948376080181));
#29753=CARTESIAN_POINT('Ctrl Pts',(-3.56483180577043,1.66146417252,22.9425161621529));
#29754=CARTESIAN_POINT('Ctrl Pts',(-3.51587079709513,1.7665147440912,22.9366522984742));
#29755=CARTESIAN_POINT('Ctrl Pts',(-3.46231113681302,1.86929461202232,22.9307884347956));
#29756=CARTESIAN_POINT('Ctrl Pts',(-3.40440802965331,1.96938949109415,22.9249245711169));
#29757=CARTESIAN_POINT('Ctrl Pts',(-3.34641950148917,2.06963203417794,22.9190520568296));
#29758=CARTESIAN_POINT('Ctrl Pts',(-3.28407495980851,2.16718133593129,22.9131795425422));
#29759=CARTESIAN_POINT('Ctrl Pts',(-3.21767207744018,2.26165324531896,22.9073070282548));
#29760=CARTESIAN_POINT('Ctrl Pts',(-3.19931974436393,2.28776325569192,22.9056839912065));
#29761=CARTESIAN_POINT('Ctrl Pts',(-3.18065764414631,2.31363840249603,22.9040609541582));
#29762=CARTESIAN_POINT('Ctrl Pts',(-3.16169257377299,2.33927105504016,22.9024379171099));
#29763=CARTESIAN_POINT('Ctrl Pts',(-3.09307723047334,2.43200961173285,22.8965657931439));
#29764=CARTESIAN_POINT('Ctrl Pts',(-3.02026309303075,2.52188215266147,22.8906936691779));
#29765=CARTESIAN_POINT('Ctrl Pts',(-2.94351803671338,2.60848434297449,22.8848215452118));
#29766=CARTESIAN_POINT('Ctrl Pts',(-2.86687248188534,2.6949742518282,22.8789570345711));
#29767=CARTESIAN_POINT('Ctrl Pts',(-2.78630641495392,2.77820193549154,22.8730925239304));
#29768=CARTESIAN_POINT('Ctrl Pts',(-2.70213006103201,2.85779322787131,22.8672280132897));
#29769=CARTESIAN_POINT('Ctrl Pts',(-2.61804032374078,2.93730262160312,22.8613695371721));
#29770=CARTESIAN_POINT('Ctrl Pts',(-2.53034798725479,3.01318278436915,22.8555110610545));
#29771=CARTESIAN_POINT('Ctrl Pts',(-2.4394020373658,3.08509427734317,22.8496525849369));
#29772=CARTESIAN_POINT('Ctrl Pts',(-2.34486996820258,3.15984133574158,22.8435631013456));
#29773=CARTESIAN_POINT('Ctrl Pts',(-2.24682272007433,3.23029996503633,22.8374736177543));
#29774=CARTESIAN_POINT('Ctrl Pts',(-2.14569287915494,3.29613274434507,22.8313841341631));
#29775=CARTESIAN_POINT('Ctrl Pts',(-2.04851223718589,3.3593947024147,22.8255324496427));
#29776=CARTESIAN_POINT('Ctrl Pts',(-1.9484856189111,3.41838507004249,22.8196807651223));
#29777=CARTESIAN_POINT('Ctrl Pts',(-1.84602808994652,3.4728474327457,22.8138290806019));
#29778=CARTESIAN_POINT('Ctrl Pts',(-1.74358618798242,3.52730148875465,22.8079782885906));
#29779=CARTESIAN_POINT('Ctrl Pts',(-1.63871447747251,3.57722871901678,22.8021274965792));
#29780=CARTESIAN_POINT('Ctrl Pts',(-1.53185315802065,3.62241837758453,22.7962767045679));
#29781=CARTESIAN_POINT('Ctrl Pts',(-1.42498225433632,3.66761208914541,22.7904253878078));
#29782=CARTESIAN_POINT('Ctrl Pts',(-1.31612176776655,3.70806722330985,22.7845740710477));
#29783=CARTESIAN_POINT('Ctrl Pts',(-1.20573176459711,3.74362122975089,22.7787227542876));
#29784=CARTESIAN_POINT('Ctrl Pts',(-1.09530512312952,3.77918703652032,22.7728694954831));
#29785=CARTESIAN_POINT('Ctrl Pts',(-0.983348348942471,3.80984835435136,
22.7670162366785));
#29786=CARTESIAN_POINT('Ctrl Pts',(-0.870335852415045,3.83549273288335,
22.761162977874));
#29787=CARTESIAN_POINT('Ctrl Pts',(-0.757194782129312,3.86116628689795,
22.7553030598459));
#29788=CARTESIAN_POINT('Ctrl Pts',(-0.642995995563085,3.88181141756271,
22.7494431418178));
#29789=CARTESIAN_POINT('Ctrl Pts',(-0.528223361666999,3.89736694194801,
22.7435832237896));
#29790=CARTESIAN_POINT('Ctrl Pts',(-0.413373448071697,3.91293294031309,
22.737719360111));
#29791=CARTESIAN_POINT('Ctrl Pts',(-0.297949328490464,3.92340247136172,
22.7318554964324));
#29792=CARTESIAN_POINT('Ctrl Pts',(-0.182437499126775,3.92876641694468,
22.7259916327537));
#29793=CARTESIAN_POINT('Ctrl Pts',(-0.0667552620427459,3.93413827563701,
22.7201191184664));
#29794=CARTESIAN_POINT('Ctrl Pts',(0.0490145312043054,3.93438951556414,
22.714246604179));
#29795=CARTESIAN_POINT('Ctrl Pts',(0.164387793031867,3.92956303594969,22.7083740898916));
#29796=CARTESIAN_POINT('Ctrl Pts',(0.196274489116512,3.92822910045903,22.7067510528432));
#29797=CARTESIAN_POINT('Ctrl Pts',(0.228130943146691,3.92650760594574,22.7051280157949));
#29798=CARTESIAN_POINT('Ctrl Pts',(0.259947061604018,3.92440014845115,22.7035049787465));
#29799=CARTESIAN_POINT('Ctrl Pts',(0.375057306246639,3.91677539849614,22.6976328547805));
#29800=CARTESIAN_POINT('Ctrl Pts',(0.490024774287151,3.90406896245712,22.6917607308145));
#29801=CARTESIAN_POINT('Ctrl Pts',(0.604364495680487,3.88628776036475,22.6858886068485));
#29802=CARTESIAN_POINT('Ctrl Pts',(0.718555973355043,3.86852961195391,22.6800240962077));
#29803=CARTESIAN_POINT('Ctrl Pts',(0.832120918179618,3.84570984473741,22.674159585567));
#29804=CARTESIAN_POINT('Ctrl Pts',(0.944576861721214,3.81788731529637,22.6682950749263));
#29805=CARTESIAN_POINT('Ctrl Pts',(1.05691708921537,3.7900934149614,22.6624365988087));
#29806=CARTESIAN_POINT('Ctrl Pts',(1.16815018633433,3.75730709029619,22.6565781226911));
#29807=CARTESIAN_POINT('Ctrl Pts',(1.27780196137464,3.71963857753776,22.6507196465735));
#29808=CARTESIAN_POINT('Ctrl Pts',(1.39177745115346,3.68048474542421,22.6446301629822));
#29809=CARTESIAN_POINT('Ctrl Pts',(1.50404389635716,3.63605585179692,22.638540679391));
#29810=CARTESIAN_POINT('Ctrl Pts',(1.61408362998758,3.58653356814154,22.6324511957997));
#29811=CARTESIAN_POINT('Ctrl Pts',(1.71982622642691,3.5389451681831,22.6265995112793));
#29812=CARTESIAN_POINT('Ctrl Pts',(1.82351234490465,3.4866539005432,22.6207478267589));
#29813=CARTESIAN_POINT('Ctrl Pts',(1.92470194778825,3.42987046580189,22.6148961422385));
#29814=CARTESIAN_POINT('Ctrl Pts',(2.02587611705769,3.37309569176878,22.6090453502272));
#29815=CARTESIAN_POINT('Ctrl Pts',(2.12455416740145,3.31183031519032,22.6031945582158));
#29816=CARTESIAN_POINT('Ctrl Pts',(2.22032090750863,3.24633086232443,22.5973437662045));
#29817=CARTESIAN_POINT('Ctrl Pts',(2.31609623679193,3.18082553491027,22.5914924494444));
#29818=CARTESIAN_POINT('Ctrl Pts',(2.40895939551932,3.11108560970491,22.5856411326843));
#29819=CARTESIAN_POINT('Ctrl Pts',(2.49852501127375,3.0374103720175,22.5797898159242));
#29820=CARTESIAN_POINT('Ctrl Pts',(2.58812035373882,2.96371068161514,22.5739365571197));
#29821=CARTESIAN_POINT('Ctrl Pts',(2.67441565788307,2.88607334407693,22.5680832983152));
#29822=CARTESIAN_POINT('Ctrl Pts',(2.75705995669766,2.80483678583519,22.5622300395107));
#29823=CARTESIAN_POINT('Ctrl Pts',(2.83979827952272,2.72350780516248,22.5563701214825));
#29824=CARTESIAN_POINT('Ctrl Pts',(2.91887701127858,2.6385717206208,22.5505102034544));
#29825=CARTESIAN_POINT('Ctrl Pts',(2.99398321259888,2.55040261972028,22.5446502854263));
#29826=CARTESIAN_POINT('Ctrl Pts',(3.06913998507393,2.46217415204089,22.5387864217476));
#29827=CARTESIAN_POINT('Ctrl Pts',(3.14031864774902,2.37070865886867,22.532922558069));
#29828=CARTESIAN_POINT('Ctrl Pts',(3.20724865111092,2.27641057148028,22.5270586943904));
#29829=CARTESIAN_POINT('Ctrl Pts',(3.27427739231955,2.18197337174121,22.521186180103));
#29830=CARTESIAN_POINT('Ctrl Pts',(3.33704474156023,2.08469558383841,22.5153136658156));
#29831=CARTESIAN_POINT('Ctrl Pts',(3.3953252204052,1.98500771980373,22.5094411515282));
#29832=CARTESIAN_POINT('Ctrl Pts',(3.41143269528444,1.95745613138978,22.5078181144798));
#29833=CARTESIAN_POINT('Ctrl Pts',(3.42719772057107,1.92972057326528,22.5061950774315));
#29834=CARTESIAN_POINT('Ctrl Pts',(3.44261618523119,1.90181040095595,22.5045720403831));
#29835=CARTESIAN_POINT('Ctrl Pts',(3.50115409939407,1.7958463308018,22.4984099999001));
#29836=CARTESIAN_POINT('Ctrl Pts',(3.55487319665964,1.6870374951563,22.4922479594172));
#29837=CARTESIAN_POINT('Ctrl Pts',(3.60350142191582,1.57583834902272,22.4860859189342));
#29838=CARTESIAN_POINT('Ctrl Pts',(3.65204246483522,1.4648385645018,22.4799349259671));
#29839=CARTESIAN_POINT('Ctrl Pts',(3.69551067384141,1.35145732804514,22.473783933));
#29840=CARTESIAN_POINT('Ctrl Pts',(3.73367945692755,1.23617422433782,22.4676329400329));
#29841=CARTESIAN_POINT('Ctrl Pts',(3.77176063720777,1.1211557118106,22.4614960644727));
#29842=CARTESIAN_POINT('Ctrl Pts',(3.80456652708893,1.00424436862022,22.4553591889125));
#29843=CARTESIAN_POINT('Ctrl Pts',(3.83191863633248,0.885939368426433,22.4492223133524));
#29844=CARTESIAN_POINT('Ctrl Pts',(3.85923289212364,0.767798094278509,22.4430939308091));
#29845=CARTESIAN_POINT('Ctrl Pts',(3.88110831736986,0.64826734729674,22.4369655482658));
#29846=CARTESIAN_POINT('Ctrl Pts',(3.89741586819658,0.527862245599663,22.4308371657226));
#29847=CARTESIAN_POINT('Ctrl Pts',(3.913695364911,0.407664278516497,22.4247193259233));
#29848=CARTESIAN_POINT('Ctrl Pts',(3.92442603206477,0.286595304961994,22.4186014861239));
#29849=CARTESIAN_POINT('Ctrl Pts',(3.92952978485551,0.165180719012368,22.4124836463246));
#29850=CARTESIAN_POINT('Ctrl Pts',(3.93184344779074,0.11014035188924,22.4097102715614));
#29851=CARTESIAN_POINT('Ctrl Pts',(3.93300144940657,0.0550291046220322,
22.4069368967982));
#29852=CARTESIAN_POINT('Ctrl Pts',(3.93299999863833,-0.000103493608108607,
22.404163522035));
#29853=CARTESIAN_POINT('',(3.93299837124471,-0.00357935559718133,21.154163522035));
#29854=CARTESIAN_POINT('Ctrl Pts',(3.9329999986383,-0.000103494422981112,
22.404163521994));
#29855=CARTESIAN_POINT('Ctrl Pts',(3.9329967860024,-0.122190237360205,22.3980221047082));
#29856=CARTESIAN_POINT('Ctrl Pts',(3.92730461696609,-0.244162252495147,
22.3918806874223));
#29857=CARTESIAN_POINT('Ctrl Pts',(3.91598119473771,-0.365486364260817,
22.3857392701364));
#29858=CARTESIAN_POINT('Ctrl Pts',(3.90464111657057,-0.486988935059093,
22.379588819268));
#29859=CARTESIAN_POINT('Ctrl Pts',(3.88765329229108,-0.607841353962135,
22.3734383683995));
#29860=CARTESIAN_POINT('Ctrl Pts',(3.86512675196899,-0.727519203329828,
22.367287917531));
#29861=CARTESIAN_POINT('Ctrl Pts',(3.84254403578185,-0.847495500955385,
22.3611221288924));
#29862=CARTESIAN_POINT('Ctrl Pts',(3.81439505748278,-0.966291029651327,
22.3549563402538));
#29863=CARTESIAN_POINT('Ctrl Pts',(3.78083947401601,-1.08339368270371,22.3487905516151));
#29864=CARTESIAN_POINT('Ctrl Pts',(3.74723768458369,-1.20065758585503,22.342616272699));
#29865=CARTESIAN_POINT('Ctrl Pts',(3.70821454621656,-1.31622363179537,22.3364419937828));
#29866=CARTESIAN_POINT('Ctrl Pts',(3.663978222529,-1.42959874959138,22.3302677148666));
#29867=CARTESIAN_POINT('Ctrl Pts',(3.61964185622934,-1.54323027076782,22.3240794725163));
#29868=CARTESIAN_POINT('Ctrl Pts',(3.57006888036979,-1.65466064076861,22.317891230166));
#29869=CARTESIAN_POINT('Ctrl Pts',(3.51551436855138,-1.76341932747399,22.3117029878157));
#29870=CARTESIAN_POINT('Ctrl Pts',(3.49769496682149,-1.79894369870233,22.3096816925504));
#29871=CARTESIAN_POINT('Ctrl Pts',(3.4793444322737,-1.83418325163946,22.307660397285));
#29872=CARTESIAN_POINT('Ctrl Pts',(3.46047264866889,-1.86912226668416,22.3056391020197));
#29873=CARTESIAN_POINT('Ctrl Pts',(3.40564767841961,-1.97062462069992,22.2997669780537));
#29874=CARTESIAN_POINT('Ctrl Pts',(3.3462611177917,-2.06988291325659,22.2938948540876));
#29875=CARTESIAN_POINT('Ctrl Pts',(3.28252103059589,-2.16645901962065,22.2880227301216));
#29876=CARTESIAN_POINT('Ctrl Pts',(3.21886358368866,-2.26290991314534,22.2821582194809));
#29877=CARTESIAN_POINT('Ctrl Pts',(3.15086406056402,-2.35668519412931,22.2762937088402));
#29878=CARTESIAN_POINT('Ctrl Pts',(3.07877671234546,-2.44737062079271,22.2704291981994));
#29879=CARTESIAN_POINT('Ctrl Pts',(3.00676354129109,-2.5379627330542,22.2645707220818));
#29880=CARTESIAN_POINT('Ctrl Pts',(2.93067116743926,-2.62547099335779,22.2587122459642));
#29881=CARTESIAN_POINT('Ctrl Pts',(2.85079712008861,-2.70951006274095,22.2528537698466));
#29882=CARTESIAN_POINT('Ctrl Pts',(2.76777353324704,-2.79686290395091,22.2467642862553));
#29883=CARTESIAN_POINT('Ctrl Pts',(2.68066415523773,-2.88046695630752,22.2406748026641));
#29884=CARTESIAN_POINT('Ctrl Pts',(2.58984956229429,-2.95992706746029,22.2345853190728));
#29885=CARTESIAN_POINT('Ctrl Pts',(2.50258134984423,-3.03628419946554,22.2287336345524));
#29886=CARTESIAN_POINT('Ctrl Pts',(2.41189221550572,-3.10881466719643,22.222881950032));
#29887=CARTESIAN_POINT('Ctrl Pts',(2.31815683530451,-3.17720598748822,22.2170302655116));
#29888=CARTESIAN_POINT('Ctrl Pts',(2.22443575178628,-3.24558687661706,22.2111794735003));
#29889=CARTESIAN_POINT('Ctrl Pts',(2.12766968008904,-3.30982962994567,22.205328681489));
#29890=CARTESIAN_POINT('Ctrl Pts',(2.02826463018973,-3.3696634238335,22.1994778894777));
#29891=CARTESIAN_POINT('Ctrl Pts',(1.92885066479962,-3.42950258412515,22.1936265727175));
#29892=CARTESIAN_POINT('Ctrl Pts',(1.82679760491666,-3.48493178568025,22.1877752559574));
#29893=CARTESIAN_POINT('Ctrl Pts',(1.72253793702354,-3.53572511028709,22.1819239391972));
#29894=CARTESIAN_POINT('Ctrl Pts',(1.61824366548264,-3.58653529313212,22.1760706803927));
#29895=CARTESIAN_POINT('Ctrl Pts',(1.51174170111808,-3.63270635857377,22.1702174215882));
#29896=CARTESIAN_POINT('Ctrl Pts',(1.40348580876995,-3.67405995930678,22.1643641627836));
#29897=CARTESIAN_POINT('Ctrl Pts',(1.29510675422864,-3.71546060782677,22.1585042447555));
#29898=CARTESIAN_POINT('Ctrl Pts',(1.18497017529292,-3.75203270448121,22.1526443267274));
#29899=CARTESIAN_POINT('Ctrl Pts',(1.07354644358195,-3.7836473188542,22.1467844086993));
#29900=CARTESIAN_POINT('Ctrl Pts',(0.962047687083573,-3.81528322025182,
22.1409205450206));
#29901=CARTESIAN_POINT('Ctrl Pts',(0.849260453421637,-3.8419548978208,22.135056681342));
#29902=CARTESIAN_POINT('Ctrl Pts',(0.735665070846138,-3.86358459251728,
22.1291928176634));
#29903=CARTESIAN_POINT('Ctrl Pts',(0.621902107769854,-3.88524619621383,
22.123320303376));
#29904=CARTESIAN_POINT('Ctrl Pts',(0.507329023948782,-3.9018509128245,22.1174477890886));
#29905=CARTESIAN_POINT('Ctrl Pts',(0.392431112203861,-3.91337281921547,
22.1115752748012));
#29906=CARTESIAN_POINT('Ctrl Pts',(0.360675792691475,-3.91655722712403,
22.1099522377529));
#29907=CARTESIAN_POINT('Ctrl Pts',(0.328895657420771,-3.91935369076338,
22.1083292007045));
#29908=CARTESIAN_POINT('Ctrl Pts',(0.297100924157665,-3.92176236415016,
22.1067061636562));
#29909=CARTESIAN_POINT('Ctrl Pts',(0.18206805082896,-3.93047690873524,22.1008340396902));
#29910=CARTESIAN_POINT('Ctrl Pts',(0.0664585796198982,-3.93414056691307,
22.0949619157242));
#29911=CARTESIAN_POINT('Ctrl Pts',(-0.0492464061903585,-3.93269167256694,
22.0890897917581));
#29912=CARTESIAN_POINT('Ctrl Pts',(-0.164801378189099,-3.93124465674109,
22.0832252811174));
#29913=CARTESIAN_POINT('Ctrl Pts',(-0.280451208963663,-3.9246982752529,
22.0773607704767));
#29914=CARTESIAN_POINT('Ctrl Pts',(-0.395709954140918,-3.91304263102177,
22.071496259836));
#29915=CARTESIAN_POINT('Ctrl Pts',(-0.510850099215983,-3.90139898033261,
22.0656377837184));
#29916=CARTESIAN_POINT('Ctrl Pts',(-0.625599550294319,-3.88465656542435,
22.0597793076008));
#29917=CARTESIAN_POINT('Ctrl Pts',(-0.739473297777974,-3.86285752285447,
22.0539208314832));
#29918=CARTESIAN_POINT('Ctrl Pts',(-0.857837237966087,-3.84019891516028,
22.0478313478919));
#29919=CARTESIAN_POINT('Ctrl Pts',(-0.975254538460975,-3.81207670237197,
22.0417418643006));
#29920=CARTESIAN_POINT('Ctrl Pts',(-1.09118705804657,-3.77859759756866,
22.0356523807094));
#29921=CARTESIAN_POINT('Ctrl Pts',(-1.20259232256574,-3.74642587784921,
22.029800696189));
#29922=CARTESIAN_POINT('Ctrl Pts',(-1.31262615914762,-3.70930792204073,
22.0239490116686));
#29923=CARTESIAN_POINT('Ctrl Pts',(-1.4208231760497,-3.66739014864795,22.0180973271482));
#29924=CARTESIAN_POINT('Ctrl Pts',(-1.52900369055487,-3.62547876862677,
22.0122465351369));
#29925=CARTESIAN_POINT('Ctrl Pts',(-1.63534755702896,-3.5787691759257,22.0063957431256));
#29926=CARTESIAN_POINT('Ctrl Pts',(-1.73940750656553,-3.5274566653757,22.0005449511142));
#29927=CARTESIAN_POINT('Ctrl Pts',(-1.84347678908387,-3.47613955268312,
21.9946936343541));
#29928=CARTESIAN_POINT('Ctrl Pts',(-1.94526137665291,-3.4202188843225,21.988842317594));
#29929=CARTESIAN_POINT('Ctrl Pts',(-2.04433747915184,-3.35993649811051,
21.9829910008339));
#29930=CARTESIAN_POINT('Ctrl Pts',(-2.14344646487984,-3.29963410425324,
21.9771377420293));
#29931=CARTESIAN_POINT('Ctrl Pts',(-2.23984482505981,-3.23496732876461,
21.9712844832248));
#29932=CARTESIAN_POINT('Ctrl Pts',(-2.33313730000854,-3.16622161879248,
21.9654312244203));
#29933=CARTESIAN_POINT('Ctrl Pts',(-2.42653591334463,-3.0973976971661,21.9595713063922));
#29934=CARTESIAN_POINT('Ctrl Pts',(-2.51682125556449,-3.02448582396564,
21.9537113883641));
#29935=CARTESIAN_POINT('Ctrl Pts',(-2.60363067498649,-2.94781212228144,
21.9478514703359));
#29936=CARTESIAN_POINT('Ctrl Pts',(-2.69049854567493,-2.87108679399961,
21.9419876066573));
#29937=CARTESIAN_POINT('Ctrl Pts',(-2.77388553657606,-2.7905948800586,21.9361237429787));
#29938=CARTESIAN_POINT('Ctrl Pts',(-2.85346667369742,-2.70669853180922,
21.9302598793001));
#29939=CARTESIAN_POINT('Ctrl Pts',(-2.9331652121296,-2.62267841627511,21.9243873650127));
#29940=CARTESIAN_POINT('Ctrl Pts',(-3.00904642122821,-2.53524415379346,
21.9185148507253));
#29941=CARTESIAN_POINT('Ctrl Pts',(-3.08082626130832,-2.44479008252917,
21.9126423364379));
#29942=CARTESIAN_POINT('Ctrl Pts',(-3.10066467022034,-2.4197905164742,21.9110192993895));
#29943=CARTESIAN_POINT('Ctrl Pts',(-3.12019005574155,-2.3945604445957,21.9093962623412));
#29944=CARTESIAN_POINT('Ctrl Pts',(-3.13939702632131,-2.3691085477717,21.9077732252928));
#29945=CARTESIAN_POINT('Ctrl Pts',(-3.20888756097712,-2.27702396259676,
21.9019011013268));
#29946=CARTESIAN_POINT('Ctrl Pts',(-3.27443963197061,-2.18172496883002,
21.8960289773608));
#29947=CARTESIAN_POINT('Ctrl Pts',(-3.33574139859285,-2.08358304891209,
21.8901568533947));
#29948=CARTESIAN_POINT('Ctrl Pts',(-3.39696368625746,-1.98556837194203,
21.884292342754));
#29949=CARTESIAN_POINT('Ctrl Pts',(-3.45394641115383,-1.88471844615048,
21.8784278321133));
#29950=CARTESIAN_POINT('Ctrl Pts',(-3.50641866652358,-1.78143681758715,
21.8725633214726));
#29951=CARTESIAN_POINT('Ctrl Pts',(-3.55883692846457,-1.6782614647921,21.866704845355));
#29952=CARTESIAN_POINT('Ctrl Pts',(-3.60675376637638,-1.57265975256975,
21.8608463692374));
#29953=CARTESIAN_POINT('Ctrl Pts',(-3.64994256188307,-1.46506255666932,
21.8549878931197));
#29954=CARTESIAN_POINT('Ctrl Pts',(-3.69483434880596,-1.35322266080759,
21.8488984095285));
#29955=CARTESIAN_POINT('Ctrl Pts',(-3.73461731533458,-1.23922706053372,
21.8428089259372));
#29956=CARTESIAN_POINT('Ctrl Pts',(-3.76909047092907,-1.12358623253923,
21.8367194423459));
#29957=CARTESIAN_POINT('Ctrl Pts',(-3.80221742298311,-1.01246126882759,
21.8308677578255));
#29958=CARTESIAN_POINT('Ctrl Pts',(-3.83044135719184,-0.899817594464047,
21.8250160733051));
#29959=CARTESIAN_POINT('Ctrl Pts',(-3.85363400283394,-0.786125926427865,
21.8191643887847));
#29960=CARTESIAN_POINT('Ctrl Pts',(-3.87682311109344,-0.672451598842391,
21.8133135967734));
#29961=CARTESIAN_POINT('Ctrl Pts',(-3.89498237396998,-0.557730000358334,
21.8074628047621));
#29962=CARTESIAN_POINT('Ctrl Pts',(-3.90803443996023,-0.442443008855035,
21.8016120127508));
#29963=CARTESIAN_POINT('Ctrl Pts',(-3.92108767657085,-0.327145677433238,
21.7957606959906));
#29964=CARTESIAN_POINT('Ctrl Pts',(-3.92903275921059,-0.211283262999728,
21.7899093792305));
#29965=CARTESIAN_POINT('Ctrl Pts',(-3.93184418629909,-0.0953430367987633,
21.7840580624704));
#29966=CARTESIAN_POINT('Ctrl Pts',(-3.93465654649658,0.0206356698118804,
21.7782048036658));
#29967=CARTESIAN_POINT('Ctrl Pts',(-3.93233185312455,0.136691826469843,
21.7723515448613));
#29968=CARTESIAN_POINT('Ctrl Pts',(-3.92489671567469,0.252338604430756,
21.7664982860568));
#29969=CARTESIAN_POINT('Ctrl Pts',(-3.91745311930571,0.368116953159008,
21.7606383680287));
#29970=CARTESIAN_POINT('Ctrl Pts',(-3.90488750055562,0.483484580762219,
21.7547784500005));
#29971=CARTESIAN_POINT('Ctrl Pts',(-3.88727831501467,0.59796011707865,21.7489185319724));
#29972=CARTESIAN_POINT('Ctrl Pts',(-3.86965727270514,0.712512733049828,
21.7430546682938));
#29973=CARTESIAN_POINT('Ctrl Pts',(-3.84698598222039,0.826171657244995,
21.7371908046151));
#29974=CARTESIAN_POINT('Ctrl Pts',(-3.8193935738895,0.938467755296662,21.7313269409365));
#29975=CARTESIAN_POINT('Ctrl Pts',(-3.79176046012235,1.05092951709206,21.7254544266491));
#29976=CARTESIAN_POINT('Ctrl Pts',(-3.75919185509884,1.16202404493571,21.7195819123617));
#29977=CARTESIAN_POINT('Ctrl Pts',(-3.7218660912396,1.27129925622602,21.7137093980743));
#29978=CARTESIAN_POINT('Ctrl Pts',(-3.71155005033509,1.30150058187796,21.712086361026));
#29979=CARTESIAN_POINT('Ctrl Pts',(-3.70087091071236,1.33156306985958,21.7104633239777));
#29980=CARTESIAN_POINT('Ctrl Pts',(-3.68983306351299,1.36147749280197,21.7088402869293));
#29981=CARTESIAN_POINT('Ctrl Pts',(-3.64989829607244,1.46970743128049,21.7029681629633));
#29982=CARTESIAN_POINT('Ctrl Pts',(-3.60513065091982,1.57636028015001,21.6970960389973));
#29983=CARTESIAN_POINT('Ctrl Pts',(-3.55567420649336,1.68097291390368,21.6912239150312));
#29984=CARTESIAN_POINT('Ctrl Pts',(-3.50628188332908,1.78544991530054,21.6853594043905));
#29985=CARTESIAN_POINT('Ctrl Pts',(-3.45221302511802,1.88789159158776,21.6794948937498));
#29986=CARTESIAN_POINT('Ctrl Pts',(-3.39366080852721,1.98785193529762,21.6736303831091));
#29987=CARTESIAN_POINT('Ctrl Pts',(-3.33516884158474,2.08770942080828,21.6677719069915));
#29988=CARTESIAN_POINT('Ctrl Pts',(-3.27220290009002,2.18509029773725,21.6619134308738));
#29989=CARTESIAN_POINT('Ctrl Pts',(-3.20500308818911,2.27957105717244,21.6560549547562));
#29990=CARTESIAN_POINT('Ctrl Pts',(-3.1351534986898,2.37777731810457,21.649965471165));
#29991=CARTESIAN_POINT('Ctrl Pts',(-3.06072946983559,2.47284963393164,21.6438759875737));
#29992=CARTESIAN_POINT('Ctrl Pts',(-2.98205193327693,2.56434304788562,21.6377865039824));
#29993=CARTESIAN_POINT('Ctrl Pts',(-2.90644681571913,2.6522635728578,21.631934819462));
#29994=CARTESIAN_POINT('Ctrl Pts',(-2.82691445693249,2.73687912546003,21.6260831349416));
#29995=CARTESIAN_POINT('Ctrl Pts',(-2.74378162707226,2.81782742249072,21.6202314504212));
#29996=CARTESIAN_POINT('Ctrl Pts',(-2.66066147677571,2.89876337314649,21.6143806584099));
#29997=CARTESIAN_POINT('Ctrl Pts',(-2.57394224339891,2.97603289203649,21.6085298663986));
#29998=CARTESIAN_POINT('Ctrl Pts',(-2.48398760242921,3.04931051075124,21.6026790743873));
#29999=CARTESIAN_POINT('Ctrl Pts',(-2.39402489356179,3.12259470162643,21.5968277576272));
#30000=CARTESIAN_POINT('Ctrl Pts',(-2.30082652079628,3.19188601948351,21.590976440867));
#30001=CARTESIAN_POINT('Ctrl Pts',(-2.20478871481115,3.25689971031369,21.5851251241069));
#30002=CARTESIAN_POINT('Ctrl Pts',(-2.10871903400364,3.32193497910295,21.5792718653024));
#30003=CARTESIAN_POINT('Ctrl Pts',(-2.00980838823148,3.38268956617601,21.5734186064979));
#30004=CARTESIAN_POINT('Ctrl Pts',(-1.90848079393494,3.43892280506287,21.5675653476933));
#30005=CARTESIAN_POINT('Ctrl Pts',(-1.80703791973546,3.49522002022753,21.5617054296652));
#30006=CARTESIAN_POINT('Ctrl Pts',(-1.70317297027669,3.54698541935955,21.5558455116371));
#30007=CARTESIAN_POINT('Ctrl Pts',(-1.59733338384113,3.59402491099695,21.549985593609));
#30008=CARTESIAN_POINT('Ctrl Pts',(-1.49142253258304,3.64109607567028,21.5441217299304));
#30009=CARTESIAN_POINT('Ctrl Pts',(-1.38353478079582,3.68343484603208,21.5382578662517));
#30010=CARTESIAN_POINT('Ctrl Pts',(-1.27413465303335,3.72089638204823,21.5323940025731));
#30011=CARTESIAN_POINT('Ctrl Pts',(-1.16457313377961,3.75841318283679,21.5265214882857));
#30012=CARTESIAN_POINT('Ctrl Pts',(-1.05349518082514,3.79103827314213,21.5206489739983));
#30013=CARTESIAN_POINT('Ctrl Pts',(-0.941377556893697,3.81867742751032,
21.5147764597109));
#30014=CARTESIAN_POINT('Ctrl Pts',(-0.910390649326295,3.82631629722248,
21.5131534226626));
#30015=CARTESIAN_POINT('Ctrl Pts',(-0.879324366010399,3.83357461986997,
21.5115303856142));
#30016=CARTESIAN_POINT('Ctrl Pts',(-0.848188843983448,3.84045110435506,
21.5099073485659));
#30017=CARTESIAN_POINT('Ctrl Pts',(-0.735540987129409,3.86533012322185,
21.5040352245999));
#30018=CARTESIAN_POINT('Ctrl Pts',(-0.621608724895704,3.88529037990338,
21.4981631006338));
#30019=CARTESIAN_POINT('Ctrl Pts',(-0.506859602906506,3.9002028592038,21.4922909766678));
#30020=CARTESIAN_POINT('Ctrl Pts',(-0.392259255432419,3.9150960041787,21.4864264660271));
#30021=CARTESIAN_POINT('Ctrl Pts',(-0.276844560494443,3.92495433370975,
21.4805619553864));
#30022=CARTESIAN_POINT('Ctrl Pts',(-0.161095189999589,3.92969939559745,
21.4746974447457));
#30023=CARTESIAN_POINT('Ctrl Pts',(-0.0454649244554603,3.93443957486369,
21.4688389686281));
#30024=CARTESIAN_POINT('Ctrl Pts',(0.0704989210831195,3.93407693503178,
21.4629804925105));
#30025=CARTESIAN_POINT('Ctrl Pts',(0.186310248777662,3.92858466768891,21.4571220163929));
#30026=CARTESIAN_POINT('Ctrl Pts',(0.306688170530945,3.92287583296946,21.4510325328016));
#30027=CARTESIAN_POINT('Ctrl Pts',(0.426900847770564,3.91162445356513,21.4449430492103));
#30028=CARTESIAN_POINT('Ctrl Pts',(0.546400460576367,3.89486014340463,21.438853565619));
#30029=CARTESIAN_POINT('Ctrl Pts',(0.661233520550923,3.8787504925958,21.4330018810986));
#30030=CARTESIAN_POINT('Ctrl Pts',(0.775407714478856,3.85755046247219,21.4271501965782));
#30031=CARTESIAN_POINT('Ctrl Pts',(0.888441632612912,3.83133925219891,21.4212985120578));
#30032=CARTESIAN_POINT('Ctrl Pts',(1.00145831061734,3.80513203970497,21.4154477200465));
#30033=CARTESIAN_POINT('Ctrl Pts',(1.11333465601346,3.77391526011858,21.4095969280352));
#30034=CARTESIAN_POINT('Ctrl Pts',(1.22360029484686,3.73781905908388,21.4037461360239));
#30035=CARTESIAN_POINT('Ctrl Pts',(1.33387582324108,3.7017196206347,21.3978948192638));
#30036=CARTESIAN_POINT('Ctrl Pts',(1.44253996497586,3.66074001939788,21.3920435025036));
#30037=CARTESIAN_POINT('Ctrl Pts',(1.54913901377223,3.61505979425082,21.3861921857435));
#30038=CARTESIAN_POINT('Ctrl Pts',(1.65577344265372,3.56936440789667,21.380338926939));
#30039=CARTESIAN_POINT('Ctrl Pts',(1.76034103592844,3.51896545816352,21.3744856681345));
#30040=CARTESIAN_POINT('Ctrl Pts',(1.86241017044259,3.46408968663226,21.3686324093299));
#30041=CARTESIAN_POINT('Ctrl Pts',(1.96459542850639,3.40915148320706,21.3627724913018));
#30042=CARTESIAN_POINT('Ctrl Pts',(2.06427618994552,3.34972648785753,21.3569125732737));
#30043=CARTESIAN_POINT('Ctrl Pts',(2.16104736582602,3.28608631698202,21.3510526552456));
#30044=CARTESIAN_POINT('Ctrl Pts',(2.25788370050872,3.22240329535813,21.3451887915669));
#30045=CARTESIAN_POINT('Ctrl Pts',(2.35180621445919,3.15449968842387,21.3393249278883));
#30046=CARTESIAN_POINT('Ctrl Pts',(2.44244202842624,3.08268810257819,21.3334610642097));
#30047=CARTESIAN_POINT('Ctrl Pts',(2.53321155201019,3.01077057737794,21.3275885499223));
#30048=CARTESIAN_POINT('Ctrl Pts',(2.62068438736605,2.93493383677828,21.3217160356349));
#30049=CARTESIAN_POINT('Ctrl Pts',(2.70452363159946,2.85552813435975,21.3158435213475));
#30050=CARTESIAN_POINT('Ctrl Pts',(2.7276950012782,2.83358210058806,21.3142204842991));
#30051=CARTESIAN_POINT('Ctrl Pts',(2.7505890532504,2.81136364899845,21.3125974472508));
#30052=CARTESIAN_POINT('Ctrl Pts',(2.77319922360723,2.78888061167635,21.3109744102024));
#30053=CARTESIAN_POINT('Ctrl Pts',(2.85386063832436,2.70867274199126,21.305184251951));
#30054=CARTESIAN_POINT('Ctrl Pts',(2.93119302544246,2.62480957187567,21.2993940936995));
#30055=CARTESIAN_POINT('Ctrl Pts',(3.00483960642236,2.53760279391309,21.293603935448));
#30056=CARTESIAN_POINT('Ctrl Pts',(3.07873877903787,2.45009691581051,21.2877939182225));
#30057=CARTESIAN_POINT('Ctrl Pts',(3.1489264602448,2.35922470143109,21.281983900997));
#30058=CARTESIAN_POINT('Ctrl Pts',(3.21507690142854,2.26534092752077,21.2761738837714));
#30059=CARTESIAN_POINT('Ctrl Pts',(3.28083667184213,2.17201161168513,21.2703981793012));
#30060=CARTESIAN_POINT('Ctrl Pts',(3.34260648871566,2.07570654588649,21.264622474831));
#30061=CARTESIAN_POINT('Ctrl Pts',(3.40010512745083,1.97680907582968,21.2588467703608));
#30062=CARTESIAN_POINT('Ctrl Pts',(3.45756656704702,1.87797558816991,21.2530748025222));
#30063=CARTESIAN_POINT('Ctrl Pts',(3.51076210601668,1.77655339587996,21.2473028346837));
#30064=CARTESIAN_POINT('Ctrl Pts',(3.55945375553484,1.67295485958495,21.2415308668451));
#30065=CARTESIAN_POINT('Ctrl Pts',(3.60812647113049,1.56939660795228,21.235761143457));
#30066=CARTESIAN_POINT('Ctrl Pts',(3.65229859812937,1.4636640797495,21.2299914200688));
#30067=CARTESIAN_POINT('Ctrl Pts',(3.69177846402697,1.35619348639738,21.2242216966807));
#30068=CARTESIAN_POINT('Ctrl Pts',(3.73172675897349,1.24744775325724,21.2183835154602));
#30069=CARTESIAN_POINT('Ctrl Pts',(3.76687052644689,1.13692284275504,21.2125453342397));
#30070=CARTESIAN_POINT('Ctrl Pts',(3.79706196232525,1.02508997374023,21.2067071530192));
#30071=CARTESIAN_POINT('Ctrl Pts',(3.82690916046214,0.914532204538681,21.2009355377722));
#30072=CARTESIAN_POINT('Ctrl Pts',(3.85191631229563,0.802696579324076,21.1951639225251));
#30073=CARTESIAN_POINT('Ctrl Pts',(3.87199158259496,0.690050856324234,21.189392307278));
#30074=CARTESIAN_POINT('Ctrl Pts',(3.89241415512724,0.575456361997903,21.1835208430708));
#30075=CARTESIAN_POINT('Ctrl Pts',(3.90773252666534,0.460023929919707,21.1776493788637));
#30076=CARTESIAN_POINT('Ctrl Pts',(3.9179049576323,0.344252440746937,21.1717779146565));
#30077=CARTESIAN_POINT('Ctrl Pts',(3.92807738859927,0.228480951574167,21.1659064504493));
#30078=CARTESIAN_POINT('Ctrl Pts',(3.93310389559052,0.11237086755328,21.1600349862422));
#30079=CARTESIAN_POINT('Ctrl Pts',(3.93299837124471,-0.00357935559718133,
21.154163522035));
#30080=CARTESIAN_POINT('',(3.93453862278255,0.00168715760829792,19.904163522035));
#30081=CARTESIAN_POINT('Ctrl Pts',(3.93385572002521,-0.00358013585587236,
21.154163522035));
#30082=CARTESIAN_POINT('Ctrl Pts',(3.9364368881255,-0.280919883983378,21.1401228386363));
#30083=CARTESIAN_POINT('Ctrl Pts',(3.78295630631491,-1.86523628308173,21.0597711757834));
#30084=CARTESIAN_POINT('Ctrl Pts',(1.63507764328188,-4.35555465900237,20.9131085334754));
#30085=CARTESIAN_POINT('Ctrl Pts',(-2.78143531328603,-3.72933678891077,
20.7141755951122));
#30086=CARTESIAN_POINT('Ctrl Pts',(-4.64096218155626,0.325277291681748,
20.5152426567487));
#30087=CARTESIAN_POINT('Ctrl Pts',(-2.23403148460003,4.08086248395284,20.3163097183853));
#30088=CARTESIAN_POINT('Ctrl Pts',(2.22665448024071,4.08489230124149,20.1173767800218));
#30089=CARTESIAN_POINT('Ctrl Pts',(3.8935518733233,1.49431200163386,19.9799947145718));
#30090=CARTESIAN_POINT('Ctrl Pts',(3.93915414306072,0.0954158123487556,
19.9089236285761));
#30091=CARTESIAN_POINT('Ctrl Pts',(3.93864968270786,0.00168892045947167,
19.904163522035));
#30092=CARTESIAN_POINT('',(3.93210890370979,0.00278794103289284,18.6541635611165));
#30093=CARTESIAN_POINT('Ctrl Pts',(3.93299963840903,0.00168649768106297,
19.904163522035));
#30094=CARTESIAN_POINT('Ctrl Pts',(3.9330486303541,-0.112565246857441,19.898352669845));
#30095=CARTESIAN_POINT('Ctrl Pts',(3.92811496827436,-0.227020618325729,
19.892541817655));
#30096=CARTESIAN_POINT('Ctrl Pts',(3.91817167495914,-0.341203349262369,
19.886730965465));
#30097=CARTESIAN_POINT('Ctrl Pts',(3.90824065065424,-0.455245190349012,
19.8809272832743));
#30098=CARTESIAN_POINT('Ctrl Pts',(3.89331231900895,-0.569014642437496,
19.8751236010836));
#30099=CARTESIAN_POINT('Ctrl Pts',(3.87341170273253,-0.682034296157216,
19.8693199188928));
#30100=CARTESIAN_POINT('Ctrl Pts',(3.8535300506206,-0.794946248523693,19.8635217672837));
#30101=CARTESIAN_POINT('Ctrl Pts',(3.8286856079953,-0.907109409310164,19.8577236156747));
#30102=CARTESIAN_POINT('Ctrl Pts',(3.79895523187636,-1.01805115107208,19.8519254640656));
#30103=CARTESIAN_POINT('Ctrl Pts',(3.76924333610225,-1.12892393165994,19.8461309165765));
#30104=CARTESIAN_POINT('Ctrl Pts',(3.73465165362909,-1.23857639555064,19.8403363690873));
#30105=CARTESIAN_POINT('Ctrl Pts',(3.6953080442437,-1.34654649312522,19.8345418215982));
#30106=CARTESIAN_POINT('Ctrl Pts',(3.65597667055693,-1.4544830124492,19.8287490761892));
#30107=CARTESIAN_POINT('Ctrl Pts',(3.61189645120518,-1.56073780846829,19.8229563307802));
#30108=CARTESIAN_POINT('Ctrl Pts',(3.5632447555487,-1.66486510326053,19.8171635853712));
#30109=CARTESIAN_POINT('Ctrl Pts',(3.51459582578694,-1.76898647831797,19.8113711692852));
#30110=CARTESIAN_POINT('Ctrl Pts',(3.46137611556296,-1.87098020983424,19.8055787531992));
#30111=CARTESIAN_POINT('Ctrl Pts',(3.40381032984178,-1.97042235027478,19.7997863371132));
#30112=CARTESIAN_POINT('Ctrl Pts',(3.34623318594587,-2.06988411141871,19.7939927781388));
#30113=CARTESIAN_POINT('Ctrl Pts',(3.28430847461729,-2.16679291556439,19.7881992191643));
#30114=CARTESIAN_POINT('Ctrl Pts',(3.21830542378325,-2.26075191015009,19.7824056601898));
#30115=CARTESIAN_POINT('Ctrl Pts',(3.1522329179153,-2.3548097778193,19.7766060046512));
#30116=CARTESIAN_POINT('Ctrl Pts',(3.08207374807207,-2.4459112927357,19.7708063491126));
#30117=CARTESIAN_POINT('Ctrl Pts',(3.00813882466016,-2.53369094634136,19.7650066935739));
#30118=CARTESIAN_POINT('Ctrl Pts',(2.9341614336904,-2.6215210197939,19.7592037067651));
#30119=CARTESIAN_POINT('Ctrl Pts',(2.85640425805586,-2.70602512345837,19.7534007199562));
#30120=CARTESIAN_POINT('Ctrl Pts',(2.77521530495391,-2.78687441610661,19.7475977331474));
#30121=CARTESIAN_POINT('Ctrl Pts',(2.69389971201757,-2.86784981878142,19.7417856947464));
#30122=CARTESIAN_POINT('Ctrl Pts',(2.60914196606835,-2.94515874444064,19.7359736563455));
#30123=CARTESIAN_POINT('Ctrl Pts',(2.52132351813424,-3.01851233505897,19.7301616179445));
#30124=CARTESIAN_POINT('Ctrl Pts',(2.4676803058116,-3.06331980238201,19.726611379728));
#30125=CARTESIAN_POINT('Ctrl Pts',(2.4128956596014,-3.10665225137229,19.7230611415115));
#30126=CARTESIAN_POINT('Ctrl Pts',(2.3570614911877,-3.14845202071749,19.719510903295));
#30127=CARTESIAN_POINT('Ctrl Pts',(2.26471130551823,-3.21758919190929,19.7136387793289));
#30128=CARTESIAN_POINT('Ctrl Pts',(2.16916182641396,-3.28277561125713,19.7077666553629));
#30129=CARTESIAN_POINT('Ctrl Pts',(2.07078572851163,-3.34370086380234,19.7018945313969));
#30130=CARTESIAN_POINT('Ctrl Pts',(1.97253717717358,-3.40454712554791,19.6960300207562));
#30131=CARTESIAN_POINT('Ctrl Pts',(1.87146964315069,-3.46114299143328,19.6901655101154));
#30132=CARTESIAN_POINT('Ctrl Pts',(1.76798770760113,-3.51321910301241,19.6843009994747));
#30133=CARTESIAN_POINT('Ctrl Pts',(1.6646122539337,-3.56524162879083,19.6784425233571));
#30134=CARTESIAN_POINT('Ctrl Pts',(1.55882770738393,-3.61275346616886,19.6725840472395));
#30135=CARTESIAN_POINT('Ctrl Pts',(1.45106580890289,-3.65552964948077,19.6667255711219));
#30136=CARTESIAN_POINT('Ctrl Pts',(1.3390547160197,-3.69999255436344,19.6606360875306));
#30137=CARTESIAN_POINT('Ctrl Pts',(1.22490751072737,-3.73933841604629,19.6545466039394));
#30138=CARTESIAN_POINT('Ctrl Pts',(1.1091354361331,-3.77336820152948,19.6484571203481));
#30139=CARTESIAN_POINT('Ctrl Pts',(0.997884351103417,-3.80606909741997,
19.6426054358277));
#30140=CARTESIAN_POINT('Ctrl Pts',(0.885133354146109,-3.83386119200615,
19.6367537513073));
#30141=CARTESIAN_POINT('Ctrl Pts',(0.771353650297388,-3.85661801922006,
19.6309020667869));
#30142=CARTESIAN_POINT('Ctrl Pts',(0.657591300326917,-3.87937137552313,
19.6250512747756));
#30143=CARTESIAN_POINT('Ctrl Pts',(0.542800960703745,-3.89709091039657,
19.6192004827643));
#30144=CARTESIAN_POINT('Ctrl Pts',(0.427464802167997,-3.90970111938336,
19.6133496907529));
#30145=CARTESIAN_POINT('Ctrl Pts',(0.312118299304034,-3.922312459361,19.6074983739928));
#30146=CARTESIAN_POINT('Ctrl Pts',(0.196226291200135,-3.92981351756233,
19.6016470572327));
#30147=CARTESIAN_POINT('Ctrl Pts',(0.0802761432412044,-3.93218065973911,
19.5957957404725));
#30148=CARTESIAN_POINT('Ctrl Pts',(-0.0357124884206846,-3.9345485875673,
19.589942481668));
#30149=CARTESIAN_POINT('Ctrl Pts',(-0.151758885199464,-3.93177920276364,
19.5840892228635));
#30150=CARTESIAN_POINT('Ctrl Pts',(-0.267376323888127,-3.92390098007379,
19.5782359640589));
#30151=CARTESIAN_POINT('Ctrl Pts',(-0.383125299964816,-3.91601379436896,
19.5723760460308));
#30152=CARTESIAN_POINT('Ctrl Pts',(-0.498443931167058,-3.90300619770365,
19.5665161280027));
#30153=CARTESIAN_POINT('Ctrl Pts',(-0.61285115149628,-3.88495848962504,
19.5606562099746));
#30154=CARTESIAN_POINT('Ctrl Pts',(-0.727335405481232,-3.86689862950807,
19.554792346296));
#30155=CARTESIAN_POINT('Ctrl Pts',(-0.840906622513694,-3.84379198277531,
19.5489284826173));
#30156=CARTESIAN_POINT('Ctrl Pts',(-0.953096166476963,-3.81576947645516,
19.5430646189387));
#30157=CARTESIAN_POINT('Ctrl Pts',(-1.06545121699102,-3.78770563020081,
19.5371921046513));
#30158=CARTESIAN_POINT('Ctrl Pts',(-1.17642013158342,-3.7547115679444,19.5313195903639));
#30159=CARTESIAN_POINT('Ctrl Pts',(-1.28555151431262,-3.71696735310502,
19.5254470760765));
#30160=CARTESIAN_POINT('Ctrl Pts',(-1.31571308883352,-3.70653566132085,
19.5238240390282));
#30161=CARTESIAN_POINT('Ctrl Pts',(-1.34573443536757,-3.69574140548776,
19.5222010019798));
#30162=CARTESIAN_POINT('Ctrl Pts',(-1.37560634343977,-3.68458901207289,
19.5205779649315));
#30163=CARTESIAN_POINT('Ctrl Pts',(-1.48368246374951,-3.64423981812336,
19.5147058409655));
#30164=CARTESIAN_POINT('Ctrl Pts',(-1.59016298721955,-3.59906382509579,
19.5088337169995));
#30165=CARTESIAN_POINT('Ctrl Pts',(-1.69458534382848,-3.549206884993,19.5029615930334));
#30166=CARTESIAN_POINT('Ctrl Pts',(-1.79887231477886,-3.49941458540291,
19.4970970823927));
#30167=CARTESIAN_POINT('Ctrl Pts',(-1.90110605583298,-3.44495358413687,
19.491232571752));
#30168=CARTESIAN_POINT('Ctrl Pts',(-2.00084130301933,-3.3860187654725,19.4853680611113));
#30169=CARTESIAN_POINT('Ctrl Pts',(-2.10047392362842,-3.32714459015029,
19.4795095849937));
#30170=CARTESIAN_POINT('Ctrl Pts',(-2.19761281028807,-3.26380596308677,
19.473651108876));
#30171=CARTESIAN_POINT('Ctrl Pts',(-2.29183537723579,-3.19624460948321,
19.4677926327584));
#30172=CARTESIAN_POINT('Ctrl Pts',(-2.38977326480867,-3.12601922221301,
19.4617031491672));
#30173=CARTESIAN_POINT('Ctrl Pts',(-2.48455970176964,-3.05123143794407,
19.4556136655759));
#30174=CARTESIAN_POINT('Ctrl Pts',(-2.57575096437571,-2.97220389097343,
19.4495241819846));
#30175=CARTESIAN_POINT('Ctrl Pts',(-2.66338113724523,-2.89626243118241,
19.4436724974642));
#30176=CARTESIAN_POINT('Ctrl Pts',(-2.74769131345249,-2.81640642311625,
19.4378208129438));
#30177=CARTESIAN_POINT('Ctrl Pts',(-2.82832046458625,-2.73296402274208,
19.4319691284234));
#30178=CARTESIAN_POINT('Ctrl Pts',(-2.90893731802168,-2.64953434914792,
19.4261183364121));
#30179=CARTESIAN_POINT('Ctrl Pts',(-2.9858739755019,-2.56251966807222,19.4202675444008));
#30180=CARTESIAN_POINT('Ctrl Pts',(-3.05880636455274,-2.47228489947491,
19.4144167523895));
#30181=CARTESIAN_POINT('Ctrl Pts',(-3.1317452948009,-2.38204203785563,19.4085654356294));
#30182=CARTESIAN_POINT('Ctrl Pts',(-3.20067898280185,-2.2885788361392,19.4027141188692));
#30183=CARTESIAN_POINT('Ctrl Pts',(-3.26532419492947,-2.19229261322667,
19.3968628021091));
#30184=CARTESIAN_POINT('Ctrl Pts',(-3.32999086271838,-2.09597443304278,
19.3910095433046));
#30185=CARTESIAN_POINT('Ctrl Pts',(-3.39036599409769,-1.99683171163408,
19.3851562845001));
#30186=CARTESIAN_POINT('Ctrl Pts',(-3.44621054912699,-1.89528938452307,
19.3793030256956));
#30187=CARTESIAN_POINT('Ctrl Pts',(-3.50211863823058,-1.7936315332083,19.3734431076675));
#30188=CARTESIAN_POINT('Ctrl Pts',(-3.55348566356971,-1.68956898960502,
19.3675831896394));
#30189=CARTESIAN_POINT('Ctrl Pts',(-3.60011924961873,-1.58354993243808,
19.3617232716112));
#30190=CARTESIAN_POINT('Ctrl Pts',(-3.64678423539589,-1.47745948960572,
19.3558594079326));
#30191=CARTESIAN_POINT('Ctrl Pts',(-3.68870928644008,-1.36941029453041,
19.349995544254));
#30192=CARTESIAN_POINT('Ctrl Pts',(-3.7257513437638,-1.2598674233594,19.3441316805753));
#30193=CARTESIAN_POINT('Ctrl Pts',(-3.76284804702802,-1.15016295011623,
19.3382591662879));
#30194=CARTESIAN_POINT('Ctrl Pts',(-3.79504726499192,-1.0389607985519,19.3323866520005));
#30195=CARTESIAN_POINT('Ctrl Pts',(-3.82225659977131,-0.92673808894675,
19.3265141377131));
#30196=CARTESIAN_POINT('Ctrl Pts',(-3.82977667656401,-0.895722137952037,
19.3248911006648));
#30197=CARTESIAN_POINT('Ctrl Pts',(-3.83691590493077,-0.864628269986622,
19.3232680636164));
#30198=CARTESIAN_POINT('Ctrl Pts',(-3.84367303262681,-0.833466626960804,
19.3216450265681));
#30199=CARTESIAN_POINT('Ctrl Pts',(-3.8681202204012,-0.720724264720546,
19.3157729026021));
#30200=CARTESIAN_POINT('Ctrl Pts',(-3.88764376046699,-0.606716354434508,
19.309900778636));
#30201=CARTESIAN_POINT('Ctrl Pts',(-3.90211643013503,-0.49191093265982,
19.30402865467));
#30202=CARTESIAN_POINT('Ctrl Pts',(-3.91657033569951,-0.377254358393829,
19.2981641440293));
#30203=CARTESIAN_POINT('Ctrl Pts',(-3.925986342335,-0.261802735244286,19.2922996333886));
#30204=CARTESIAN_POINT('Ctrl Pts',(-3.93028783644347,-0.146036032212877,
19.2864351227478));
#30205=CARTESIAN_POINT('Ctrl Pts',(-3.93458490435729,-0.0303884519675996,
19.2805766466302));
#30206=CARTESIAN_POINT('Ctrl Pts',(-3.93377791241063,0.0855731526423031,
19.2747181705126));
#30207=CARTESIAN_POINT('Ctrl Pts',(-3.92784191503611,0.20136258462152,19.268859694395));
#30208=CARTESIAN_POINT('Ctrl Pts',(-3.92167185342207,0.321717747282592,
19.2627702108038));
#30209=CARTESIAN_POINT('Ctrl Pts',(-3.90995992100421,0.441886428504692,
19.2566807272125));
#30210=CARTESIAN_POINT('Ctrl Pts',(-3.89273783065155,0.561320925865294,
19.2505912436212));
#30211=CARTESIAN_POINT('Ctrl Pts',(-3.87618827632311,0.676091413203553,
19.2447395591008));
#30212=CARTESIAN_POINT('Ctrl Pts',(-3.85455090471959,0.790183533818666,
19.2388878745804));
#30213=CARTESIAN_POINT('Ctrl Pts',(-3.82790675910924,0.903116184976115,
19.23303619006));
#30214=CARTESIAN_POINT('Ctrl Pts',(-3.80126667731029,1.01603161144929,19.2271853980487));
#30215=CARTESIAN_POINT('Ctrl Pts',(-3.76962143476761,1.12778751783175,19.2213346060374));
#30216=CARTESIAN_POINT('Ctrl Pts',(-3.73310297856709,1.2379140323195,19.2154838140261));
#30217=CARTESIAN_POINT('Ctrl Pts',(-3.69658124708061,1.34805042389035,19.2096324972659));
#30218=CARTESIAN_POINT('Ctrl Pts',(-3.65518556320843,1.45655674063406,19.2037811805058));
#30219=CARTESIAN_POINT('Ctrl Pts',(-3.60909720303922,1.56297996756661,19.1979298637456));
#30220=CARTESIAN_POINT('Ctrl Pts',(-3.56299354620353,1.66943851622901,19.1920766049411));
#30221=CARTESIAN_POINT('Ctrl Pts',(-3.51219428030129,1.77381222116112,19.1862233461366));
#30222=CARTESIAN_POINT('Ctrl Pts',(-3.45692779915915,1.87567033121513,19.1803700873321));
#30223=CARTESIAN_POINT('Ctrl Pts',(-3.40159844161468,1.97764432473732,19.174510169304));
#30224=CARTESIAN_POINT('Ctrl Pts',(-3.34179192191341,2.07709664735771,19.1686502512758));
#30225=CARTESIAN_POINT('Ctrl Pts',(-3.27778140669515,2.17362325390661,19.1627903332477));
#30226=CARTESIAN_POINT('Ctrl Pts',(-3.21372779136531,2.27021485458184,19.1569264695691));
#30227=CARTESIAN_POINT('Ctrl Pts',(-3.14546478700233,2.36387648331367,19.1510626058905));
#30228=CARTESIAN_POINT('Ctrl Pts',(-3.07330642652341,2.45423646144578,19.1451987422119));
#30229=CARTESIAN_POINT('Ctrl Pts',(-3.0010416151137,2.54472974227095,19.1393262279245));
#30230=CARTESIAN_POINT('Ctrl Pts',(-2.92487024945583,2.63191134126862,19.1334537136371));
#30231=CARTESIAN_POINT('Ctrl Pts',(-2.84514387151662,2.71544570013312,19.1275811993497));
#30232=CARTESIAN_POINT('Ctrl Pts',(-2.82310920990589,2.73853280603239,19.1259581623013));
#30233=CARTESIAN_POINT('Ctrl Pts',(-2.80080319511398,2.76134155239987,19.124335125253));
#30234=CARTESIAN_POINT('Ctrl Pts',(-2.77823368432067,2.78386540538618,19.1227120882046));
#30235=CARTESIAN_POINT('Ctrl Pts',(-2.69657752904987,2.86535637138854,19.1168399642386));
#30236=CARTESIAN_POINT('Ctrl Pts',(-2.61119600685286,2.94338821035076,19.1109678402725));
#30237=CARTESIAN_POINT('Ctrl Pts',(-2.52241419876744,3.01760096928941,19.1050957163065));
#30238=CARTESIAN_POINT('Ctrl Pts',(-2.4337474980592,3.09171750991241,19.0992312056658));
#30239=CARTESIAN_POINT('Ctrl Pts',(-2.34168959270523,3.16202455458497,19.0933666950251));
#30240=CARTESIAN_POINT('Ctrl Pts',(-2.24660295070884,3.22819828725968,19.0875021843844));
#30241=CARTESIAN_POINT('Ctrl Pts',(-2.15161415192113,3.29430392782177,19.0816437082668));
#30242=CARTESIAN_POINT('Ctrl Pts',(-2.05360315272201,3.35628448135034,19.0757852321492));
#30243=CARTESIAN_POINT('Ctrl Pts',(-1.95296558031232,3.41385624215715,19.0699267560316));
#30244=CARTESIAN_POINT('Ctrl Pts',(-1.84835973511434,3.47369813375422,19.0638372724403));
#30245=CARTESIAN_POINT('Ctrl Pts',(-1.740916265865,3.52877609870654,19.0577477888491));
#30246=CARTESIAN_POINT('Ctrl Pts',(-1.63111316826112,3.57882087178517,19.0516583052578));
#30247=CARTESIAN_POINT('Ctrl Pts',(-1.52559796702751,3.62691135754844,19.0458066207374));
#30248=CARTESIAN_POINT('Ctrl Pts',(-1.41790438138372,3.67035418719305,19.039954936217));
#30249=CARTESIAN_POINT('Ctrl Pts',(-1.30848102283375,3.7089575911412,19.0341032516966));
#30250=CARTESIAN_POINT('Ctrl Pts',(-1.19907435372463,3.74755510723108,19.0282524596853));
#30251=CARTESIAN_POINT('Ctrl Pts',(-1.08793882603715,3.78131452773204,19.022401667674));
#30252=CARTESIAN_POINT('Ctrl Pts',(-0.975541106863264,3.81009298427479,
19.0165508756627));
#30253=CARTESIAN_POINT('Ctrl Pts',(-0.863133306905562,3.8388740219144,19.0106995589025));
#30254=CARTESIAN_POINT('Ctrl Pts',(-0.74946349093942,3.86267310497829,19.0048482421424));
#30255=CARTESIAN_POINT('Ctrl Pts',(-0.635010796838518,3.88139798112723,
18.9989969253823));
#30256=CARTESIAN_POINT('Ctrl Pts',(-0.520520116037529,3.90012907203816,
18.9931436665778));
#30257=CARTESIAN_POINT('Ctrl Pts',(-0.405246448207288,3.91378254055294,
18.9872904077732));
#30258=CARTESIAN_POINT('Ctrl Pts',(-0.289675657461678,3.92231781138068,
18.9814371489687));
#30259=CARTESIAN_POINT('Ctrl Pts',(-0.173973382399091,3.93086279274382,
18.9755772309406));
#30260=CARTESIAN_POINT('Ctrl Pts',(-0.0579737222475329,3.9342779235025,
18.9697173129125));
#30261=CARTESIAN_POINT('Ctrl Pts',(0.0578357375176416,3.93257473259769,
18.9638573948843));
#30262=CARTESIAN_POINT('Ctrl Pts',(0.173723175106275,3.9308703948857,18.9579935312057));
#30263=CARTESIAN_POINT('Ctrl Pts',(0.289419745614166,3.92404089752945,18.9521296675271));
#30264=CARTESIAN_POINT('Ctrl Pts',(0.404443016103308,3.91214964523665,18.9462658038485));
#30265=CARTESIAN_POINT('Ctrl Pts',(0.51963597357111,3.90024085048774,18.9403932895611));
#30266=CARTESIAN_POINT('Ctrl Pts',(0.634153241211034,3.88325545787445,18.9345207752737));
#30267=CARTESIAN_POINT('Ctrl Pts',(0.747522511328454,3.86130795133685,18.9286482609863));
#30268=CARTESIAN_POINT('Ctrl Pts',(0.778855347068329,3.85524213106183,18.9270252239379));
#30269=CARTESIAN_POINT('Ctrl Pts',(0.810100584535425,3.84879757193155,18.9254021868896));
#30270=CARTESIAN_POINT('Ctrl Pts',(0.841248480266414,3.8419773547549,18.9237791498412));
#30271=CARTESIAN_POINT('Ctrl Pts',(0.953941104996053,3.81730191017589,18.9179070258752));
#30272=CARTESIAN_POINT('Ctrl Pts',(1.06573606917177,3.78762265463477,18.9120349019091));
#30273=CARTESIAN_POINT('Ctrl Pts',(1.17615483650006,3.75301862513064,18.9061627779431));
#30274=CARTESIAN_POINT('Ctrl Pts',(1.28643044370397,3.71845946043789,18.9002982673024));
#30275=CARTESIAN_POINT('Ctrl Pts',(1.39533301147143,3.67898834185165,18.8944337566617));
#30276=CARTESIAN_POINT('Ctrl Pts',(1.50239420867585,3.63473529183863,18.8885692460209));
#30277=CARTESIAN_POINT('Ctrl Pts',(1.60934524097383,3.59052777777366,18.8827107699033));
#30278=CARTESIAN_POINT('Ctrl Pts',(1.71445829170005,3.54154827648078,18.8768522937857));
#30279=CARTESIAN_POINT('Ctrl Pts',(1.81728086276403,3.48797638550373,18.870993817668));
#30280=CARTESIAN_POINT('Ctrl Pts',(1.92415786400686,3.43229208390254,18.8649043340768));
#30281=CARTESIAN_POINT('Ctrl Pts',(2.02855960189874,3.37164590980433,18.8588148504855));
#30282=CARTESIAN_POINT('Ctrl Pts',(2.13000122152532,3.30629457191894,18.8527253668942));
#30283=CARTESIAN_POINT('Ctrl Pts',(2.22748146700065,3.24349525461052,18.8468736823738));
#30284=CARTESIAN_POINT('Ctrl Pts',(2.32222806536106,3.17635160311987,18.8410219978534));
#30285=CARTESIAN_POINT('Ctrl Pts',(2.41383724745544,3.10513747566782,18.835170313333));
#30286=CARTESIAN_POINT('Ctrl Pts',(2.50543245715824,3.0339342099182,18.8293195213217));
#30287=CARTESIAN_POINT('Ctrl Pts',(2.59389087574815,2.95866195628142,18.8234687293104));
#30288=CARTESIAN_POINT('Ctrl Pts',(2.67884012529963,2.87963618936223,18.817617937299));
#30289=CARTESIAN_POINT('Ctrl Pts',(2.76379699382277,2.80060333473973,18.8117666205389));
#30290=CARTESIAN_POINT('Ctrl Pts',(2.84524376494135,2.71781657921138,18.8059153037787));
#30291=CARTESIAN_POINT('Ctrl Pts',(2.92284391261533,2.63162924107624,18.8000639870186));
#30292=CARTESIAN_POINT('Ctrl Pts',(3.00046981567637,2.54541329747681,18.7942107282141));
#30293=CARTESIAN_POINT('Ctrl Pts',(3.0742462802051,2.45579483409477,18.7883574694096));
#30294=CARTESIAN_POINT('Ctrl Pts',(3.14387662888212,2.36316075254494,18.7825042106051));
#30295=CARTESIAN_POINT('Ctrl Pts',(3.21358619566299,2.27042128165798,18.776644292577));
#30296=CARTESIAN_POINT('Ctrl Pts',(3.27913998300501,2.17465967537183,18.7707843745489));
#30297=CARTESIAN_POINT('Ctrl Pts',(3.34028422613442,2.07629243813043,18.7649244565208));
#30298=CARTESIAN_POINT('Ctrl Pts',(3.40146963943263,1.977858967413,18.7590605928421));
#30299=CARTESIAN_POINT('Ctrl Pts',(3.45823939450847,1.8768167318374,18.7531967291635));
#30300=CARTESIAN_POINT('Ctrl Pts',(3.5103861611893,1.77360593124027,18.7473328654849));
#30301=CARTESIAN_POINT('Ctrl Pts',(3.56260985688832,1.67024286989788,18.7414603511975));
#30302=CARTESIAN_POINT('Ctrl Pts',(3.61019678340428,1.56470523407687,18.7355878369101));
#30303=CARTESIAN_POINT('Ctrl Pts',(3.65298806191879,1.45745230435813,18.7297153226227));
#30304=CARTESIAN_POINT('Ctrl Pts',(3.66481465389889,1.42780989397715,18.7280922855744));
#30305=CARTESIAN_POINT('Ctrl Pts',(3.67627522564143,1.39803654176343,18.7264692485261));
#30306=CARTESIAN_POINT('Ctrl Pts',(3.68736710460949,1.36814211098258,18.7248462114777));
#30307=CARTESIAN_POINT('Ctrl Pts',(3.73357286612343,1.24361001473156,18.7180850790313));
#30308=CARTESIAN_POINT('Ctrl Pts',(3.77350486082523,1.11663082843232,18.7113239465848));
#30309=CARTESIAN_POINT('Ctrl Pts',(3.80693270518357,0.987801790949832,18.7045628141384));
#30310=CARTESIAN_POINT('Ctrl Pts',(3.84022696812535,0.859487568755357,18.6978286999358));
#30311=CARTESIAN_POINT('Ctrl Pts',(3.86706885387637,0.72933839269851,18.6910945857331));
#30312=CARTESIAN_POINT('Ctrl Pts',(3.88727736453247,0.59796629603476,18.6843604715305));
#30313=CARTESIAN_POINT('Ctrl Pts',(3.90733771924772,0.467557335987658,18.6776757275681));
#30314=CARTESIAN_POINT('Ctrl Pts',(3.92086151599839,0.335943479056069,18.6709909836057));
#30315=CARTESIAN_POINT('Ctrl Pts',(3.92771916947069,0.203742793179215,18.6643062396433));
#30316=CARTESIAN_POINT('Ctrl Pts',(3.93118751002375,0.136880709549541,18.6609253501503));
#30317=CARTESIAN_POINT('Ctrl Pts',(3.93295144684361,0.0698688121993667,
18.6575444606572));
#30318=CARTESIAN_POINT('Ctrl Pts',(3.93299901128319,0.00278877131541848,
18.6541635711641));
#30319=CARTESIAN_POINT('',(3.92848299207397,-0.00269963646582772,17.404163522035));
#30320=CARTESIAN_POINT('Ctrl Pts',(3.92864672146726,0.00278471154748855,
18.654163522035));
#30321=CARTESIAN_POINT('Ctrl Pts',(3.92313822395883,-0.844483024166633,
18.6114134390614));
#30322=CARTESIAN_POINT('Ctrl Pts',(3.23759721412511,-3.01409901755068,18.5023523766335));
#30323=CARTESIAN_POINT('Ctrl Pts',(-0.34305832318172,-4.63968169964443,
18.3269803347509));
#30324=CARTESIAN_POINT('Ctrl Pts',(-4.08939297301161,-2.2183778757014,18.1280473963876));
#30325=CARTESIAN_POINT('Ctrl Pts',(-4.07633013060909,2.24229078252717,17.929114458024));
#30326=CARTESIAN_POINT('Ctrl Pts',(-0.315878526192679,4.64161136285755,
17.7301815196607));
#30327=CARTESIAN_POINT('Ctrl Pts',(3.24728594800834,2.99873176707587,17.5551978743308));
#30328=CARTESIAN_POINT('Ctrl Pts',(3.92320510227271,0.836958268880239,17.4465252084557));
#30329=CARTESIAN_POINT('Ctrl Pts',(3.92848299207397,-0.00269963646582772,
17.404163522035));
#30330=CARTESIAN_POINT('',(3.9349711294896,-0.00179957505841655,16.1541641208363));
#30331=CARTESIAN_POINT('Ctrl Pts',(3.92848299207397,-0.00269963646582772,
17.404163522035));
#30332=CARTESIAN_POINT('Ctrl Pts',(3.93146686122864,-0.47740248525043,17.3802142290012));
#30333=CARTESIAN_POINT('Ctrl Pts',(3.63168221550235,-2.26282468683885,17.2899539565132));
#30334=CARTESIAN_POINT('Ctrl Pts',(0.968478616941049,-4.55042684323626,
17.1333827045702));
#30335=CARTESIAN_POINT('Ctrl Pts',(-3.30560419092301,-3.27373123821604,
16.9344497662068));
#30336=CARTESIAN_POINT('Ctrl Pts',(-4.54083008587026,1.01252032985696,16.7355168278434));
#30337=CARTESIAN_POINT('Ctrl Pts',(-1.60165030493022,4.36795737019433,16.5365838894799));
#30338=CARTESIAN_POINT('Ctrl Pts',(2.69574705430972,3.72499564046276,16.3428000122829));
#30339=CARTESIAN_POINT('Ctrl Pts',(3.93162038906629,1.20261472713713,16.2153271145402));
#30340=CARTESIAN_POINT('Ctrl Pts',(3.93851192302398,-0.00178002804509826,
16.1541651962521));
#30341=CARTESIAN_POINT('',(3.93299839598119,0.00355207114488244,14.9041635220072));
#30342=CARTESIAN_POINT('Ctrl Pts',(3.93299958330002,-0.0018104590140189,
16.154163522035));
#30343=CARTESIAN_POINT('Ctrl Pts',(3.93295297921618,-0.103052100462509,
16.149015018941));
#30344=CARTESIAN_POINT('Ctrl Pts',(3.92899756056485,-0.204200298766311,
16.143866515847));
#30345=CARTESIAN_POINT('Ctrl Pts',(3.92115268406435,-0.30504201063944,16.138718012753));
#30346=CARTESIAN_POINT('Ctrl Pts',(3.91220521205771,-0.420057000872728,
16.1328458887869));
#30347=CARTESIAN_POINT('Ctrl Pts',(3.8981780309882,-0.53487080847362,16.1269737648208));
#30348=CARTESIAN_POINT('Ctrl Pts',(3.87908363530141,-0.648998574988258,
16.1211016408548));
#30349=CARTESIAN_POINT('Ctrl Pts',(3.86001399587776,-0.762978372587534,
16.115237130214));
#30350=CARTESIAN_POINT('Ctrl Pts',(3.83589027426291,-0.876273493949008,
16.1093726195733));
#30351=CARTESIAN_POINT('Ctrl Pts',(3.80677686926452,-0.988402179091408,
16.1035081089325));
#30352=CARTESIAN_POINT('Ctrl Pts',(3.77769342167025,-1.10041548493225,16.0976496328149));
#30353=CARTESIAN_POINT('Ctrl Pts',(3.74363060639703,-1.21126434417529,16.0917911566972));
#30354=CARTESIAN_POINT('Ctrl Pts',(3.70470410337022,-1.32047586364608,16.0859326805796));
#30355=CARTESIAN_POINT('Ctrl Pts',(3.6642426767658,-1.43399373799459,16.0798431969883));
#30356=CARTESIAN_POINT('Ctrl Pts',(3.61852618315301,-1.54574204231883,16.0737537133971));
#30357=CARTESIAN_POINT('Ctrl Pts',(3.56774223274705,-1.65520523219119,16.0676642298058));
#30358=CARTESIAN_POINT('Ctrl Pts',(3.5189414351059,-1.76039379935491,16.0618125452854));
#30359=CARTESIAN_POINT('Ctrl Pts',(3.46546172033017,-1.86347196359888,16.055960860765));
#30360=CARTESIAN_POINT('Ctrl Pts',(3.40751883343924,-1.96400213842981,16.0501091762446));
#30361=CARTESIAN_POINT('Ctrl Pts',(3.34958478409809,-2.06451698022382,16.0442583842333));
#30362=CARTESIAN_POINT('Ctrl Pts',(3.28718912253459,-2.16248424723207,16.038407592222));
#30363=CARTESIAN_POINT('Ctrl Pts',(3.22059313080242,-2.25749172442077,16.0325568002107));
#30364=CARTESIAN_POINT('Ctrl Pts',(3.15399116617496,-2.35250772268857,16.0267054834505));
#30365=CARTESIAN_POINT('Ctrl Pts',(3.08318835979914,-2.44456306487948,16.0208541666904));
#30366=CARTESIAN_POINT('Ctrl Pts',(3.00848840717777,-2.53327584441114,16.0150028499303));
#30367=CARTESIAN_POINT('Ctrl Pts',(2.93376366173962,-2.62201806759854,16.0091495911258));
#30368=CARTESIAN_POINT('Ctrl Pts',(2.8551394642411,-2.70741520610614,16.0032963323212));
#30369=CARTESIAN_POINT('Ctrl Pts',(2.77295825322183,-2.78912020642513,15.9974430735167));
#30370=CARTESIAN_POINT('Ctrl Pts',(2.69068354504526,-2.87091816211885,15.9915831554886));
#30371=CARTESIAN_POINT('Ctrl Pts',(2.60484403939898,-2.94901530383245,15.9857232374605));
#30372=CARTESIAN_POINT('Ctrl Pts',(2.51581739640533,-3.0231030131215,15.9798633194324));
#30373=CARTESIAN_POINT('Ctrl Pts',(2.42673080922506,-3.09724060778557,15.9739994557537));
#30374=CARTESIAN_POINT('Ctrl Pts',(2.33445313996473,-3.16736314494313,15.9681355920751));
#30375=CARTESIAN_POINT('Ctrl Pts',(2.23939190322457,-3.23320474201252,15.9622717283965));
#30376=CARTESIAN_POINT('Ctrl Pts',(2.14419042830493,-3.29914347126768,15.9563992141091));
#30377=CARTESIAN_POINT('Ctrl Pts',(2.0461975388517,-3.36078843672843,15.9505266998217));
#30378=CARTESIAN_POINT('Ctrl Pts',(1.94584631039175,-3.41791912372643,15.9446541855343));
#30379=CARTESIAN_POINT('Ctrl Pts',(1.91811138227575,-3.43370882078768,15.9430311484861));
#30380=CARTESIAN_POINT('Ctrl Pts',(1.89019643316264,-3.44915397609759,15.9414081114379));
#30381=CARTESIAN_POINT('Ctrl Pts',(1.86211086521754,-3.4642505864384,15.9397850743898));
#30382=CARTESIAN_POINT('Ctrl Pts',(1.7604976969819,-3.5188698987253,15.9339129504237));
#30383=CARTESIAN_POINT('Ctrl Pts',(1.65630900294329,-3.56910622282458,15.9280408264577));
#30384=CARTESIAN_POINT('Ctrl Pts',(1.54995951462399,-3.61470807991829,15.9221687024917));
#30385=CARTESIAN_POINT('Ctrl Pts',(1.44374791052793,-3.66025081329882,15.916304191851));
#30386=CARTESIAN_POINT('Ctrl Pts',(1.33538145978728,-3.70117086733896,15.9104396812103));
#30387=CARTESIAN_POINT('Ctrl Pts',(1.22530033314438,-3.73726211197399,15.9045751705696));
#30388=CARTESIAN_POINT('Ctrl Pts',(1.11533247888564,-3.77331621907734,15.898716694452));
#30389=CARTESIAN_POINT('Ctrl Pts',(1.0036538486417,-3.80455127192809,15.8928582183344));
#30390=CARTESIAN_POINT('Ctrl Pts',(0.890724861888612,-3.83080908169717,
15.8869997422167));
#30391=CARTESIAN_POINT('Ctrl Pts',(0.773342935598185,-3.85810227168745,
15.8809102586255));
#30392=CARTESIAN_POINT('Ctrl Pts',(0.654610435968224,-3.8800174454089,15.8748207750342));
#30393=CARTESIAN_POINT('Ctrl Pts',(0.535062538391735,-3.896433892678,15.8687312914429));
#30394=CARTESIAN_POINT('Ctrl Pts',(0.420183079204392,-3.91220926491191,
15.8628796069225));
#30395=CARTESIAN_POINT('Ctrl Pts',(0.304551159006151,-3.92290724918914,
15.8570279224021));
#30396=CARTESIAN_POINT('Ctrl Pts',(0.188651558702059,-3.92847293352001,
15.8511762378817));
#30397=CARTESIAN_POINT('Ctrl Pts',(0.0727696356063224,-3.93403776896303,
15.8453254458704));
#30398=CARTESIAN_POINT('Ctrl Pts',(-0.0433794735954423,-3.93447184106165,
15.8394746538591));
#30399=CARTESIAN_POINT('Ctrl Pts',(-0.159307730771794,-3.92977226400161,
15.8336238618477));
#30400=CARTESIAN_POINT('Ctrl Pts',(-0.275246385380741,-3.92507226544351,
15.8277725450876));
#30401=CARTESIAN_POINT('Ctrl Pts',(-0.390963735490063,-3.915237719182,15.8219212283275));
#30402=CARTESIAN_POINT('Ctrl Pts',(-0.505974327755538,-3.90031780495543,
15.8160699115673));
#30403=CARTESIAN_POINT('Ctrl Pts',(-0.621023091886366,-3.88539293882882,
15.8102166527628));
#30404=CARTESIAN_POINT('Ctrl Pts',(-0.735364221981617,-3.86537940176006,
15.8043633939583));
#30405=CARTESIAN_POINT('Ctrl Pts',(-0.848520656818351,-3.84037780627799,
15.7985101351537));
#30406=CARTESIAN_POINT('Ctrl Pts',(-0.961805829171468,-3.81534776660437,
15.7926502171256));
#30407=CARTESIAN_POINT('Ctrl Pts',(-1.07390321213151,-3.78531843083299,
15.7867902990975));
#30408=CARTESIAN_POINT('Ctrl Pts',(-1.1843490534434,-3.75044081670511,15.7809303810693));
#30409=CARTESIAN_POINT('Ctrl Pts',(-1.29486926110112,-3.71553971848147,
15.7750665173907));
#30410=CARTESIAN_POINT('Ctrl Pts',(-1.40373532545892,-3.675783983138,15.7692026537121));
#30411=CARTESIAN_POINT('Ctrl Pts',(-1.5105033222041,-3.63137284144859,15.7633387900334));
#30412=CARTESIAN_POINT('Ctrl Pts',(-1.61742882741433,-3.58689618264756,
15.757466275746));
#30413=CARTESIAN_POINT('Ctrl Pts',(-1.72224971474705,-3.53775058540083,
15.7515937614586));
#30414=CARTESIAN_POINT('Ctrl Pts',(-1.82454642256008,-3.4841813029639,15.7457212471712));
#30415=CARTESIAN_POINT('Ctrl Pts',(-1.85281903946332,-3.46937590176869,
15.7440982101229));
#30416=CARTESIAN_POINT('Ctrl Pts',(-1.88089901846817,-3.45423285102442,
15.7424751730745));
#30417=CARTESIAN_POINT('Ctrl Pts',(-1.90877791066121,-3.43875789897629,
15.7408521360261));
#30418=CARTESIAN_POINT('Ctrl Pts',(-2.00964332908048,-3.38276975201031,
15.7349800120601));
#30419=CARTESIAN_POINT('Ctrl Pts',(-2.10821239750051,-3.32224611220501,
15.7291078880941));
#30420=CARTESIAN_POINT('Ctrl Pts',(-2.20404941189026,-3.2574000659953,15.723235764128));
#30421=CARTESIAN_POINT('Ctrl Pts',(-2.2997621716879,-3.19263809397209,15.7173712534873));
#30422=CARTESIAN_POINT('Ctrl Pts',(-2.39274958229793,-3.12356508957238,
15.7115067428466));
#30423=CARTESIAN_POINT('Ctrl Pts',(-2.48260035200154,-3.05044004895062,
15.7056422322059));
#30424=CARTESIAN_POINT('Ctrl Pts',(-2.572358666157,-2.97739025326816,15.6997837560883));
#30425=CARTESIAN_POINT('Ctrl Pts',(-2.65898644048793,-2.90029697409149,
15.6939252799707));
#30426=CARTESIAN_POINT('Ctrl Pts',(-2.7421017816784,-2.81946215064437,15.6880668038531));
#30427=CARTESIAN_POINT('Ctrl Pts',(-2.82849447086952,-2.73543990303206,
15.6819773202618));
#30428=CARTESIAN_POINT('Ctrl Pts',(-2.91109165153983,-2.64737522763415,
15.6758878366705));
#30429=CARTESIAN_POINT('Ctrl Pts',(-2.98950257228258,-2.55565321792997,
15.6697983530793));
#30430=CARTESIAN_POINT('Ctrl Pts',(-3.06485148557938,-2.46751302404955,
15.6639466685589));
#30431=CARTESIAN_POINT('Ctrl Pts',(-3.13633466294613,-2.37599612293355,
15.6580949840385));
#30432=CARTESIAN_POINT('Ctrl Pts',(-3.20364394887505,-2.28148075793689,
15.6522432995181));
#30433=CARTESIAN_POINT('Ctrl Pts',(-3.27094296867473,-2.18697980858791,
15.6463925075068));
#30434=CARTESIAN_POINT('Ctrl Pts',(-3.33406912306604,-2.08948164132976,
15.6405417154955));
#30435=CARTESIAN_POINT('Ctrl Pts',(-3.3927562735057,-1.98939535250983,15.6346909234842));
#30436=CARTESIAN_POINT('Ctrl Pts',(-3.45144868750846,-1.88930008709975,
15.628839606724));
#30437=CARTESIAN_POINT('Ctrl Pts',(-3.50570109699303,-1.78661659533198,
15.6229882899639));
#30438=CARTESIAN_POINT('Ctrl Pts',(-3.55529257023308,-1.68177993210926,
15.6171369732038));
#30439=CARTESIAN_POINT('Ctrl Pts',(-3.60490050281836,-1.57690847373489,
15.6112837143993));
#30440=CARTESIAN_POINT('Ctrl Pts',(-3.64984424644787,-1.46988279641373,
15.6054304555947));
#30441=CARTESIAN_POINT('Ctrl Pts',(-3.68995068175951,-1.36115868515855,
15.5995771967902));
#30442=CARTESIAN_POINT('Ctrl Pts',(-3.73010274596424,-1.25231087901974,
15.5937172787621));
#30443=CARTESIAN_POINT('Ctrl Pts',(-3.76540637408494,-1.1417611702238,15.587857360734));
#30444=CARTESIAN_POINT('Ctrl Pts',(-3.79573805128353,-1.02998138140373,
15.5819974427059));
#30445=CARTESIAN_POINT('Ctrl Pts',(-3.82609015166841,-0.918126328052883,
15.5761335790273));
#30446=CARTESIAN_POINT('Ctrl Pts',(-3.85146354480521,-0.80503994787316,
15.5702697153486));
#30447=CARTESIAN_POINT('Ctrl Pts',(-3.87178599830118,-0.691203431240699,
15.56440585167));
#30448=CARTESIAN_POINT('Ctrl Pts',(-3.89213843230215,-0.577198978376718,
15.5585333373826));
#30449=CARTESIAN_POINT('Ctrl Pts',(-3.90742500076692,-0.462442588687338,
15.5526608230952));
#30450=CARTESIAN_POINT('Ctrl Pts',(-3.91762536085701,-0.34741982092271,
15.5467883088079));
#30451=CARTESIAN_POINT('Ctrl Pts',(-3.92044452170068,-0.315629993882404,
15.5451652717595));
#30452=CARTESIAN_POINT('Ctrl Pts',(-3.92287547864341,-0.283819812255978,
15.5435422347111));
#30453=CARTESIAN_POINT('Ctrl Pts',(-3.92491850314786,-0.251999491363761,
15.5419191976628));
#30454=CARTESIAN_POINT('Ctrl Pts',(-3.93231013550017,-0.136874042375434,
15.5360470736967));
#30455=CARTESIAN_POINT('Ctrl Pts',(-3.93464458701186,-0.0212300950170252,
15.5301749497307));
#30456=CARTESIAN_POINT('Ctrl Pts',(-3.93186572583331,0.0944505903489437,
15.5243028257647));
#30457=CARTESIAN_POINT('Ctrl Pts',(-3.92909046750346,0.209981293409424,
15.5184383151239));
#30458=CARTESIAN_POINT('Ctrl Pts',(-3.92121509001258,0.325548230282245,
15.5125738044832));
#30459=CARTESIAN_POINT('Ctrl Pts',(-3.90823528300636,0.440665374932272,
15.5067092938425));
#30460=CARTESIAN_POINT('Ctrl Pts',(-3.89526883209242,0.555664065185687,
15.5008508177249));
#30461=CARTESIAN_POINT('Ctrl Pts',(-3.87720844499173,0.670213475474608,
15.4949923416073));
#30462=CARTESIAN_POINT('Ctrl Pts',(-3.85410183080451,0.783829112619164,
15.4891338654897));
#30463=CARTESIAN_POINT('Ctrl Pts',(-3.83008409221207,0.901924764835474,
15.4830443818984));
#30464=CARTESIAN_POINT('Ctrl Pts',(-3.80061399142199,1.01901103417153,15.4769548983072));
#30465=CARTESIAN_POINT('Ctrl Pts',(-3.76580442055278,1.13455104166587,15.4708654147159));
#30466=CARTESIAN_POINT('Ctrl Pts',(-3.73235419050217,1.24557912199635,15.4650137301955));
#30467=CARTESIAN_POINT('Ctrl Pts',(-3.69397381613963,1.35517900657719,15.4591620456751));
#30468=CARTESIAN_POINT('Ctrl Pts',(-3.65081505610943,1.46288701753918,15.4533103611547));
#30469=CARTESIAN_POINT('Ctrl Pts',(-3.60766287872829,1.57057860068822,15.4474595691434));
#30470=CARTESIAN_POINT('Ctrl Pts',(-3.55973391850471,1.67637850030463,15.441608777132));
#30471=CARTESIAN_POINT('Ctrl Pts',(-3.50722859885247,1.77984172200545,15.4357579851207));
#30472=CARTESIAN_POINT('Ctrl Pts',(-3.45471857007634,1.88331422316847,15.4299066683606));
#30473=CARTESIAN_POINT('Ctrl Pts',(-3.39763155303805,1.98444926112361,15.4240553516005));
#30474=CARTESIAN_POINT('Ctrl Pts',(-3.33621424116639,2.08282585374739,15.4182040348403));
#30475=CARTESIAN_POINT('Ctrl Pts',(-3.27477654496913,2.18123509743379,15.4123507760358));
#30476=CARTESIAN_POINT('Ctrl Pts',(-3.20900591493992,2.27688372483143,15.4064975172313));
#30477=CARTESIAN_POINT('Ctrl Pts',(-3.13919232299163,2.36937978367134,15.4006442584267));
#30478=CARTESIAN_POINT('Ctrl Pts',(-3.06929930446503,2.46198107481996,15.3947843403986));
#30479=CARTESIAN_POINT('Ctrl Pts',(-2.99535439242745,2.55142230835978,15.3889244223705));
#30480=CARTESIAN_POINT('Ctrl Pts',(-2.91768785720815,2.63734460545074,15.3830645043424));
#30481=CARTESIAN_POINT('Ctrl Pts',(-2.83996902688801,2.72332475648327,15.3772006406638));
#30482=CARTESIAN_POINT('Ctrl Pts',(-2.75852387350708,2.80578095971988,15.3713367769851));
#30483=CARTESIAN_POINT('Ctrl Pts',(-2.67371826015857,2.88439242567557,15.3654729133065));
#30484=CARTESIAN_POINT('Ctrl Pts',(-2.5887875381407,2.96311986244398,15.3596003990191));
#30485=CARTESIAN_POINT('Ctrl Pts',(-2.50048677607265,3.03799097548627,15.3537278847317));
#30486=CARTESIAN_POINT('Ctrl Pts',(-2.40921355118324,3.10872627691713,15.3478553704443));
#30487=CARTESIAN_POINT('Ctrl Pts',(-2.38398758862848,3.12827599774004,15.346232333396));
#30488=CARTESIAN_POINT('Ctrl Pts',(-2.35853473377561,3.14751006612287,15.3446092963477));
#30489=CARTESIAN_POINT('Ctrl Pts',(-2.33286372890652,3.16642319066046,15.3429862592993));
#30490=CARTESIAN_POINT('Ctrl Pts',(-2.23998641407328,3.23485059469533,15.3371141353333));
#30491=CARTESIAN_POINT('Ctrl Pts',(-2.14394017682271,3.29930284472971,15.3312420113673));
#30492=CARTESIAN_POINT('Ctrl Pts',(-2.04510005975041,3.35947239095797,15.3253698874012));
#30493=CARTESIAN_POINT('Ctrl Pts',(-1.94638809085243,3.41956392617484,15.3195053767605));
#30494=CARTESIAN_POINT('Ctrl Pts',(-1.84488979547726,3.475383586732,15.3136408661198));
#30495=CARTESIAN_POINT('Ctrl Pts',(-1.74101180716334,3.52666512265027,15.3077763554791));
#30496=CARTESIAN_POINT('Ctrl Pts',(-1.63724070826596,3.57789389037826,15.3019178793615));
#30497=CARTESIAN_POINT('Ctrl Pts',(-1.53109515544061,3.62459363979043,15.2960594032439));
#30498=CARTESIAN_POINT('Ctrl Pts',(-1.42300860101158,3.66654272052666,15.2902009271263));
#30499=CARTESIAN_POINT('Ctrl Pts',(-1.31066005056624,3.71014590908352,15.284111443535));
#30500=CARTESIAN_POINT('Ctrl Pts',(-1.1962146655235,3.74861583435038,15.2780219599437));
#30501=CARTESIAN_POINT('Ctrl Pts',(-1.08018519929101,3.78175738714591,15.2719324763525));
#30502=CARTESIAN_POINT('Ctrl Pts',(-0.968686773966867,3.81360473652606,
15.2660807918321));
#30503=CARTESIAN_POINT('Ctrl Pts',(-0.855726099957108,3.84053193399624,
15.2602291073117));
#30504=CARTESIAN_POINT('Ctrl Pts',(-0.741775337648642,3.86241612833939,
15.2543774227913));
#30505=CARTESIAN_POINT('Ctrl Pts',(-0.627841955308467,3.88429698486718,
15.24852663078));
#30506=CARTESIAN_POINT('Ctrl Pts',(-0.512919190806072,3.90113628966476,
15.2426758387686));
#30507=CARTESIAN_POINT('Ctrl Pts',(-0.397489779359752,3.91286223566644,
15.2368250467573));
#30508=CARTESIAN_POINT('Ctrl Pts',(-0.282050015221484,3.92458923335074,
15.2309737299972));
#30509=CARTESIAN_POINT('Ctrl Pts',(-0.166103925128302,3.93120191878143,
15.2251224132371));
#30510=CARTESIAN_POINT('Ctrl Pts',(-0.0501390412770755,3.93268039338818,
15.2192710964769));
#30511=CARTESIAN_POINT('Ctrl Pts',(0.0658643311677466,3.93415935869873,
15.2134178376724));
#30512=CARTESIAN_POINT('Ctrl Pts',(0.181886096613168,3.93050071954967,15.2075645788679));
#30513=CARTESIAN_POINT('Ctrl Pts',(0.297439764364947,3.92173667991293,15.2017113200634));
#30514=CARTESIAN_POINT('Ctrl Pts',(0.413124896953059,3.91296266947165,15.1958514020352));
#30515=CARTESIAN_POINT('Ctrl Pts',(0.528340456412262,3.89907169643602,15.1899914840071));
#30516=CARTESIAN_POINT('Ctrl Pts',(0.642606006256308,3.88014774470294,15.184131565979));
#30517=CARTESIAN_POINT('Ctrl Pts',(0.756948494365145,3.86121105093159,15.1782677023004));
#30518=CARTESIAN_POINT('Ctrl Pts',(0.870339295670883,3.83723471591799,15.1724038386218));
#30519=CARTESIAN_POINT('Ctrl Pts',(0.982310791193972,3.8083532542956,15.1665399749431));
#30520=CARTESIAN_POINT('Ctrl Pts',(1.09444747159405,3.7794291855734,15.1606674606557));
#30521=CARTESIAN_POINT('Ctrl Pts',(1.20516027346793,3.74558566845092,15.1547949463683));
#30522=CARTESIAN_POINT('Ctrl Pts',(1.31399919406769,3.70700622038721,15.1489224320809));
#30523=CARTESIAN_POINT('Ctrl Pts',(1.34407993832644,3.69634368804627,15.1472993950326));
#30524=CARTESIAN_POINT('Ctrl Pts',(1.3740176801626,3.68531967695767,15.1456763579843));
#30525=CARTESIAN_POINT('Ctrl Pts',(1.40380324329441,3.67393868404416,15.1440533209359));
#30526=CARTESIAN_POINT('Ctrl Pts',(1.51156696888942,3.63276242049987,15.1381811969699));
#30527=CARTESIAN_POINT('Ctrl Pts',(1.6176981537394,3.5867717276716,15.1323090730038));
#30528=CARTESIAN_POINT('Ctrl Pts',(1.72173535916131,3.53611599824068,15.1264369490378));
#30529=CARTESIAN_POINT('Ctrl Pts',(1.82563767828066,3.48552594496877,15.1205724383971));
#30530=CARTESIAN_POINT('Ctrl Pts',(1.92745104863593,3.43028306229887,15.1147079277564));
#30531=CARTESIAN_POINT('Ctrl Pts',(2.02673171285057,3.37058564112022,15.1088434171157));
#30532=CARTESIAN_POINT('Ctrl Pts',(2.12591021824936,3.3109496479941,15.1029849409981));
#30533=CARTESIAN_POINT('Ctrl Pts',(2.22256084906092,3.246868445263,15.0971264648805));
#30534=CARTESIAN_POINT('Ctrl Pts',(2.31626288442289,3.17858698956706,15.0912679887628));
#30535=CARTESIAN_POINT('Ctrl Pts',(2.41365971516021,3.10761310562499,15.0851785051716));
#30536=CARTESIAN_POINT('Ctrl Pts',(2.50787022334694,3.03210111018839,15.0790890215803));
#30537=CARTESIAN_POINT('Ctrl Pts',(2.59845317081765,2.95237702861063,15.072999537989));
#30538=CARTESIAN_POINT('Ctrl Pts',(2.68549878373087,2.8757662344308,15.0671478534686));
#30539=CARTESIAN_POINT('Ctrl Pts',(2.76919449786016,2.79526645012846,15.0612961689482));
#30540=CARTESIAN_POINT('Ctrl Pts',(2.84918181025936,2.71120858881924,15.0554444844278));
#30541=CARTESIAN_POINT('Ctrl Pts',(2.92915692285471,2.62716354816106,15.0495936924165));
#30542=CARTESIAN_POINT('Ctrl Pts',(3.00542447342669,2.53956180892775,15.0437429004052));
#30543=CARTESIAN_POINT('Ctrl Pts',(3.07766319562631,2.44877076393182,15.0378921083939));
#30544=CARTESIAN_POINT('Ctrl Pts',(3.14990839680929,2.35797157602235,15.0320407916338));
#30545=CARTESIAN_POINT('Ctrl Pts',(3.21812379389503,2.26398283724511,15.0261894748736));
#30546=CARTESIAN_POINT('Ctrl Pts',(3.28202920647656,2.16720402542881,15.0203381581135));
#30547=CARTESIAN_POINT('Ctrl Pts',(3.34595582918103,2.0703930928513,15.014484899309));
#30548=CARTESIAN_POINT('Ctrl Pts',(3.40556939528597,1.97079059070546,15.0086316405044));
#30549=CARTESIAN_POINT('Ctrl Pts',(3.46063412841561,1.86882327394677,15.0027783816999));
#30550=CARTESIAN_POINT('Ctrl Pts',(3.51576150841988,1.76673994947596,14.9969184636718));
#30551=CARTESIAN_POINT('Ctrl Pts',(3.56632952936074,1.66228680432709,14.9910585456437));
#30552=CARTESIAN_POINT('Ctrl Pts',(3.61214925603401,1.55591347835699,14.9851986276156));
#30553=CARTESIAN_POINT('Ctrl Pts',(3.65799983444048,1.4494685281824,14.979334763937));
#30554=CARTESIAN_POINT('Ctrl Pts',(3.69909560617089,1.34110120835168,14.9734709002583));
#30555=CARTESIAN_POINT('Ctrl Pts',(3.73529708060636,1.23127767770459,14.9676070365797));
#30556=CARTESIAN_POINT('Ctrl Pts',(3.77155196092052,1.121292130945,14.9617345222923));
#30557=CARTESIAN_POINT('Ctrl Pts',(3.80289802211392,1.00984648231908,14.9558620080049));
#30558=CARTESIAN_POINT('Ctrl Pts',(3.829246525485,0.897418546198519,14.9499894937175));
#30559=CARTESIAN_POINT('Ctrl Pts',(3.83652868693191,0.866345874994292,14.9483664566692));
#30560=CARTESIAN_POINT('Ctrl Pts',(3.84342941401067,0.835198207785689,14.9467434196208));
#30561=CARTESIAN_POINT('Ctrl Pts',(3.84994753223704,0.803985695781907,14.9451203825724));
#30562=CARTESIAN_POINT('Ctrl Pts',(3.88332231308886,0.644167982788329,14.9368099310093));
#30563=CARTESIAN_POINT('Ctrl Pts',(3.90675505914046,0.482207980055859,14.9284994794461));
#30564=CARTESIAN_POINT('Ctrl Pts',(3.92003124128456,0.319130173053279,14.9201890278829));
#30565=CARTESIAN_POINT('Ctrl Pts',(3.92856497469929,0.214306172018008,14.9148471926003));
#30566=CARTESIAN_POINT('Ctrl Pts',(3.93290314243907,0.10902067104636,14.9095053573176));
#30567=CARTESIAN_POINT('Ctrl Pts',(3.93299839598069,0.00355207169431283,
14.904163522035));
#30568=CARTESIAN_POINT('',(3.93299999319383,0.000231381426135529,13.654163522081));
#30569=CARTESIAN_POINT('Ctrl Pts',(3.93299839598119,0.00355207114488768,
14.9041635220072));
#30570=CARTESIAN_POINT('Ctrl Pts',(3.9331014152117,-0.110515032762491,14.8983861846387));
#30571=CARTESIAN_POINT('Ctrl Pts',(3.92823788678433,-0.224740458271784,
14.8926088472702));
#30572=CARTESIAN_POINT('Ctrl Pts',(3.91839323831547,-0.338649420379848,
14.8868315099017));
#30573=CARTESIAN_POINT('Ctrl Pts',(3.90840744311791,-0.454191541601957,
14.8809713404978));
#30574=CARTESIAN_POINT('Ctrl Pts',(3.89329652357728,-0.569407612697175,
14.875111171094));
#30575=CARTESIAN_POINT('Ctrl Pts',(3.87310012082037,-0.683801472725241,
14.8692510016901));
#30576=CARTESIAN_POINT('Ctrl Pts',(3.85321605094451,-0.796426257126016,
14.8634814585039));
#30577=CARTESIAN_POINT('Ctrl Pts',(3.82840275016944,-0.908253645725761,
14.8577119153178));
#30578=CARTESIAN_POINT('Ctrl Pts',(3.79875019094154,-1.018815972991,14.8519423721317));
#30579=CARTESIAN_POINT('Ctrl Pts',(3.76910388804956,-1.1293549729254,14.8461740462502));
#30580=CARTESIAN_POINT('Ctrl Pts',(3.73462046600092,-1.23862903038604,14.8404057203688));
#30581=CARTESIAN_POINT('Ctrl Pts',(3.69544052012651,-1.34618288586919,14.8346373944874));
#30582=CARTESIAN_POINT('Ctrl Pts',(3.65625872133245,-1.4537418278487,14.8288687958071));
#30583=CARTESIAN_POINT('Ctrl Pts',(3.61238010408342,-1.55958000593681,14.8231001971268));
#30584=CARTESIAN_POINT('Ctrl Pts',(3.5639941217805,-1.66326032235307,14.8173315984465));
#30585=CARTESIAN_POINT('Ctrl Pts',(3.51426540979626,-1.76981780756068,14.8114029189268));
#30586=CARTESIAN_POINT('Ctrl Pts',(3.45977569300044,-1.8740954742395,14.805474239407));
#30587=CARTESIAN_POINT('Ctrl Pts',(3.40078145967277,-1.97564532837904,14.7995455598872));
#30588=CARTESIAN_POINT('Ctrl Pts',(3.34329862424868,-2.07459353439134,14.7937687696842));
#30589=CARTESIAN_POINT('Ctrl Pts',(3.28153957424957,-2.17095167930799,14.7879919794813));
#30590=CARTESIAN_POINT('Ctrl Pts',(3.21578513749197,-2.26433543219324,14.7822151892783));
#30591=CARTESIAN_POINT('Ctrl Pts',(3.14743737568872,-2.36140219777171,14.7762105651001));
#30592=CARTESIAN_POINT('Ctrl Pts',(3.07477291673487,-2.45525472351012,14.7702059409219));
#30593=CARTESIAN_POINT('Ctrl Pts',(2.99815157968798,-2.54550115011061,14.7642013167437));
#30594=CARTESIAN_POINT('Ctrl Pts',(2.92153024264109,-2.63574757671111,14.7581966925655));
#30595=CARTESIAN_POINT('Ctrl Pts',(2.8409524305194,-2.72238758486848,14.7521920683873));
#30596=CARTESIAN_POINT('Ctrl Pts',(2.7568176077604,-2.80507498608187,14.7461874442091));
#30597=CARTESIAN_POINT('Ctrl Pts',(2.67453933447666,-2.88593777714813,14.740315320243));
#30598=CARTESIAN_POINT('Ctrl Pts',(2.58856231310642,-2.96331299295254,14.734443196277));
#30599=CARTESIAN_POINT('Ctrl Pts',(2.4992143736846,-3.03684318238006,14.728571072311));
#30600=CARTESIAN_POINT('Ctrl Pts',(2.40998227564033,-3.11027803845699,14.7227065616703));
#30601=CARTESIAN_POINT('Ctrl Pts',(2.31738826707177,-3.17987752154393,14.7168420510296));
#30602=CARTESIAN_POINT('Ctrl Pts',(2.22179728694164,-3.24532060292027,14.7109775403889));
#30603=CARTESIAN_POINT('Ctrl Pts',(2.12630466897917,-3.31069634401686,14.7051190642713));
#30604=CARTESIAN_POINT('Ctrl Pts',(2.02782155246119,-3.37192395821685,14.6992605881536));
#30605=CARTESIAN_POINT('Ctrl Pts',(1.9267457271836,-3.42872278010045,14.693402112036));
#30606=CARTESIAN_POINT('Ctrl Pts',(1.82168434822659,-3.48776125476871,14.6873126284448));
#30607=CARTESIAN_POINT('Ctrl Pts',(1.71382193747888,-3.54201419621266,14.6812231448535));
#30608=CARTESIAN_POINT('Ctrl Pts',(1.60363854014731,-3.59121601028874,14.6751336612622));
#30609=CARTESIAN_POINT('Ctrl Pts',(1.4977578901862,-3.63849645525419,14.6692819767418));
#30610=CARTESIAN_POINT('Ctrl Pts',(1.38973453766306,-3.68111268627017,14.6634302922214));
#30611=CARTESIAN_POINT('Ctrl Pts',(1.28001855055742,-3.71887637737918,14.657578607701));
#30612=CARTESIAN_POINT('Ctrl Pts',(1.17031929752487,-3.75663430870437,14.6517278156897));
#30613=CARTESIAN_POINT('Ctrl Pts',(1.05892831401735,-3.78954103719815,14.6458770236784));
#30614=CARTESIAN_POINT('Ctrl Pts',(0.946313348311815,-3.81745727504669,
14.6400262316671));
#30615=CARTESIAN_POINT('Ctrl Pts',(0.833688282337644,-3.84537601666104,
14.634174914907));
#30616=CARTESIAN_POINT('Ctrl Pts',(0.719839417229986,-3.86830327838651,
14.6283235981468));
#30617=CARTESIAN_POINT('Ctrl Pts',(0.605246583779176,-3.88615048252427,
14.6224722813867));
#30618=CARTESIAN_POINT('Ctrl Pts',(0.490615717116629,-3.90400361012578,
14.6166190225821));
#30619=CARTESIAN_POINT('Ctrl Pts',(0.375240799394601,-3.91677326392419,
14.6107657637776));
#30620=CARTESIAN_POINT('Ctrl Pts',(0.259607991412779,-3.92442259329887,
14.6049125049731));
#30621=CARTESIAN_POINT('Ctrl Pts',(0.143843628557176,-3.93208062527775,
14.599052586945));
#30622=CARTESIAN_POINT('Ctrl Pts',(0.0278212025794243,-3.93460667824846,
14.5931926689169));
#30623=CARTESIAN_POINT('Ctrl Pts',(-0.0879718037169931,-3.93201601748401,
14.5873327508887));
#30624=CARTESIAN_POINT('Ctrl Pts',(-0.203842776758241,-3.92942361235352,
14.5814688872101));
#30625=CARTESIAN_POINT('Ctrl Pts',(-0.319483611039676,-3.92170766081718,
14.5756050235315));
#30626=CARTESIAN_POINT('Ctrl Pts',(-0.434412373700088,-3.90893526290424,
14.5697411598528));
#30627=CARTESIAN_POINT('Ctrl Pts',(-0.549510683917648,-3.89614402263353,
14.5638686455654));
#30628=CARTESIAN_POINT('Ctrl Pts',(-0.66389441902465,-3.87828151180883,
14.5579961312781));
#30629=CARTESIAN_POINT('Ctrl Pts',(-0.777092162557845,-3.85546583059572,
14.5521236169907));
#30630=CARTESIAN_POINT('Ctrl Pts',(-0.808377592026888,-3.84916006545323,
14.5505005799423));
#30631=CARTESIAN_POINT('Ctrl Pts',(-0.839572523284305,-3.84247624389752,
14.548877542894));
#30632=CARTESIAN_POINT('Ctrl Pts',(-0.870667236763032,-3.83541752131726,
14.5472545058456));
#30633=CARTESIAN_POINT('Ctrl Pts',(-0.983167448893482,-3.80987916772564,
14.5413823818796));
#30634=CARTESIAN_POINT('Ctrl Pts',(-1.09473167951701,-3.77934402944453,
14.5355102579135));
#30635=CARTESIAN_POINT('Ctrl Pts',(-1.20488201210244,-3.74389480847312,
14.5296381339475));
#30636=CARTESIAN_POINT('Ctrl Pts',(-1.31488953259477,-3.7084915481205,14.5237736233068));
#30637=CARTESIAN_POINT('Ctrl Pts',(-1.42348641061541,-3.66818700057338,
14.5179091126661));
#30638=CARTESIAN_POINT('Ctrl Pts',(-1.53020532523377,-3.62311477359277,
14.5120446020253));
#30639=CARTESIAN_POINT('Ctrl Pts',(-1.63681442715081,-3.57808892548527,
14.5061861259077));
#30640=CARTESIAN_POINT('Ctrl Pts',(-1.74154903076589,-3.5283053158792,14.5003276497901));
#30641=CARTESIAN_POINT('Ctrl Pts',(-1.84395802764422,-3.47394700481836,
14.4944691736725));
#30642=CARTESIAN_POINT('Ctrl Pts',(-1.95040514692368,-3.41744527354764,
14.4883796900812));
#30643=CARTESIAN_POINT('Ctrl Pts',(-2.05433904962757,-3.35600078497178,
14.4822902064899));
#30644=CARTESIAN_POINT('Ctrl Pts',(-2.15527686239815,-3.2898739560067,14.4762007228987));
#30645=CARTESIAN_POINT('Ctrl Pts',(-2.25227297506704,-3.2263294311485,14.4703490383783));
#30646=CARTESIAN_POINT('Ctrl Pts',(-2.34650222756403,-3.15846164932073,
14.4644973538579));
#30647=CARTESIAN_POINT('Ctrl Pts',(-2.43756296134085,-3.08654755503608,
14.4586456693374));
#30648=CARTESIAN_POINT('Ctrl Pts',(-2.52860980637626,-3.01464442921411,
14.4527948773261));
#30649=CARTESIAN_POINT('Ctrl Pts',(-2.61648876923034,-2.9386964741749,14.4469440853148));
#30650=CARTESIAN_POINT('Ctrl Pts',(-2.70082990059078,-2.85902200902246,
14.4410932933035));
#30651=CARTESIAN_POINT('Ctrl Pts',(-2.78517859638153,-2.77934039798603,
14.4352419765434));
#30652=CARTESIAN_POINT('Ctrl Pts',(-2.8659885293692,-2.69593189633899,14.4293906597832));
#30653=CARTESIAN_POINT('Ctrl Pts',(-2.94292589109389,-2.60915239101308,
14.4235393430231));
#30654=CARTESIAN_POINT('Ctrl Pts',(-3.01988878822831,-2.52234408368284,
14.4176860842186));
#30655=CARTESIAN_POINT('Ctrl Pts',(-3.09297628424887,-2.43216285712852,
14.4118328254141));
#30656=CARTESIAN_POINT('Ctrl Pts',(-3.16189467561598,-2.33899787522591,
14.4059795666096));
#30657=CARTESIAN_POINT('Ctrl Pts',(-3.23089147509628,-2.2457268999839,14.4001196485815));
#30658=CARTESIAN_POINT('Ctrl Pts',(-3.29570945667423,-2.14946572641166,
14.3942597305534));
#30659=CARTESIAN_POINT('Ctrl Pts',(-3.35609805496052,-2.05063279147931,
14.3883998125253));
#30660=CARTESIAN_POINT('Ctrl Pts',(-3.41652731461829,-1.95173330950337,
14.3825359488466));
#30661=CARTESIAN_POINT('Ctrl Pts',(-3.47252105313717,-1.85025897921189,
14.376672085168));
#30662=CARTESIAN_POINT('Ctrl Pts',(-3.52387531995793,-1.74665157641454,
14.3708082214894));
#30663=CARTESIAN_POINT('Ctrl Pts',(-3.57530534666929,-1.64289132778788,
14.364935707202));
#30664=CARTESIAN_POINT('Ctrl Pts',(-3.62208207524491,-1.53699210298548,
14.3590631929146));
#30665=CARTESIAN_POINT('Ctrl Pts',(-3.66405015128463,-1.42941438668816,
14.3531906786272));
#30666=CARTESIAN_POINT('Ctrl Pts',(-3.67564922774955,-1.39968221225936,
14.3515676415788));
#30667=CARTESIAN_POINT('Ctrl Pts',(-3.68688129123676,-1.36982190488367,
14.3499446045305));
#30668=CARTESIAN_POINT('Ctrl Pts',(-3.6977437448762,-1.33984334801833,14.3483215674821));
#30669=CARTESIAN_POINT('Ctrl Pts',(-3.73704394101808,-1.23138137395919,
14.3424494435161));
#30670=CARTESIAN_POINT('Ctrl Pts',(-3.77163387810056,-1.12100697259218,
14.3365773195501));
#30671=CARTESIAN_POINT('Ctrl Pts',(-3.80132490392914,-1.00916697070807,
14.330705195584));
#30672=CARTESIAN_POINT('Ctrl Pts',(-3.83097743475323,-0.897471971606928,
14.3248406849433));
#30673=CARTESIAN_POINT('Ctrl Pts',(-3.85574358012656,-0.784315546636132,
14.3189761743026));
#30674=CARTESIAN_POINT('Ctrl Pts',(-3.87548324739994,-0.670163113818152,
14.3131116636619));
#30675=CARTESIAN_POINT('Ctrl Pts',(-3.89520260275208,-0.556128142717823,
14.3072531875442));
#30676=CARTESIAN_POINT('Ctrl Pts',(-3.90990569772854,-0.441099607223665,
14.3013947114266));
#30677=CARTESIAN_POINT('Ctrl Pts',(-3.91950281128406,-0.325556004915201,
14.295536235309));
#30678=CARTESIAN_POINT('Ctrl Pts',(-3.92947835173971,-0.205456365315012,
14.2894467517177));
#30679=CARTESIAN_POINT('Ctrl Pts',(-3.93393683864074,-0.0848006435188474,
14.2833572681265));
#30680=CARTESIAN_POINT('Ctrl Pts',(-3.93283647814454,0.0358641349488431,
14.2772677845352));
#30681=CARTESIAN_POINT('Ctrl Pts',(-3.93177908758163,0.151816859959831,
14.2714161000148));
#30682=CARTESIAN_POINT('Ctrl Pts',(-3.92558886120765,0.267777495236413,
14.2655644154944));
#30683=CARTESIAN_POINT('Ctrl Pts',(-3.9142817964293,0.383258422141242,14.259712730974));
#30684=CARTESIAN_POINT('Ctrl Pts',(-3.90297645622411,0.498721735694511,
14.2538619389627));
#30685=CARTESIAN_POINT('Ctrl Pts',(-3.88655586962668,0.613705075021255,
14.2480111469514));
#30686=CARTESIAN_POINT('Ctrl Pts',(-3.86508798236867,0.727725146294467,
14.2421603549401));
#30687=CARTESIAN_POINT('Ctrl Pts',(-3.84361816968779,0.841755443858191,
14.23630903818));
#30688=CARTESIAN_POINT('Ctrl Pts',(-3.81710023294893,0.954821895326569,
14.2304577214198));
#30689=CARTESIAN_POINT('Ctrl Pts',(-3.78565325765257,1.06645131760644,14.2246064046597));
#30690=CARTESIAN_POINT('Ctrl Pts',(-3.75419584514628,1.17811778954537,14.2187531458552));
#30691=CARTESIAN_POINT('Ctrl Pts',(-3.71780625315916,1.28834588620145,14.2128998870507));
#30692=CARTESIAN_POINT('Ctrl Pts',(-3.67665323840663,1.39667818931708,14.2070466282462));
#30693=CARTESIAN_POINT('Ctrl Pts',(-3.6354534040726,1.50513374155858,14.201186710218));
#30694=CARTESIAN_POINT('Ctrl Pts',(-3.58947947704671,1.61168880857652,14.1953267921899));
#30695=CARTESIAN_POINT('Ctrl Pts',(-3.53894815525177,1.71590645270659,14.1894668741618));
#30696=CARTESIAN_POINT('Ctrl Pts',(-3.48838280927194,1.82019426955856,14.1836030104832));
#30697=CARTESIAN_POINT('Ctrl Pts',(-3.43325415445786,1.92214116691071,14.1777391468046));
#30698=CARTESIAN_POINT('Ctrl Pts',(-3.37382371522563,2.0213368196768,14.171875283126));
#30699=CARTESIAN_POINT('Ctrl Pts',(-3.31430560180668,2.12067880988031,14.1660027688386));
#30700=CARTESIAN_POINT('Ctrl Pts',(-3.25047326529065,2.21726111138966,14.1601302545512));
#30701=CARTESIAN_POINT('Ctrl Pts',(-3.18263023134453,2.31070418066265,14.1542577402638));
#30702=CARTESIAN_POINT('Ctrl Pts',(-3.16387987124665,2.33652984168647,14.1526347032155));
#30703=CARTESIAN_POINT('Ctrl Pts',(-3.14482338009861,2.36211591899212,14.1510116661671));
#30704=CARTESIAN_POINT('Ctrl Pts',(-3.12546767104173,2.38745488696079,14.1493886291187));
#30705=CARTESIAN_POINT('Ctrl Pts',(-3.05543900278274,2.47913089721128,14.1435165051527));
#30706=CARTESIAN_POINT('Ctrl Pts',(-2.98125596041094,2.56787687429722,14.1376443811867));
#30707=CARTESIAN_POINT('Ctrl Pts',(-2.90319258488583,2.65329263652993,14.1317722572206));
#30708=CARTESIAN_POINT('Ctrl Pts',(-2.82523042007706,2.73859765553095,14.1259077465799));
#30709=CARTESIAN_POINT('Ctrl Pts',(-2.74339820312727,2.82058074365197,14.1200432359392));
#30710=CARTESIAN_POINT('Ctrl Pts',(-2.65801185747595,2.8988725335063,14.1141787252985));
#30711=CARTESIAN_POINT('Ctrl Pts',(-2.57271337352471,2.97708376188787,14.1083202491809));
#30712=CARTESIAN_POINT('Ctrl Pts',(-2.48386833801991,3.0516109693087,14.1024617730633));
#30713=CARTESIAN_POINT('Ctrl Pts',(-2.39183089826932,3.12212010564683,14.0966032969457));
#30714=CARTESIAN_POINT('Ctrl Pts',(-2.29616430035355,3.19540951062949,14.0905138133544));
#30715=CARTESIAN_POINT('Ctrl Pts',(-2.19704866423883,3.26435711381618,14.0844243297631));
#30716=CARTESIAN_POINT('Ctrl Pts',(-2.09492169686658,3.32863216411751,14.0783348461719));
#30717=CARTESIAN_POINT('Ctrl Pts',(-1.99678286700823,3.39039722370915,14.0724831616515));
#30718=CARTESIAN_POINT('Ctrl Pts',(-1.89586386492152,3.4478475749194,14.0666314771311));
#30719=CARTESIAN_POINT('Ctrl Pts',(-1.79258363747961,3.50073319500935,14.0607797926106));
#30720=CARTESIAN_POINT('Ctrl Pts',(-1.68931916251746,3.55361074889263,14.0549290005993));
#30721=CARTESIAN_POINT('Ctrl Pts',(-1.5836945461416,3.60192476758717,14.049078208588));
#30722=CARTESIAN_POINT('Ctrl Pts',(-1.47615316630862,3.64547127674832,14.0432274165767));
#30723=CARTESIAN_POINT('Ctrl Pts',(-1.36860214124985,3.68902169153087,14.0373760998166));
#30724=CARTESIAN_POINT('Ctrl Pts',(-1.25913439420161,3.7278035915955,14.0315247830565));
#30725=CARTESIAN_POINT('Ctrl Pts',(-1.14821242878449,3.76166149704952,14.0256734662963));
#30726=CARTESIAN_POINT('Ctrl Pts',(-1.03725364851147,3.79553063989828,14.0198202074918));
#30727=CARTESIAN_POINT('Ctrl Pts',(-0.924840085338792,3.82447241787311,
14.0139669486873));
#30728=CARTESIAN_POINT('Ctrl Pts',(-0.811447817423676,3.84838166501172,
14.0081136898828));
#30729=CARTESIAN_POINT('Ctrl Pts',(-0.69792654368625,3.87231811358252,14.0022537718546));
#30730=CARTESIAN_POINT('Ctrl Pts',(-0.583424747514154,3.89121051805456,
13.9963938538265));
#30731=CARTESIAN_POINT('Ctrl Pts',(-0.468427178759808,3.90500511884416,
13.9905339357984));
#30732=CARTESIAN_POINT('Ctrl Pts',(-0.353352178851344,3.91880900793327,
13.9846700721198));
#30733=CARTESIAN_POINT('Ctrl Pts',(-0.23778115290438,3.92750822761183,13.9788062084411));
#30734=CARTESIAN_POINT('Ctrl Pts',(-0.122200679729478,3.93110111722831,
13.9729423447625));
#30735=CARTESIAN_POINT('Ctrl Pts',(-0.00644969756785038,3.93469930722081,
13.9670698304751));
#30736=CARTESIAN_POINT('Ctrl Pts',(0.109310347808056,3.933176137972,13.9611973161877));
#30737=CARTESIAN_POINT('Ctrl Pts',(0.224596083185247,3.92658192317668,13.9553248019003));
#30738=CARTESIAN_POINT('Ctrl Pts',(0.256458588835168,3.92475942358048,13.953701764852));
#30739=CARTESIAN_POINT('Ctrl Pts',(0.28828491594598,3.9225498739989,13.9520787278036));
#30740=CARTESIAN_POINT('Ctrl Pts',(0.320064996647098,3.91995502498706,13.9504556907553));
#30741=CARTESIAN_POINT('Ctrl Pts',(0.435044857223373,3.91056689975214,13.9445835667893));
#30742=CARTESIAN_POINT('Ctrl Pts',(0.549804072017342,3.89609987364663,13.9387114428232));
#30743=CARTESIAN_POINT('Ctrl Pts',(0.663857834011462,3.87656829892388,13.9328393188572));
#30744=CARTESIAN_POINT('Ctrl Pts',(0.777763723038539,3.85706204727557,13.9269748082165));
#30745=CARTESIAN_POINT('Ctrl Pts',(0.890965574425546,3.83250437410981,13.9211102975758));
#30746=CARTESIAN_POINT('Ctrl Pts',(1.0029818784939,3.80296152378812,13.9152457869351));
#30747=CARTESIAN_POINT('Ctrl Pts',(1.11488291889988,3.77344907276547,13.9093873108175));
#30748=CARTESIAN_POINT('Ctrl Pts',(1.22560044112199,3.73896175259183,13.9035288346999));
#30749=CARTESIAN_POINT('Ctrl Pts',(1.33466199872439,3.69961705439374,13.8976703585822));
#30750=CARTESIAN_POINT('Ctrl Pts',(1.44802399800976,3.65872094262836,13.891580874991));
#30751=CARTESIAN_POINT('Ctrl Pts',(1.55959630369189,3.61257658314208,13.8854913913997));
#30752=CARTESIAN_POINT('Ctrl Pts',(1.66886409402017,3.56137356025596,13.8794019078084));
#30753=CARTESIAN_POINT('Ctrl Pts',(1.77386489214363,3.51217005524115,13.873550223288));
#30754=CARTESIAN_POINT('Ctrl Pts',(1.87673737398412,3.45829575416619,13.8676985387676));
#30755=CARTESIAN_POINT('Ctrl Pts',(1.97704478296108,3.39996807722755,13.8618468542472));
#30756=CARTESIAN_POINT('Ctrl Pts',(2.07733689287751,3.34164929652766,13.8559960622359));
#30757=CARTESIAN_POINT('Ctrl Pts',(2.17506435053191,3.27887869825671,13.8501452702246));
#30758=CARTESIAN_POINT('Ctrl Pts',(2.26981594510753,3.21191914209178,13.8442944782133));
#30759=CARTESIAN_POINT('Ctrl Pts',(2.36457603781254,3.14495358042399,13.8384431614532));
#30760=CARTESIAN_POINT('Ctrl Pts',(2.45635939922749,3.07379855260564,13.8325918446931));
#30761=CARTESIAN_POINT('Ctrl Pts',(2.54478528928605,2.99875921531445,13.826740527933));
#30762=CARTESIAN_POINT('Ctrl Pts',(2.63324052778248,2.92369497256483,13.8208872691284));
#30763=CARTESIAN_POINT('Ctrl Pts',(2.71833576408495,2.84474412420843,13.8150340103239));
#30764=CARTESIAN_POINT('Ctrl Pts',(2.79972525940186,2.76225043612399,13.8091807515193));
#30765=CARTESIAN_POINT('Ctrl Pts',(2.8812073511449,2.67966289537878,13.8033208334912));
#30766=CARTESIAN_POINT('Ctrl Pts',(2.95897499634773,2.59352476425796,13.7974609154631));
#30767=CARTESIAN_POINT('Ctrl Pts',(3.03272102596443,2.50421488268744,13.791600997435));
#30768=CARTESIAN_POINT('Ctrl Pts',(3.10651671089327,2.41484486621786,13.7857371337563));
#30769=CARTESIAN_POINT('Ctrl Pts',(3.17628514007976,2.32229917614927,13.7798732700777));
#30770=CARTESIAN_POINT('Ctrl Pts',(3.24176199442451,2.22698634290937,13.7740094063991));
#30771=CARTESIAN_POINT('Ctrl Pts',(3.30733544287201,2.13153290032437,13.7681368921117));
#30772=CARTESIAN_POINT('Ctrl Pts',(3.36860446279701,2.03330451671025,13.7622643778243));
#30773=CARTESIAN_POINT('Ctrl Pts',(3.42535020062575,1.93273510939113,13.7563918635369));
#30774=CARTESIAN_POINT('Ctrl Pts',(3.44103350599118,1.90493988131309,13.7547688264885));
#30775=CARTESIAN_POINT('Ctrl Pts',(3.45637158232319,1.87696595378804,13.7531457894402));
#30776=CARTESIAN_POINT('Ctrl Pts',(3.47136046246101,1.84882274425173,13.7515227523918));
#30777=CARTESIAN_POINT('Ctrl Pts',(3.52866492773603,1.74122754309106,13.7453176677343));
#30778=CARTESIAN_POINT('Ctrl Pts',(3.58103620167279,1.63082901965534,13.7391125830767));
#30779=CARTESIAN_POINT('Ctrl Pts',(3.62820672022146,1.51809255163835,13.7329074984191));
#30780=CARTESIAN_POINT('Ctrl Pts',(3.67528768351236,1.40557011865349,13.7267141943816));
#30781=CARTESIAN_POINT('Ctrl Pts',(3.71718742956168,1.29071889958609,13.720520890344));
#30782=CARTESIAN_POINT('Ctrl Pts',(3.75368432305832,1.17402853578019,13.7143275863065));
#30783=CARTESIAN_POINT('Ctrl Pts',(3.79009025522458,1.0576289997604,13.7081497178614));
#30784=CARTESIAN_POINT('Ctrl Pts',(3.82112007752275,0.939399784372105,13.7019718494164));
#30785=CARTESIAN_POINT('Ctrl Pts',(3.84660061620373,0.819849193096546,13.6957939809713));
#30786=CARTESIAN_POINT('Ctrl Pts',(3.87204208990804,0.70048188841153,13.6896255840013));
#30787=CARTESIAN_POINT('Ctrl Pts',(3.89195115264444,0.579797577402339,13.6834571870313));
#30788=CARTESIAN_POINT('Ctrl Pts',(3.90620429215287,0.45831978788454,13.6772887900613));
#30789=CARTESIAN_POINT('Ctrl Pts',(3.92042982092566,0.337077321337482,13.6711323423168));
#30790=CARTESIAN_POINT('Ctrl Pts',(3.92902122565854,0.215044780944509,13.6649758945723));
#30791=CARTESIAN_POINT('Ctrl Pts',(3.93190608507485,0.0927552594271314,
13.6588194468278));
#30792=CARTESIAN_POINT('Ctrl Pts',(3.93263332741248,0.0619273733287159,
13.6572674719122));
#30793=CARTESIAN_POINT('Ctrl Pts',(3.93299817815724,0.0310832048097634,
13.6557154969966));
#30794=CARTESIAN_POINT('Ctrl Pts',(3.93299999319383,0.000231381426136011,
13.654163522081));
#30795=CARTESIAN_POINT('',(3.93299832708652,-0.00362755215277343,12.404163522035));
#30796=CARTESIAN_POINT('Ctrl Pts',(3.93299999319388,0.000231380512522024,
13.654163522035));
#30797=CARTESIAN_POINT('Ctrl Pts',(3.93300713064364,-0.12109080676601,13.6480605118815));
#30798=CARTESIAN_POINT('Ctrl Pts',(3.92739626933809,-0.242314977188312,
13.641957501728));
#30799=CARTESIAN_POINT('Ctrl Pts',(3.9162204337665,-0.362913921129693,13.6358544915745));
#30800=CARTESIAN_POINT('Ctrl Pts',(3.90503076600943,-0.483662128806295,
13.6297439278052));
#30801=CARTESIAN_POINT('Ctrl Pts',(3.88826242076357,-0.603783209724141,
13.6236333640359));
#30802=CARTESIAN_POINT('Ctrl Pts',(3.86601983502594,-0.722758351861834,
13.6175228002666));
#30803=CARTESIAN_POINT('Ctrl Pts',(3.84372661366624,-0.842004342919838,
13.6113983256957));
#30804=CARTESIAN_POINT('Ctrl Pts',(3.81593430937306,-0.960098827271787,
13.6052738511248));
#30805=CARTESIAN_POINT('Ctrl Pts',(3.78279806763248,-1.07653508048553,13.5991493765539));
#30806=CARTESIAN_POINT('Ctrl Pts',(3.74962104396456,-1.19311463585328,13.5930173643787));
#30807=CARTESIAN_POINT('Ctrl Pts',(3.71108707651018,-1.30803154905568,13.5868853522035));
#30808=CARTESIAN_POINT('Ctrl Pts',(3.66739993048077,-1.42079792719078,13.5807533400283));
#30809=CARTESIAN_POINT('Ctrl Pts',(3.62361518202276,-1.53381623920967,13.5746076281878));
#30810=CARTESIAN_POINT('Ctrl Pts',(3.57465438680126,-1.64467408370087,13.5684619163473));
#30811=CARTESIAN_POINT('Ctrl Pts',(3.52076837296381,-1.75290589135236,13.5623162045067));
#30812=CARTESIAN_POINT('Ctrl Pts',(3.49234115815661,-1.81000287489173,13.5590740743473));
#30813=CARTESIAN_POINT('Ctrl Pts',(3.46254399245362,-1.86636948408595,13.5558319441879));
#30814=CARTESIAN_POINT('Ctrl Pts',(3.43141852376606,-1.9219406636926,13.5525898140285));
#30815=CARTESIAN_POINT('Ctrl Pts',(3.37504428780194,-2.0225908040454,13.5467176900624));
#30816=CARTESIAN_POINT('Ctrl Pts',(3.31414339153923,-2.12092723197968,13.5408455660964));
#30817=CARTESIAN_POINT('Ctrl Pts',(3.24893058939613,-2.216515063176,13.5349734421304));
#30818=CARTESIAN_POINT('Ctrl Pts',(3.18380233694594,-2.31197896285108,13.5291089314897));
#30819=CARTESIAN_POINT('Ctrl Pts',(3.1143735268679,-2.4047010141651,13.523244420849));
#30820=CARTESIAN_POINT('Ctrl Pts',(3.04090472941863,-2.4942709208503,13.5173799102083));
#30821=CARTESIAN_POINT('Ctrl Pts',(2.96751153063104,-2.5837486609926,13.5115214340907));
#30822=CARTESIAN_POINT('Ctrl Pts',(2.89008687375892,-2.67008039031586,13.5056629579731));
#30823=CARTESIAN_POINT('Ctrl Pts',(2.808934159163,-2.7528853752903,13.4998044818555));
#30824=CARTESIAN_POINT('Ctrl Pts',(2.72458148553266,-2.83895547050886,13.4937149982642));
#30825=CARTESIAN_POINT('Ctrl Pts',(2.63620095757157,-2.92121459513927,13.4876255146729));
#30826=CARTESIAN_POINT('Ctrl Pts',(2.54417916322833,-2.99927347625967,13.4815360310817));
#30827=CARTESIAN_POINT('Ctrl Pts',(2.45575089153234,-3.07428409735508,13.4756843465613));
#30828=CARTESIAN_POINT('Ctrl Pts',(2.36396075026837,-3.14541607190262,13.4698326620409));
#30829=CARTESIAN_POINT('Ctrl Pts',(2.2691881608167,-3.21236269602443,13.4639809775205));
#30830=CARTESIAN_POINT('Ctrl Pts',(2.17443002624507,-3.27929910933079,13.4581301855092));
#30831=CARTESIAN_POINT('Ctrl Pts',(2.07669068551652,-3.34205120300772,13.4522793934979));
#30832=CARTESIAN_POINT('Ctrl Pts',(1.97638025177507,-3.40035440805712,13.4464286014866));
#30833=CARTESIAN_POINT('Ctrl Pts',(1.87606082134031,-3.4586628422341,13.4405772847264));
#30834=CARTESIAN_POINT('Ctrl Pts',(1.77317019693155,-3.51252138682279,13.4347259679663));
#30835=CARTESIAN_POINT('Ctrl Pts',(1.66814427683231,-3.56171077877915,13.4288746512062));
#30836=CARTESIAN_POINT('Ctrl Pts',(1.56308349876767,-3.61091649663032,13.4230213924017));
#30837=CARTESIAN_POINT('Ctrl Pts',(1.4558863899923,-3.65544980514802,13.4171681335972));
#30838=CARTESIAN_POINT('Ctrl Pts',(1.34700939553832,-3.69513933273584,13.4113148747927));
#30839=CARTESIAN_POINT('Ctrl Pts',(1.23800853226577,-3.73487401490308,13.4054549567646));
#30840=CARTESIAN_POINT('Ctrl Pts',(1.12732435725675,-3.76975377516436,13.3995950387365));
#30841=CARTESIAN_POINT('Ctrl Pts',(1.01542916296934,-3.7996569075367,13.3937351207084));
#30842=CARTESIAN_POINT('Ctrl Pts',(0.903458626445167,-3.8295801745439,13.3878712570297));
#30843=CARTESIAN_POINT('Ctrl Pts',(0.790275849736148,-3.85452005260822,
13.3820073933511));
#30844=CARTESIAN_POINT('Ctrl Pts',(0.67636229646865,-3.87440615371126,13.3761435296725));
#30845=CARTESIAN_POINT('Ctrl Pts',(0.562280693322265,-3.89432159159456,
13.3702710153851));
#30846=CARTESIAN_POINT('Ctrl Pts',(0.447466570451588,-3.90916831983204,
13.3643985010977));
#30847=CARTESIAN_POINT('Ctrl Pts',(0.332405560992506,-3.9189278563175,13.3585259868103));
#30848=CARTESIAN_POINT('Ctrl Pts',(0.300605164765652,-3.92162518296783,
13.3569029497618));
#30849=CARTESIAN_POINT('Ctrl Pts',(0.268785901636926,-3.92393423057168,
13.3552799127134));
#30850=CARTESIAN_POINT('Ctrl Pts',(0.236957985811464,-3.92585530973318,
13.3536568756649));
#30851=CARTESIAN_POINT('Ctrl Pts',(0.121805058475212,-3.93280574564309,
13.3477847516989));
#30852=CARTESIAN_POINT('Ctrl Pts',(0.00615301487782126,-3.9346970510376,
13.3419126277329));
#30853=CARTESIAN_POINT('Ctrl Pts',(-0.109516173066837,-3.93147494050729,
13.3360405037669));
#30854=CARTESIAN_POINT('Ctrl Pts',(-0.225035393612344,-3.92825700750727,
13.3301759931262));
#30855=CARTESIAN_POINT('Ctrl Pts',(-0.340571304869079,-3.91993885394681,
13.3243114824855));
#30856=CARTESIAN_POINT('Ctrl Pts',(-0.455637867853506,-3.90651803187671,
13.3184469718449));
#30857=CARTESIAN_POINT('Ctrl Pts',(-0.570586028489416,-3.893111019699,13.3125884957273));
#30858=CARTESIAN_POINT('Ctrl Pts',(-0.685065393316299,-3.87461183030031,
13.3067300196097));
#30859=CARTESIAN_POINT('Ctrl Pts',(-0.798591655524796,-3.85107002893042,
13.3008715434922));
#30860=CARTESIAN_POINT('Ctrl Pts',(-0.916594408634085,-3.826599943148,13.2947820599009));
#30861=CARTESIAN_POINT('Ctrl Pts',(-1.03356689369985,-3.79668140298915,
13.2886925763096));
#30862=CARTESIAN_POINT('Ctrl Pts',(-1.14897266828653,-3.76142935697728,
13.2826030927183));
#30863=CARTESIAN_POINT('Ctrl Pts',(-1.25987175760789,-3.72755393078278,
13.276751408198));
#30864=CARTESIAN_POINT('Ctrl Pts',(-1.36932377014591,-3.68875386908723,
13.2708997236776));
#30865=CARTESIAN_POINT('Ctrl Pts',(-1.47686561295014,-3.64518270615965,
13.2650480391572));
#30866=CARTESIAN_POINT('Ctrl Pts',(-1.58439105328567,-3.60161818878154,
13.259197247146));
#30867=CARTESIAN_POINT('Ctrl Pts',(-1.69000652011402,-3.55328417225649,
13.2533464551347));
#30868=CARTESIAN_POINT('Ctrl Pts',(-1.79326779030938,-3.50038278367365,
13.2474956631234));
#30869=CARTESIAN_POINT('Ctrl Pts',(-1.89653832185428,-3.44747665044406,
13.2416443463633));
#30870=CARTESIAN_POINT('Ctrl Pts',(-1.99745386907008,-3.39000251933692,
13.2357930296032));
#30871=CARTESIAN_POINT('Ctrl Pts',(-2.09559439821346,-3.32820869510558,
13.2299417128431));
#30872=CARTESIAN_POINT('Ctrl Pts',(-2.19376750007045,-3.26639436158458,
13.2240884540386));
#30873=CARTESIAN_POINT('Ctrl Pts',(-2.28916340280131,-3.20025770427893,
13.2182351952341));
#30874=CARTESIAN_POINT('Ctrl Pts',(-2.38139126814028,-3.13009019487063,
13.2123819364296));
#30875=CARTESIAN_POINT('Ctrl Pts',(-2.47372406066531,-3.05984285623405,
13.2065220184015));
#30876=CARTESIAN_POINT('Ctrl Pts',(-2.56288129257795,-2.98555576266533,
13.2006621003734));
#30877=CARTESIAN_POINT('Ctrl Pts',(-2.64850535321555,-2.90756055723497,
13.1948021823454));
#30878=CARTESIAN_POINT('Ctrl Pts',(-2.73418706698361,-2.8295128354007,13.1889383186668));
#30879=CARTESIAN_POINT('Ctrl Pts',(-2.81633058015719,-2.74775232106288,
13.1830744549882));
#30880=CARTESIAN_POINT('Ctrl Pts',(-2.89461650753482,-2.66264610384236,
13.1772105913096));
#30881=CARTESIAN_POINT('Ctrl Pts',(-2.97301792547758,-2.5774143344894,13.1713380770222));
#30882=CARTESIAN_POINT('Ctrl Pts',(-3.04755013455492,-2.48882732663886,
13.1654655627349));
#30883=CARTESIAN_POINT('Ctrl Pts',(-3.11793517238528,-2.39728372555331,
13.1595930484475));
#30884=CARTESIAN_POINT('Ctrl Pts',(-3.13738808786231,-2.37198303680932,
13.1579700113989));
#30885=CARTESIAN_POINT('Ctrl Pts',(-3.15652448380176,-2.34645666696216,
13.1563469743502));
#30886=CARTESIAN_POINT('Ctrl Pts',(-3.17533910233633,-2.32071337850538,
13.1547239373016));
#30887=CARTESIAN_POINT('Ctrl Pts',(-3.24341011310096,-2.22757454274115,
13.1488518133354));
#30888=CARTESIAN_POINT('Ctrl Pts',(-3.30749385624835,-2.13128203997407,
13.1429796893693));
#30889=CARTESIAN_POINT('Ctrl Pts',(-3.36728422133357,-2.03221208852767,
13.1371075654032));
#30890=CARTESIAN_POINT('Ctrl Pts',(-3.42699706702323,-1.93327058324048,
13.1312430547623));
#30891=CARTESIAN_POINT('Ctrl Pts',(-3.48242739266084,-1.83155914106754,
13.1253785441215));
#30892=CARTESIAN_POINT('Ctrl Pts',(-3.53331050837613,-1.72748541278901,
13.1195140334807));
#30893=CARTESIAN_POINT('Ctrl Pts',(-3.58414126587168,-1.62351877534124,
13.113655557363));
#30894=CARTESIAN_POINT('Ctrl Pts',(-3.63043393977614,-1.51719505586621,
13.1077970812453));
#30895=CARTESIAN_POINT('Ctrl Pts',(-3.67196854227613,-1.40894855283454,
13.1019386051276));
#30896=CARTESIAN_POINT('Ctrl Pts',(-3.71514090916976,-1.29643374680412,
13.0958491215363));
#30897=CARTESIAN_POINT('Ctrl Pts',(-3.75317201572699,-1.18184179140842,
13.0897596379451));
#30898=CARTESIAN_POINT('Ctrl Pts',(-3.78586871898737,-1.06568618391762,
13.0836701543539));
#30899=CARTESIAN_POINT('Ctrl Pts',(-3.8172885905535,-0.954066543246762,
13.0778184698334));
#30900=CARTESIAN_POINT('Ctrl Pts',(-3.84378274322947,-0.841003517854998,
13.0719667853129));
#30901=CARTESIAN_POINT('Ctrl Pts',(-3.86523013594268,-0.72696973540895,
13.0661151007924));
#30902=CARTESIAN_POINT('Ctrl Pts',(-3.88667425746228,-0.612953345593541,
13.060264308781));
#30903=CARTESIAN_POINT('Ctrl Pts',(-3.90307307311108,-0.49796689929363,
13.0544135167695));
#30904=CARTESIAN_POINT('Ctrl Pts',(-3.91435662611418,-0.382493403336624,
13.0485627247581));
#30905=CARTESIAN_POINT('Ctrl Pts',(-3.92564119112232,-0.26700955073387,
13.0427114079979));
#30906=CARTESIAN_POINT('Ctrl Pts',(-3.93180954126403,-0.151038973114173,
13.0368600912377));
#30907=CARTESIAN_POINT('Ctrl Pts',(-3.9328436462599,-0.0350692753433018,
13.0310087744774));
#30908=CARTESIAN_POINT('Ctrl Pts',(-3.93387809447388,0.08093891261901,13.0251555156728));
#30909=CARTESIAN_POINT('Ctrl Pts',(-3.9297749054669,0.196945806974127,13.0193022568682));
#30910=CARTESIAN_POINT('Ctrl Pts',(-3.92056814712845,0.312465043999806,
13.0134489980635));
#30911=CARTESIAN_POINT('Ctrl Pts',(-3.91135091430659,0.42811570668989,13.0075890800353));
#30912=CARTESIAN_POINT('Ctrl Pts',(-3.89701855578512,0.543277192321976,
13.0017291620071));
#30913=CARTESIAN_POINT('Ctrl Pts',(-3.8776568957996,0.6574693897497,12.9958692439789));
#30914=CARTESIAN_POINT('Ctrl Pts',(-3.85828219905428,0.771738476052125,
12.9900053803002));
#30915=CARTESIAN_POINT('Ctrl Pts',(-3.83387154477571,0.885036571444755,
12.9841415166214));
#30916=CARTESIAN_POINT('Ctrl Pts',(-3.80456123845042,0.996896575819474,
12.9782776529427));
#30917=CARTESIAN_POINT('Ctrl Pts',(-3.77520769237632,1.10892160059478,12.9724051386552));
#30918=CARTESIAN_POINT('Ctrl Pts',(-3.74094019009118,1.21950390676341,12.9665326243677));
#30919=CARTESIAN_POINT('Ctrl Pts',(-3.70194397204481,1.32819419809044,12.9606601100802));
#30920=CARTESIAN_POINT('Ctrl Pts',(-3.69116625342237,1.3582338643863,12.9590370730328));
#30921=CARTESIAN_POINT('Ctrl Pts',(-3.68002760666876,1.38812914418125,12.9574140359855));
#30922=CARTESIAN_POINT('Ctrl Pts',(-3.66853256383573,1.41787087849241,12.9557909989381));
#30923=CARTESIAN_POINT('Ctrl Pts',(-3.62694366935026,1.52547603212679,12.9499188749722));
#30924=CARTESIAN_POINT('Ctrl Pts',(-3.58054663655935,1.63143020888402,12.9440467510062));
#30925=CARTESIAN_POINT('Ctrl Pts',(-3.52949262520624,1.73527254591743,12.9381746270403));
#30926=CARTESIAN_POINT('Ctrl Pts',(-3.47850480639256,1.83898024929902,12.9323101163997));
#30927=CARTESIAN_POINT('Ctrl Pts',(-3.42287219685505,1.94058119035989,12.926445605759));
#30928=CARTESIAN_POINT('Ctrl Pts',(-3.36279478643395,2.03963237480009,12.9205810951184));
#30929=CARTESIAN_POINT('Ctrl Pts',(-3.30277919507061,2.13858163655672,12.9147226190009));
#30930=CARTESIAN_POINT('Ctrl Pts',(-3.23832811314525,2.23498600895748,12.9088641428834));
#30931=CARTESIAN_POINT('Ctrl Pts',(-3.16968810763422,2.32842571286313,12.9030056667659));
#30932=CARTESIAN_POINT('Ctrl Pts',(-3.09834153578124,2.4255498680696,12.8969161831746));
#30933=CARTESIAN_POINT('Ctrl Pts',(-3.02246909522505,2.51947033480564,12.8908266995833));
#30934=CARTESIAN_POINT('Ctrl Pts',(-2.94239849967909,2.60974712742178,12.884737215992));
#30935=CARTESIAN_POINT('Ctrl Pts',(-2.86545472317267,2.69649854106383,12.8788855314717));
#30936=CARTESIAN_POINT('Ctrl Pts',(-2.78463482136749,2.77988517853167,12.8730338469514));
#30937=CARTESIAN_POINT('Ctrl Pts',(-2.70027107867531,2.85954980751686,12.867182162431));
#30938=CARTESIAN_POINT('Ctrl Pts',(-2.61592020328776,2.9392022859144,12.8613313704198));
#30939=CARTESIAN_POINT('Ctrl Pts',(-2.52802686221723,3.01513360081178,12.8554805784086));
#30940=CARTESIAN_POINT('Ctrl Pts',(-2.43695967661988,3.0870238960087,12.8496297863974));
#30941=CARTESIAN_POINT('Ctrl Pts',(-2.3458843233422,3.15892063893919,12.8437784696373));
#30942=CARTESIAN_POINT('Ctrl Pts',(-2.25163488417316,3.22677538551229,12.8379271528773));
#30943=CARTESIAN_POINT('Ctrl Pts',(-2.15461190761489,3.29030948811265,12.8320758361172));
#30944=CARTESIAN_POINT('Ctrl Pts',(-2.05755672925711,3.35386467759888,12.8262225773128));
#30945=CARTESIAN_POINT('Ctrl Pts',(-1.95772652876357,3.41309614530512,12.8203693185083));
#30946=CARTESIAN_POINT('Ctrl Pts',(-1.85554896141381,3.46776975184283,12.8145160597038));
#30947=CARTESIAN_POINT('Ctrl Pts',(-1.75325514715125,3.52250556027218,12.8086561416758));
#30948=CARTESIAN_POINT('Ctrl Pts',(-1.64860900033829,3.57267296233976,12.8027962236478));
#30949=CARTESIAN_POINT('Ctrl Pts',(-1.54206088150001,3.61808474717597,12.7969363056197));
#30950=CARTESIAN_POINT('Ctrl Pts',(-1.43544102076429,3.66352710906643,12.7910724419412));
#30951=CARTESIAN_POINT('Ctrl Pts',(-1.32691702413892,3.7042073329776,12.7852085782626));
#30952=CARTESIAN_POINT('Ctrl Pts',(-1.21695558154691,3.73998771556028,12.7793447145841));
#30953=CARTESIAN_POINT('Ctrl Pts',(-1.10683191938939,3.77582088280985,12.7734722002968));
#30954=CARTESIAN_POINT('Ctrl Pts',(-0.995266975889134,3.80673967210187,
12.7675996860095));
#30955=CARTESIAN_POINT('Ctrl Pts',(-0.882738901942349,3.83265717629396,
12.7617271717222));
#30956=CARTESIAN_POINT('Ctrl Pts',(-0.851638554773166,3.83982021881182,
12.760104134673));
#30957=CARTESIAN_POINT('Ctrl Pts',(-0.820464673745179,3.84660154238882,
12.7584810976238));
#30958=CARTESIAN_POINT('Ctrl Pts',(-0.789227414493501,3.85300001144717,
12.7568580605746));
#30959=CARTESIAN_POINT('Ctrl Pts',(-0.676211473933424,3.8761495775774,12.7509859366088));
#30960=CARTESIAN_POINT('Ctrl Pts',(-0.561986667712901,3.89436127347583,
12.7451138126429));
#30961=CARTESIAN_POINT('Ctrl Pts',(-0.447022463926352,3.90751326507604,
12.7392416886771));
#30962=CARTESIAN_POINT('Ctrl Pts',(-0.332207313512615,3.92064820485801,
12.7333771780365));
#30963=CARTESIAN_POINT('Ctrl Pts',(-0.216655078864421,3.92873643926183,
12.727512667396));
#30964=CARTESIAN_POINT('Ctrl Pts',(-0.100846577966071,3.93170687713524,
12.7216481567555));
#30965=CARTESIAN_POINT('Ctrl Pts',(0.0148427571372789,3.93467425845763,
12.715789680638));
#30966=CARTESIAN_POINT('Ctrl Pts',(0.130787423199741,3.93253430735893,12.7099312045206));
#30967=CARTESIAN_POINT('Ctrl Pts',(0.246500968593963,3.92526766889625,12.7040727284031));
#30968=CARTESIAN_POINT('Ctrl Pts',(0.366777252365796,3.91771449725306,12.6979832448118));
#30969=CARTESIAN_POINT('Ctrl Pts',(0.486803361598573,3.90462196463276,12.6918937612205));
#30970=CARTESIAN_POINT('Ctrl Pts',(0.606031994606799,3.8860280778081,12.6858042776291));
#30971=CARTESIAN_POINT('Ctrl Pts',(0.720604656750912,3.86816029672769,12.6799525931089));
#30972=CARTESIAN_POINT('Ctrl Pts',(0.83444051104996,3.84521283256345,12.6741009085887));
#30973=CARTESIAN_POINT('Ctrl Pts',(0.94705941817337,3.81727225364515,12.6682492240685));
#30974=CARTESIAN_POINT('Ctrl Pts',(1.05966114846559,3.78933593627244,12.6623984320573));
#30975=CARTESIAN_POINT('Ctrl Pts',(1.17104589949739,3.75640811788417,12.6565476400462));
#30976=CARTESIAN_POINT('Ctrl Pts',(1.28074534728091,3.71862613816155,12.650696848035));
#30977=CARTESIAN_POINT('Ctrl Pts',(1.39045463384457,3.68084076982942,12.6448455312751));
#30978=CARTESIAN_POINT('Ctrl Pts',(1.49847792578075,3.63820050933438,12.6389942145151));
#30979=CARTESIAN_POINT('Ctrl Pts',(1.60436432185904,3.59089182832702,12.6331428977551));
#30980=CARTESIAN_POINT('Ctrl Pts',(1.71028586149414,3.54356744563012,12.6272896389508));
#30981=CARTESIAN_POINT('Ctrl Pts',(1.81406871775506,3.49157173000692,12.6214363801464));
#30982=CARTESIAN_POINT('Ctrl Pts',(1.91528479340871,3.43513801180351,12.615583121342));
#30983=CARTESIAN_POINT('Ctrl Pts',(2.01661602209066,3.37864008923822,12.6097232033141));
#30984=CARTESIAN_POINT('Ctrl Pts',(2.11537428020042,3.31769428767874,12.6038632852862));
#30985=CARTESIAN_POINT('Ctrl Pts',(2.21115868939502,3.25257840033302,12.5980033672582));
#30986=CARTESIAN_POINT('Ctrl Pts',(2.30700759297325,3.18741866859702,12.5921395035798));
#30987=CARTESIAN_POINT('Ctrl Pts',(2.39987833004557,3.11808350683748,12.5862756399013));
#30988=CARTESIAN_POINT('Ctrl Pts',(2.48940285641362,3.04489119977705,12.5804117762229));
#30989=CARTESIAN_POINT('Ctrl Pts',(2.57905945298267,2.97159091646589,12.5745392619357));
#30990=CARTESIAN_POINT('Ctrl Pts',(2.66535967955664,2.89442240577341,12.5686667476485));
#30991=CARTESIAN_POINT('Ctrl Pts',(2.74797204107872,2.81374104377955,12.5627942333612));
#30992=CARTESIAN_POINT('Ctrl Pts',(2.77080432670303,2.79144244502676,12.5611711963112));
#30993=CARTESIAN_POINT('Ctrl Pts',(2.79335515190305,2.76887571084539,12.5595481592612));
#30994=CARTESIAN_POINT('Ctrl Pts',(2.81561807358169,2.74604877300461,12.5579251222112));
#30995=CARTESIAN_POINT('Ctrl Pts',(2.89510692602653,2.66454612389213,12.5521301347229));
#30996=CARTESIAN_POINT('Ctrl Pts',(2.97120448473133,2.57943463234707,12.5463351472347));
#30997=CARTESIAN_POINT('Ctrl Pts',(3.04355847766435,2.49103207386767,12.5405401597464));
#30998=CARTESIAN_POINT('Ctrl Pts',(3.11579673760803,2.40277091867429,12.5347544415631));
#30999=CARTESIAN_POINT('Ctrl Pts',(3.1843030788273,2.31122949608834,12.5289687233797));
#31000=CARTESIAN_POINT('Ctrl Pts',(3.2487616329008,2.2167626964995,12.5231830051964));
#31001=CARTESIAN_POINT('Ctrl Pts',(3.31316125215976,2.12238226843098,12.5174025769274));
#31002=CARTESIAN_POINT('Ctrl Pts',(3.37352019869514,2.02508212588218,12.5116221486584));
#31003=CARTESIAN_POINT('Ctrl Pts',(3.4295626798161,1.92525032793469,12.5058417203894));
#31004=CARTESIAN_POINT('Ctrl Pts',(3.48556834691289,1.82548410899349,12.5000650892546));
#31005=CARTESIAN_POINT('Ctrl Pts',(3.53726297594805,1.72318990900058,12.4942884581199));
#31006=CARTESIAN_POINT('Ctrl Pts',(3.5844144405252,1.61878414822805,12.4885118269852));
#31007=CARTESIAN_POINT('Ctrl Pts',(3.63154706468069,1.51442010511106,12.4827375040325));
#31008=CARTESIAN_POINT('Ctrl Pts',(3.67413995891684,1.4079465657574,12.4769631810799));
#31009=CARTESIAN_POINT('Ctrl Pts',(3.71200766077777,1.29980311060067,12.4711888581273));
#31010=CARTESIAN_POINT('Ctrl Pts',(3.7498829308237,1.19163804204688,12.4654133811267));
#31011=CARTESIAN_POINT('Ctrl Pts',(3.78303097079323,1.08180278889257,12.4596379041261));
#31012=CARTESIAN_POINT('Ctrl Pts',(3.81131521201403,0.97075504359772,12.4538624271255));
#31013=CARTESIAN_POINT('Ctrl Pts',(3.83960129040054,0.859700085342571,12.4480865749863));
#31014=CARTESIAN_POINT('Ctrl Pts',(3.8630228446412,0.747432892764753,12.4423107228472));
#31015=CARTESIAN_POINT('Ctrl Pts',(3.88149410410307,0.634422981781957,12.4365348707081));
#31016=CARTESIAN_POINT('Ctrl Pts',(3.89998219168447,0.521310113862548,12.4307537565168));
#31017=CARTESIAN_POINT('Ctrl Pts',(3.91351091543769,0.407453597623295,12.4249726423256));
#31018=CARTESIAN_POINT('Ctrl Pts',(3.92204623846465,0.293329683709804,12.4191915281344));
#31019=CARTESIAN_POINT('Ctrl Pts',(3.929442095749,0.194441313888272,12.4141821927679));
#31020=CARTESIAN_POINT('Ctrl Pts',(3.93308962003901,0.0953524250593562,
12.4091728574014));
#31021=CARTESIAN_POINT('Ctrl Pts',(3.93299832708652,-0.00362755215277343,
12.404163522035));
#31022=CARTESIAN_POINT('',(3.93443448987282,0.00134968955162095,11.154163522035));
#31023=CARTESIAN_POINT('Ctrl Pts',(3.93324003457201,-0.00362777508866888,
12.404163522035));
#31024=CARTESIAN_POINT('Ctrl Pts',(3.93600258766685,-0.301163912932759,
12.3891064093059));
#31025=CARTESIAN_POINT('Ctrl Pts',(3.7690722733079,-1.90596907523995,12.3077383171222));
#31026=CARTESIAN_POINT('Ctrl Pts',(1.56812889849248,-4.38010354283667,12.1600592454845));
#31027=CARTESIAN_POINT('Ctrl Pts',(-2.83826737299349,-3.68626824908905,
11.9611263071209));
#31028=CARTESIAN_POINT('Ctrl Pts',(-4.6354315863291,0.396370150380956,11.7621933687574));
#31029=CARTESIAN_POINT('Ctrl Pts',(-2.17122253533752,4.11462367616172,11.563260430394));
#31030=CARTESIAN_POINT('Ctrl Pts',(2.28900123116229,4.05028500649437,11.3643274920306));
#31031=CARTESIAN_POINT('Ctrl Pts',(3.90396011105411,1.45381414440226,11.2279618559109));
#31032=CARTESIAN_POINT('Ctrl Pts',(3.93929569899745,0.0750487185641683,
11.1579071992457));
#31033=CARTESIAN_POINT('Ctrl Pts',(3.93896841652295,0.00135124489418437,
11.154163522035));
#31034=CARTESIAN_POINT('',(3.9329988605794,0.00299377372986385,9.90416352208001));
#31035=CARTESIAN_POINT('Ctrl Pts',(3.93299976858205,0.00134919737711916,
11.154163522035));
#31036=CARTESIAN_POINT('Ctrl Pts',(3.93303902141628,-0.113075415770322,
11.1483421609502));
#31037=CARTESIAN_POINT('Ctrl Pts',(3.92808052764153,-0.227703811320846,
11.1425207998654));
#31038=CARTESIAN_POINT('Ctrl Pts',(3.91809711475004,-0.342058473637813,
11.1366994387805));
#31039=CARTESIAN_POINT('Ctrl Pts',(3.90812625842716,-0.456269307168048,
11.1308853994724));
#31040=CARTESIAN_POINT('Ctrl Pts',(3.89314308324188,-0.570206676261325,
11.1250713601643));
#31041=CARTESIAN_POINT('Ctrl Pts',(3.87317241100323,-0.683391889506635,
11.1192573208562));
#31042=CARTESIAN_POINT('Ctrl Pts',(3.85322128602432,-0.796466317259319,
11.1134489723197));
#31043=CARTESIAN_POINT('Ctrl Pts',(3.82829244368335,-0.908789640732537,
11.1076406237833));
#31044=CARTESIAN_POINT('Ctrl Pts',(3.79846254146286,-1.0198878963413,11.1018322752469));
#31045=CARTESIAN_POINT('Ctrl Pts',(3.76865229567981,-1.13091294366752,11.0960277541263));
#31046=CARTESIAN_POINT('Ctrl Pts',(3.73394752017707,-1.24071412274453,11.0902232330057));
#31047=CARTESIAN_POINT('Ctrl Pts',(3.69447588432086,-1.34882798761429,11.0844187118851));
#31048=CARTESIAN_POINT('Ctrl Pts',(3.6550175900138,-1.45690530962457,11.0786161527127));
#31049=CARTESIAN_POINT('Ctrl Pts',(3.61079578151708,-1.56329605565847,11.0728135935403));
#31050=CARTESIAN_POINT('Ctrl Pts',(3.56198766662226,-1.6675529565297,11.0670110343678));
#31051=CARTESIAN_POINT('Ctrl Pts',(3.51318373164055,-1.7718009288695,11.0612089721249));
#31052=CARTESIAN_POINT('Ctrl Pts',(3.45979444978325,-1.87391503802175,11.055406909882));
#31053=CARTESIAN_POINT('Ctrl Pts',(3.40204441479229,-1.9734697362211,11.0496048476391));
#31054=CARTESIAN_POINT('Ctrl Pts',(3.34428475092241,-2.07304103354693,11.0438018179967));
#31055=CARTESIAN_POINT('Ctrl Pts',(3.28216310060605,-2.1700517077837,11.0379987883543));
#31056=CARTESIAN_POINT('Ctrl Pts',(3.21594865601709,-2.26410318710563,11.0321957587119));
#31057=CARTESIAN_POINT('Ctrl Pts',(3.14966538352637,-2.35825243008048,11.0263866969967));
#31058=CARTESIAN_POINT('Ctrl Pts',(3.07928106441321,-2.44943599100851,11.0205776352814));
#31059=CARTESIAN_POINT('Ctrl Pts',(3.00510669561318,-2.53728649308289,11.0147685735661));
#31060=CARTESIAN_POINT('Ctrl Pts',(2.930891994425,-2.62518476395672,11.0089563531677));
#31061=CARTESIAN_POINT('Ctrl Pts',(2.85288342588868,-2.70974605839912,11.0031441327693));
#31062=CARTESIAN_POINT('Ctrl Pts',(2.77142922418866,-2.79063954234742,10.9973319123708));
#31063=CARTESIAN_POINT('Ctrl Pts',(2.68984406177454,-2.87166308549714,10.9915103471808));
#31064=CARTESIAN_POINT('Ctrl Pts',(2.60480251344148,-2.94900675745116,10.9856887819908));
#31065=CARTESIAN_POINT('Ctrl Pts',(2.51668652332082,-3.02237951676082,10.9798672168009));
#31066=CARTESIAN_POINT('Ctrl Pts',(2.4490501969759,-3.07869919139308,10.9753986829685));
#31067=CARTESIAN_POINT('Ctrl Pts',(2.37960315685819,-3.13268008654891,10.9709301491361));
#31068=CARTESIAN_POINT('Ctrl Pts',(2.30852895187917,-3.1842083911603,10.9664616153037));
#31069=CARTESIAN_POINT('Ctrl Pts',(2.21512996297312,-3.25192200895128,10.960589491346));
#31070=CARTESIAN_POINT('Ctrl Pts',(2.11859260878961,-3.31563630408311,10.9547173673882));
#31071=CARTESIAN_POINT('Ctrl Pts',(2.01929427785213,-3.37504660996461,10.9488452434304));
#31072=CARTESIAN_POINT('Ctrl Pts',(1.92012468918109,-3.43437988919968,10.9429807327985));
#31073=CARTESIAN_POINT('Ctrl Pts',(1.81820159388882,-3.48942006589947,10.9371162221665));
#31074=CARTESIAN_POINT('Ctrl Pts',(1.7139336540081,-3.53990401418717,10.9312517115346));
#31075=CARTESIAN_POINT('Ctrl Pts',(1.60977300480953,-3.59033601498981,10.9253932354263));
#31076=CARTESIAN_POINT('Ctrl Pts',(1.50327268009245,-3.63622093358657,10.9195347593179));
#31077=CARTESIAN_POINT('Ctrl Pts',(1.39486781809373,-3.67734044793876,10.9136762832096));
#31078=CARTESIAN_POINT('Ctrl Pts',(1.28218840855007,-3.72008135930103,10.9075867996151));
#31079=CARTESIAN_POINT('Ctrl Pts',(1.16745156535847,-3.75767308877496,10.9014973160205));
#31080=CARTESIAN_POINT('Ctrl Pts',(1.05117152211228,-3.78992446245307,10.8954078324259));
#31081=CARTESIAN_POINT('Ctrl Pts',(0.939432305261353,-3.82091639483073,
10.889556147916));
#31082=CARTESIAN_POINT('Ctrl Pts',(0.826268588841986,-3.84697711368719,
10.883704463406));
#31083=CARTESIAN_POINT('Ctrl Pts',(0.71215346085846,-3.86798738986922,10.877852778896));
#31084=CARTESIAN_POINT('Ctrl Pts',(0.598055737920354,-3.88899446152599,
10.8720019868955));
#31085=CARTESIAN_POINT('Ctrl Pts',(0.483007298411011,-3.90495254727477,
10.8661511948951));
#31086=CARTESIAN_POINT('Ctrl Pts',(0.367491413672845,-3.91579354165624,
10.8603004028946));
#31087=CARTESIAN_POINT('Ctrl Pts',(0.251965168494878,-3.92663550834962,
10.8544490861457));
#31088=CARTESIAN_POINT('Ctrl Pts',(0.135971806374681,-3.93235943270659,
10.8485977693968));
#31089=CARTESIAN_POINT('Ctrl Pts',(0.019998997685629,-3.93294915300104,
10.8427464526479));
#31090=CARTESIAN_POINT('Ctrl Pts',(-0.0960123022194861,-3.93353906902284,
10.836893193855));
#31091=CARTESIAN_POINT('Ctrl Pts',(-0.21200262194024,-3.92899139051807,
10.8310399350621));
#31092=CARTESIAN_POINT('Ctrl Pts',(-0.327485731869154,-3.91934204879111,
10.8251866762692));
#31093=CARTESIAN_POINT('Ctrl Pts',(-0.443100226351587,-3.9096817290566,
10.8193267582531));
#31094=CARTESIAN_POINT('Ctrl Pts',(-0.558205947042739,-3.89490819564083,
10.8134668402371));
#31095=CARTESIAN_POINT('Ctrl Pts',(-0.672323115186839,-3.87510911185549,
10.8076069222211));
#31096=CARTESIAN_POINT('Ctrl Pts',(-0.786517121680261,-3.85529669678144,
10.8017430585549));
#31097=CARTESIAN_POINT('Ctrl Pts',(-0.899720847428843,-3.83045208184253,
10.7958791948887));
#31098=CARTESIAN_POINT('Ctrl Pts',(-1.01146771805528,-3.80071336137468,
10.7900153312225));
#31099=CARTESIAN_POINT('Ctrl Pts',(-1.12337944217693,-3.77093076914573,
10.7841428169479));
#31100=CARTESIAN_POINT('Ctrl Pts',(-1.23382962881059,-3.73623978506127,
10.7782703026733));
#31101=CARTESIAN_POINT('Ctrl Pts',(-1.34236969483216,-3.69682736983974,
10.7723977883986));
#31102=CARTESIAN_POINT('Ctrl Pts',(-1.3723678440887,-3.68593462250954,10.7707747512458));
#31103=CARTESIAN_POINT('Ctrl Pts',(-1.40222022486759,-3.67468150291626,
10.769151714093));
#31104=CARTESIAN_POINT('Ctrl Pts',(-1.4319176956174,-3.66307257817502,10.7675286769402));
#31105=CARTESIAN_POINT('Ctrl Pts',(-1.53936270136931,-3.62107166179718,
10.7616565527553));
#31106=CARTESIAN_POINT('Ctrl Pts',(-1.64513831813272,-3.57426896836526,
10.7557844285705));
#31107=CARTESIAN_POINT('Ctrl Pts',(-1.7487842656419,-3.52281742249628,10.7499123043856));
#31108=CARTESIAN_POINT('Ctrl Pts',(-1.85229583414077,-3.47143258456889,
10.7440477935253));
#31109=CARTESIAN_POINT('Ctrl Pts',(-1.95368285745297,-3.41541106249665,
10.738183282665));
#31110=CARTESIAN_POINT('Ctrl Pts',(-2.05250311084,-3.35495454216479,10.7323187718047));
#31111=CARTESIAN_POINT('Ctrl Pts',(-2.15122167918183,-3.29456023098329,
10.7264602954669));
#31112=CARTESIAN_POINT('Ctrl Pts',(-2.24737838050312,-3.22974021314422,
10.7206018191292));
#31113=CARTESIAN_POINT('Ctrl Pts',(-2.34055438353376,-3.16074266236922,
10.7147433427915));
#31114=CARTESIAN_POINT('Ctrl Pts',(-2.43740443483996,-3.08902445043473,
10.7086538592825));
#31115=CARTESIAN_POINT('Ctrl Pts',(-2.5310334788226,-3.01279267924939,10.7025643757736));
#31116=CARTESIAN_POINT('Ctrl Pts',(-2.62100278885694,-2.932376746055,10.6964748922647));
#31117=CARTESIAN_POINT('Ctrl Pts',(-2.70745873177258,-2.85510111365204,
10.6906232075242));
#31118=CARTESIAN_POINT('Ctrl Pts',(-2.79053507025231,-2.77396227746486,
10.6847715227838));
#31119=CARTESIAN_POINT('Ctrl Pts',(-2.86987584785386,-2.68929388834784,
10.6789198380434));
#31120=CARTESIAN_POINT('Ctrl Pts',(-2.94920452425714,-2.60463841300601,
10.6730690458124));
#31121=CARTESIAN_POINT('Ctrl Pts',(-3.02479849002867,-2.51645475669091,
10.6672182535815));
#31122=CARTESIAN_POINT('Ctrl Pts',(-3.09633930379688,-2.42511276351486,
10.6613674613506));
#31123=CARTESIAN_POINT('Ctrl Pts',(-3.16788653394604,-2.33376257802181,
10.6555161443714));
#31124=CARTESIAN_POINT('Ctrl Pts',(-3.23537963451814,-2.23925381804811,
10.6496648273923));
#31125=CARTESIAN_POINT('Ctrl Pts',(-3.29854149476455,-2.14198809691288,
10.6438135104132));
#31126=CARTESIAN_POINT('Ctrl Pts',(-3.36172431834001,-2.04469009342704,
10.6379602513906));
#31127=CARTESIAN_POINT('Ctrl Pts',(-3.42057281811699,-1.94463365583845,
10.6321069923679));
#31128=CARTESIAN_POINT('Ctrl Pts',(-3.47485449511554,-1.84224733349659,
10.6262537333452));
#31129=CARTESIAN_POINT('Ctrl Pts',(-3.5291979280851,-1.7397445267883,10.6203938151014));
#31130=CARTESIAN_POINT('Ctrl Pts',(-3.57896397413598,-1.63490691007829,
10.6145338968575));
#31131=CARTESIAN_POINT('Ctrl Pts',(-3.62396714946527,-1.52818555797279,
10.6086739786136));
#31132=CARTESIAN_POINT('Ctrl Pts',(-3.66900062671078,-1.42139234734957,
10.6028101147203));
#31133=CARTESIAN_POINT('Ctrl Pts',(-3.70926470424461,-1.31271326246949,
10.5969462508271));
#31134=CARTESIAN_POINT('Ctrl Pts',(-3.74462346799198,-1.20261551751327,
10.5910823869338));
#31135=CARTESIAN_POINT('Ctrl Pts',(-3.78003439439521,-1.09235535198087,
10.5852098724351));
#31136=CARTESIAN_POINT('Ctrl Pts',(-3.81052545579805,-0.980672746727933,
10.5793373579364));
#31137=CARTESIAN_POINT('Ctrl Pts',(-3.83601157787593,-0.868046182182596,
10.5734648434377));
#31138=CARTESIAN_POINT('Ctrl Pts',(-3.84305538627748,-0.836918655634727,
10.5718418084841));
#31139=CARTESIAN_POINT('Ctrl Pts',(-3.84971719775555,-0.805719058641991,
10.5702187735305));
#31140=CARTESIAN_POINT('Ctrl Pts',(-3.85599591565923,-0.774457551076468,
10.5685957385768));
#31141=CARTESIAN_POINT('Ctrl Pts',(-3.87871225158276,-0.661353742587398,
10.5627236150339));
#31142=CARTESIAN_POINT('Ctrl Pts',(-3.89648612205457,-0.547059998442666,
10.5568514914909));
#31143=CARTESIAN_POINT('Ctrl Pts',(-3.90919749281048,-0.432046250075409,
10.550979367948));
#31144=CARTESIAN_POINT('Ctrl Pts',(-3.92189238302123,-0.317181619321923,
10.5451148577301));
#31145=CARTESIAN_POINT('Ctrl Pts',(-3.92953778120365,-0.201599247850998,
10.5392503475122));
#31146=CARTESIAN_POINT('Ctrl Pts',(-3.93206443912526,-0.0857802224674986,
10.5333858372943));
#31147=CARTESIAN_POINT('Ctrl Pts',(-3.93458849714113,0.0299196262972318,
10.5275273615987));
#31148=CARTESIAN_POINT('Ctrl Pts',(-3.93200428251064,0.145855233786871,
10.5216688859032));
#31149=CARTESIAN_POINT('Ctrl Pts',(-3.9242943044177,0.261540077836615,10.5158104102076));
#31150=CARTESIAN_POINT('Ctrl Pts',(-3.91628031088973,0.381786540319882,
10.5097209264578));
#31151=CARTESIAN_POINT('Ctrl Pts',(-3.90272795529233,0.501761604293995,
10.5036314427081));
#31152=CARTESIAN_POINT('Ctrl Pts',(-3.88367734128387,0.620918117627617,
10.4975419589583));
#31153=CARTESIAN_POINT('Ctrl Pts',(-3.86537067035357,0.735421465279937,
10.4916902748555));
#31154=CARTESIAN_POINT('Ctrl Pts',(-3.8419871775853,0.849168546146305,10.4858385907527));
#31155=CARTESIAN_POINT('Ctrl Pts',(-3.81361527047577,0.961679556190125,
10.4799869066499));
#31156=CARTESIAN_POINT('Ctrl Pts',(-3.78524769068778,1.07417340590292,10.4741361150538));
#31157=CARTESIAN_POINT('Ctrl Pts',(-3.75189331040411,1.18543115889112,10.4682853234577));
#31158=CARTESIAN_POINT('Ctrl Pts',(-3.71369126282571,1.29498502092185,10.4624345318617));
#31159=CARTESIAN_POINT('Ctrl Pts',(-3.67548578894442,1.40454870872733,10.4565832155141));
#31160=CARTESIAN_POINT('Ctrl Pts',(-3.63243191959001,1.51240781139919,10.4507318991664));
#31161=CARTESIAN_POINT('Ctrl Pts',(-3.58471785281063,1.61811214560078,10.4448805828188));
#31162=CARTESIAN_POINT('Ctrl Pts',(-3.53698794976742,1.72385156299349,10.4390273244236));
#31163=CARTESIAN_POINT('Ctrl Pts',(-3.48459494375123,1.82743441325059,10.4331740660283));
#31164=CARTESIAN_POINT('Ctrl Pts',(-3.42777380377962,1.92843349642195,10.4273208076331));
#31165=CARTESIAN_POINT('Ctrl Pts',(-3.37088801860775,2.02954748587576,10.4214608900075));
#31166=CARTESIAN_POINT('Ctrl Pts',(-3.30956424684825,2.12807148047396,10.4156009723818));
#31167=CARTESIAN_POINT('Ctrl Pts',(-3.24408181575473,2.22360566933291,10.4097410547562));
#31168=CARTESIAN_POINT('Ctrl Pts',(-3.17855529342486,2.3192041841558,10.4038771914767));
#31169=CARTESIAN_POINT('Ctrl Pts',(-3.10886478410271,2.41180855519888,10.3980133281971));
#31170=CARTESIAN_POINT('Ctrl Pts',(-3.03532998044183,2.50105196064196,10.3921494649175));
#31171=CARTESIAN_POINT('Ctrl Pts',(-2.96168669515644,2.59042702169731,10.3862769510211));
#31172=CARTESIAN_POINT('Ctrl Pts',(-2.88418807245217,2.67643091546318,10.3804044371246));
#31173=CARTESIAN_POINT('Ctrl Pts',(-2.80319075601463,2.75873351112319,10.3745319232282));
#31174=CARTESIAN_POINT('Ctrl Pts',(-2.78080477818912,2.78148024104539,10.3729088822232));
#31175=CARTESIAN_POINT('Ctrl Pts',(-2.75815174411362,2.80394448378567,10.3712858412183));
#31176=CARTESIAN_POINT('Ctrl Pts',(-2.73523961024742,2.82611982664103,10.3696628002134));
#31177=CARTESIAN_POINT('Ctrl Pts',(-2.65234405084114,2.90634969356468,10.3637906761752));
#31178=CARTESIAN_POINT('Ctrl Pts',(-2.56577657936873,2.98306374184479,10.357918552137));
#31179=CARTESIAN_POINT('Ctrl Pts',(-2.47586775560022,3.05590704321632,10.3520464280989));
#31180=CARTESIAN_POINT('Ctrl Pts',(-2.38607550045775,3.1286559017601,10.3461819173894));
#31181=CARTESIAN_POINT('Ctrl Pts',(-2.29295082630594,3.19754373553336,10.34031740668));
#31182=CARTESIAN_POINT('Ctrl Pts',(-2.19686112162668,3.26225232198326,10.3344528959705));
#31183=CARTESIAN_POINT('Ctrl Pts',(-2.10087029235316,3.32689432390404,10.3285944197876));
#31184=CARTESIAN_POINT('Ctrl Pts',(-2.00192084195665,3.38736540268395,10.3227359436048));
#31185=CARTESIAN_POINT('Ctrl Pts',(-1.90041269945998,3.44338794964076,10.3168774674219));
#31186=CARTESIAN_POINT('Ctrl Pts',(-1.79490195806552,3.50161953893827,10.3107879838564));
#31187=CARTESIAN_POINT('Ctrl Pts',(-1.68662694166444,3.55504426961796,10.3046985002909));
#31188=CARTESIAN_POINT('Ctrl Pts',(-1.57606971675418,3.60340023421357,10.2986090167254));
#31189=CARTESIAN_POINT('Ctrl Pts',(-1.46982983599936,3.64986786142284,10.2927573321486));
#31190=CARTESIAN_POINT('Ctrl Pts',(-1.36148306030609,3.69165499076689,10.2869056475718));
#31191=CARTESIAN_POINT('Ctrl Pts',(-1.25148088769395,3.7285767509516,10.2810539629951));
#31192=CARTESIAN_POINT('Ctrl Pts',(-1.1414954928675,3.76549287974408,10.2752031709308));
#31193=CARTESIAN_POINT('Ctrl Pts',(-1.02985559495821,3.79754498334782,10.2693523788665));
#31194=CARTESIAN_POINT('Ctrl Pts',(-0.917029995956315,3.82459736266661,
10.2635015868022));
#31195=CARTESIAN_POINT('Ctrl Pts',(-0.804194277859957,3.8516521682573,10.2576502699924));
#31196=CARTESIAN_POINT('Ctrl Pts',(-0.690173049312679,3.87370626175716,
10.2517989531827));
#31197=CARTESIAN_POINT('Ctrl Pts',(-0.575446805842531,3.89067474529106,
10.245947636373));
#31198=CARTESIAN_POINT('Ctrl Pts',(-0.460682484949947,3.90764886063243,
10.2400943775223));
#31199=CARTESIAN_POINT('Ctrl Pts',(-0.345213092601965,3.9195339492648,10.2342411186716));
#31200=CARTESIAN_POINT('Ctrl Pts',(-0.229525057735885,3.92629688738273,
10.228387859821));
#31201=CARTESIAN_POINT('Ctrl Pts',(-0.113705405270288,3.93306751965574,
10.222527941752));
#31202=CARTESIAN_POINT('Ctrl Pts',(0.00233297325410128,3.93470434585651,
10.216668023683));
#31203=CARTESIAN_POINT('Ctrl Pts',(0.11810272632928,3.93122636667409,10.210808105614));
#31204=CARTESIAN_POINT('Ctrl Pts',(0.233950430432206,3.92774604567057,10.2049442418976));
#31205=CARTESIAN_POINT('Ctrl Pts',(0.349528737665922,3.91914409232972,10.1990803781811));
#31206=CARTESIAN_POINT('Ctrl Pts',(0.464356243540799,3.90549129804237,10.1932165144646));
#31207=CARTESIAN_POINT('Ctrl Pts',(0.579353147501274,3.89181836261203,10.1873440001441));
#31208=CARTESIAN_POINT('Ctrl Pts',(0.693596633081365,3.8730797816868,10.1814714858236));
#31209=CARTESIAN_POINT('Ctrl Pts',(0.806616202723852,3.84939726470305,10.1755989715031));
#31210=CARTESIAN_POINT('Ctrl Pts',(0.837852379002223,3.84285192678007,10.173975934952));
#31211=CARTESIAN_POINT('Ctrl Pts',(0.868995162505947,3.83592923731664,10.172352898401));
#31212=CARTESIAN_POINT('Ctrl Pts',(0.90003485814385,3.82863242609237,10.1707298618499));
#31213=CARTESIAN_POINT('Ctrl Pts',(1.01233607784,3.80223265690853,10.1648577364779));
#31214=CARTESIAN_POINT('Ctrl Pts',(1.12366304891352,3.77084342048896,10.158985611106));
#31215=CARTESIAN_POINT('Ctrl Pts',(1.23353850249376,3.73455107916138,10.153113485734));
#31216=CARTESIAN_POINT('Ctrl Pts',(1.34327150051455,3.69830579152614,10.1472489736813));
#31217=CARTESIAN_POINT('Ctrl Pts',(1.45155633457245,3.65717016914594,10.1413844616285));
#31218=CARTESIAN_POINT('Ctrl Pts',(1.55792672122676,3.61128139741112,10.1355199495758));
#31219=CARTESIAN_POINT('Ctrl Pts',(1.66418765391786,3.56543984471999,10.1296614720417));
#31220=CARTESIAN_POINT('Ctrl Pts',(1.76853768021067,3.51485503375725,10.1238029945077));
#31221=CARTESIAN_POINT('Ctrl Pts',(1.87052710768258,3.45971347649262,10.1179445169737));
#31222=CARTESIAN_POINT('Ctrl Pts',(1.97653807853306,3.40239763342211,10.1118550339117));
#31223=CARTESIAN_POINT('Ctrl Pts',(2.07999802714273,3.34015843987668,10.1057655508497));
#31224=CARTESIAN_POINT('Ctrl Pts',(2.18042609039876,3.27326000560731,10.0996760677878));
#31225=CARTESIAN_POINT('Ctrl Pts',(2.27693239144998,3.2089739860612,10.0938243818489));
#31226=CARTESIAN_POINT('Ctrl Pts',(2.37063878019018,3.14038603900235,10.08797269591));
#31227=CARTESIAN_POINT('Ctrl Pts',(2.46114573213632,3.06777617912181,10.0821210099711));
#31228=CARTESIAN_POINT('Ctrl Pts',(2.55163887978295,2.99517739384085,10.076270216543));
#31229=CARTESIAN_POINT('Ctrl Pts',(2.63893323852493,2.91855817405838,10.0704194231148));
#31230=CARTESIAN_POINT('Ctrl Pts',(2.72266130926682,2.83823966483126,10.0645686296867));
#31231=CARTESIAN_POINT('Ctrl Pts',(2.80639688940836,2.75791395200112,10.0587173115128));
#31232=CARTESIAN_POINT('Ctrl Pts',(2.88656524735549,2.673888576381,10.0528659933389));
#31233=CARTESIAN_POINT('Ctrl Pts',(2.96283531171061,2.58652197278134,10.0470146751651));
#31234=CARTESIAN_POINT('Ctrl Pts',(3.03913068993416,2.49912637239602,10.0411614149514));
#31235=CARTESIAN_POINT('Ctrl Pts',(3.1115249301235,2.40838765023391,10.0353081547378));
#31236=CARTESIAN_POINT('Ctrl Pts',(3.17972731964458,2.3146972097244,10.0294548945242));
#31237=CARTESIAN_POINT('Ctrl Pts',(3.24800730250562,2.22090017831311,10.0235949751009));
#31238=CARTESIAN_POINT('Ctrl Pts',(3.31208567237586,2.12414506021348,10.0177350556776));
#31239=CARTESIAN_POINT('Ctrl Pts',(3.37171507784118,2.02485220049723,10.0118751362543));
#31240=CARTESIAN_POINT('Ctrl Pts',(3.43138463341719,1.92549248418099,10.0060112711869));
#31241=CARTESIAN_POINT('Ctrl Pts',(3.48659906327221,1.8235919864264,10.0001474061195));
#31242=CARTESIAN_POINT('Ctrl Pts',(3.53715780830981,1.71959403322788,9.99428354105211));
#31243=CARTESIAN_POINT('Ctrl Pts',(3.58779113946049,1.61544265843847,9.98841102539611));
#31244=CARTESIAN_POINT('Ctrl Pts',(3.63375491454719,1.50918803068272,9.98253850974011));
#31245=CARTESIAN_POINT('Ctrl Pts',(3.67489731258031,1.40129181186146,9.97666599408411));
#31246=CARTESIAN_POINT('Ctrl Pts',(3.68626809200505,1.37147186544046,9.97504297055158));
#31247=CARTESIAN_POINT('Ctrl Pts',(3.69727089338434,1.34152660458722,9.97341994701905));
#31248=CARTESIAN_POINT('Ctrl Pts',(3.70790319572806,1.31146593211934,9.97179692348651));
#31249=CARTESIAN_POINT('Ctrl Pts',(3.75282647998858,1.18445448241816,9.9649393732442));
#31250=CARTESIAN_POINT('Ctrl Pts',(3.79125534051289,1.05503264886109,9.95808182300188));
#31251=CARTESIAN_POINT('Ctrl Pts',(3.82296277587289,0.923820661324593,9.95122427275956));
#31252=CARTESIAN_POINT('Ctrl Pts',(3.85452351214834,0.793215745228449,9.94439844997585));
#31253=CARTESIAN_POINT('Ctrl Pts',(3.87942477998307,0.660837308486352,9.93757262719214));
#31254=CARTESIAN_POINT('Ctrl Pts',(3.89748945725625,0.527318623392355,9.93074680440843));
#31255=CARTESIAN_POINT('Ctrl Pts',(3.91540359399889,0.39491260548778,9.92397786406815));
#31256=CARTESIAN_POINT('Ctrl Pts',(3.92659452399959,0.26138538800618,9.91720892372788));
#31257=CARTESIAN_POINT('Ctrl Pts',(3.93093689015499,0.127374116753154,9.9104399833876));
#31258=CARTESIAN_POINT('Ctrl Pts',(3.93227903490181,0.0859537212152617,
9.9083478296184));
#31259=CARTESIAN_POINT('Ctrl Pts',(3.93296727603341,0.0444872179918603,
9.90625567584921));
#31260=CARTESIAN_POINT('Ctrl Pts',(3.9329988605794,0.00299377372985386,
9.90416352208001));
#31261=CARTESIAN_POINT('',(3.93127184741014,-0.00247874324238124,8.65416299050568));
#31262=CARTESIAN_POINT('Ctrl Pts',(3.93299886058008,0.00299377283657058,
9.90416352203497));
#31263=CARTESIAN_POINT('Ctrl Pts',(3.93308723740947,-0.113109214353025,
9.89830945745726));
#31264=CARTESIAN_POINT('Ctrl Pts',(3.9280302285454,-0.229267072370521,9.89245539287955));
#31265=CARTESIAN_POINT('Ctrl Pts',(3.91783999345601,-0.344990993616612,
9.88660132830185));
#31266=CARTESIAN_POINT('Ctrl Pts',(3.90765103618284,-0.460700403528975,
9.88074799780128));
#31267=CARTESIAN_POINT('Ctrl Pts',(3.89233016843786,-0.575975574245469,
9.8748946673007));
#31268=CARTESIAN_POINT('Ctrl Pts',(3.87194153497946,-0.690331622990648,
9.86904133680013));
#31269=CARTESIAN_POINT('Ctrl Pts',(3.85155055435826,-0.80470083653492,9.86318733245746));
#31270=CARTESIAN_POINT('Ctrl Pts',(3.82609072010459,-0.91815031176996,9.85733332811479));
#31271=CARTESIAN_POINT('Ctrl Pts',(3.79567740077867,-1.03020486759578,9.85147932377211));
#31272=CARTESIAN_POINT('Ctrl Pts',(3.76525326530779,-1.14229927432729,9.84562323752056));
#31273=CARTESIAN_POINT('Ctrl Pts',(3.72987224910885,-1.25299737736529,9.83976715126901));
#31274=CARTESIAN_POINT('Ctrl Pts',(3.68969952561667,-1.36183934833156,9.83391106501746));
#31275=CARTESIAN_POINT('Ctrl Pts',(3.64947794537558,-1.4708136893336,9.82804785678585));
#31276=CARTESIAN_POINT('Ctrl Pts',(3.60445316681952,-1.57792700461605,9.82218464855424));
#31277=CARTESIAN_POINT('Ctrl Pts',(3.55483852128138,-1.68273945921941,9.81632144032263));
#31278=CARTESIAN_POINT('Ctrl Pts',(3.50518969067181,-1.78762413083063,9.81045419227193));
#31279=CARTESIAN_POINT('Ctrl Pts',(3.45094488790614,-1.89020442123878,9.80458694422123));
#31280=CARTESIAN_POINT('Ctrl Pts',(3.39236251616816,-1.99006672222245,9.79871969617053));
#31281=CARTESIAN_POINT('Ctrl Pts',(3.33368586926898,-2.09008972913596,9.79284300610273));
#31282=CARTESIAN_POINT('Ctrl Pts',(3.27065794049003,-2.18738566878382,9.78696631603493));
#31283=CARTESIAN_POINT('Ctrl Pts',(3.20357953500277,-2.28157120487427,9.78108962596713));
#31284=CARTESIAN_POINT('Ctrl Pts',(3.17228284329568,-2.3255152382018,9.77834774568578));
#31285=CARTESIAN_POINT('Ctrl Pts',(3.14010497705328,-2.36878266652459,9.77560586540443));
#31286=CARTESIAN_POINT('Ctrl Pts',(3.1070792877133,-2.41133724307966,9.77286398512307));
#31287=CARTESIAN_POINT('Ctrl Pts',(3.03635009140188,-2.50247390242771,9.76699185973954));
#31288=CARTESIAN_POINT('Ctrl Pts',(2.96148909624755,-2.59064877599629,9.761119734356));
#31289=CARTESIAN_POINT('Ctrl Pts',(2.88277340207827,-2.67546379386268,9.75524760897246));
#31290=CARTESIAN_POINT('Ctrl Pts',(2.80415976464377,-2.76016884707875,9.74938309693654));
#31291=CARTESIAN_POINT('Ctrl Pts',(2.72170164544951,-2.84152240713908,9.74351858490063));
#31292=CARTESIAN_POINT('Ctrl Pts',(2.63571778942591,-2.91915753848671,9.73765407286471));
#31293=CARTESIAN_POINT('Ctrl Pts',(2.54982241025973,-2.99671278376311,9.7317955953755));
#31294=CARTESIAN_POINT('Ctrl Pts',(2.46040881544806,-3.07055693551838,9.72593711788628));
#31295=CARTESIAN_POINT('Ctrl Pts',(2.3678337020125,-3.14035866735215,9.72007864039707));
#31296=CARTESIAN_POINT('Ctrl Pts',(2.27160826001953,-3.21291275071554,9.71398915732885));
#31297=CARTESIAN_POINT('Ctrl Pts',(2.17196715603456,-3.28109872888663,9.70789967426062));
#31298=CARTESIAN_POINT('Ctrl Pts',(2.06935061857032,-3.34458921504908,9.70181019119239));
#31299=CARTESIAN_POINT('Ctrl Pts',(1.97074130625292,-3.40560036718778,9.69595850536704));
#31300=CARTESIAN_POINT('Ctrl Pts',(1.86938496856155,-3.46227563004297,9.69010681954169));
#31301=CARTESIAN_POINT('Ctrl Pts',(1.76570245622905,-3.51436819870467,9.68425513371633));
#31302=CARTESIAN_POINT('Ctrl Pts',(1.66203575820139,-3.56645282188219,9.67840434042668));
#31303=CARTESIAN_POINT('Ctrl Pts',(1.55604396029811,-3.61395595511132,9.67255354713702));
#31304=CARTESIAN_POINT('Ctrl Pts',(1.4481719907339,-3.65667702774716,9.66670275384737));
#31305=CARTESIAN_POINT('Ctrl Pts',(1.34029034680878,-3.69940193176827,9.66085143583673));
#31306=CARTESIAN_POINT('Ctrl Pts',(1.23052858041005,-3.73734377040407,9.65500011782609));
#31307=CARTESIAN_POINT('Ctrl Pts',(1.11935037322815,-3.77035061260276,9.64914879981545));
#31308=CARTESIAN_POINT('Ctrl Pts',(1.00813526670446,-3.80336840956302,9.64329553978948));
#31309=CARTESIAN_POINT('Ctrl Pts',(0.895503180725383,-3.8314478356438,9.63744227976351));
#31310=CARTESIAN_POINT('Ctrl Pts',(0.781930985552084,-3.85448737627114,
9.63158901973754));
#31311=CARTESIAN_POINT('Ctrl Pts',(0.66822958083112,-3.87755312867169,9.62572910053695));
#31312=CARTESIAN_POINT('Ctrl Pts',(0.553586337524964,-3.89556746884632,
9.61986918133634));
#31313=CARTESIAN_POINT('Ctrl Pts',(0.43848640339453,-3.90848035354383,9.61400926213575));
#31314=CARTESIAN_POINT('Ctrl Pts',(0.323308969729893,-3.92140193279497,
9.60814539731162));
#31315=CARTESIAN_POINT('Ctrl Pts',(0.207674644412055,-3.92921518914535,
9.60228153248749));
#31316=CARTESIAN_POINT('Ctrl Pts',(0.0920700048664749,-3.93192219076165,
9.59641766766336));
#31317=CARTESIAN_POINT('Ctrl Pts',(-0.0237051783309354,-3.93463318583308,
9.5905451522788));
#31318=CARTESIAN_POINT('Ctrl Pts',(-0.139450176577184,-3.93222290045582,
9.58467263689424));
#31319=CARTESIAN_POINT('Ctrl Pts',(-0.254682016237665,-3.92474535105211,
9.57880012150967));
#31320=CARTESIAN_POINT('Ctrl Pts',(-0.286529382266794,-3.92267873254143,
9.57717709659299));
#31321=CARTESIAN_POINT('Ctrl Pts',(-0.31833760521875,-3.92022535841899,
9.57555407167632));
#31322=CARTESIAN_POINT('Ctrl Pts',(-0.350096631160233,-3.91738705629789,
9.57393104675964));
#31323=CARTESIAN_POINT('Ctrl Pts',(-0.465001345995669,-3.90711802926783,
9.56805891404481));
#31324=CARTESIAN_POINT('Ctrl Pts',(-0.579646493589882,-3.89177192615486,
9.56218678132999));
#31325=CARTESIAN_POINT('Ctrl Pts',(-0.693547389923439,-3.87136681521273,
9.55631464861516));
#31326=CARTESIAN_POINT('Ctrl Pts',(-0.807300612601107,-3.85098815970185,
9.55045012917937));
#31327=CARTESIAN_POINT('Ctrl Pts',(-0.920311099740817,-3.82556361216972,
9.54458560974357));
#31328=CARTESIAN_POINT('Ctrl Pts',(-1.03209786236774,-3.79516310617817,
9.53872109030778));
#31329=CARTESIAN_POINT('Ctrl Pts',(-1.14376959837936,-3.76479388177333,
9.53286260535948));
#31330=CARTESIAN_POINT('Ctrl Pts',(-1.25421971794834,-3.72945899101311,
9.52700412041119));
#31331=CARTESIAN_POINT('Ctrl Pts',(-1.36297668791349,-3.68927954324477,
9.52114563546289));
#31332=CARTESIAN_POINT('Ctrl Pts',(-1.4760218576683,-3.64751585219047,9.51505615516844));
#31333=CARTESIAN_POINT('Ctrl Pts',(-1.58723716410742,-3.60051779123602,
9.508966674874));
#31334=CARTESIAN_POINT('Ctrl Pts',(-1.6961092556027,-3.54847888440369,9.50287719457955));
#31335=CARTESIAN_POINT('Ctrl Pts',(-1.80073002235906,-3.49847203453807,
9.49702550119511));
#31336=CARTESIAN_POINT('Ctrl Pts',(-1.90318673160227,-3.44381082464488,
9.49117380781068));
#31337=CARTESIAN_POINT('Ctrl Pts',(-2.00304430489268,-3.38471601654216,
9.48532211442625));
#31338=CARTESIAN_POINT('Ctrl Pts',(-2.10288664770936,-3.32563022169594,
9.47947131355361));
#31339=CARTESIAN_POINT('Ctrl Pts',(-2.20013028710999,-3.26211238366864,
9.47362051268097));
#31340=CARTESIAN_POINT('Ctrl Pts',(-2.29436603792941,-3.19442850663403,
9.46776971180833));
#31341=CARTESIAN_POINT('Ctrl Pts',(-2.38861024040586,-3.12673855928205,
9.46191838619893));
#31342=CARTESIAN_POINT('Ctrl Pts',(-2.4798456822328,-3.05488207135051,9.45606706058954));
#31343=CARTESIAN_POINT('Ctrl Pts',(-2.56769397226143,-2.97916710924585,
9.45021573498014));
#31344=CARTESIAN_POINT('Ctrl Pts',(-2.65557141865656,-2.90342701775981,
9.44436246734782));
#31345=CARTESIAN_POINT('Ctrl Pts',(-2.74005916491526,-2.82382617545463,
9.43850919971549));
#31346=CARTESIAN_POINT('Ctrl Pts',(-2.82081411601947,-2.74071098856945,
9.43265593208316));
#31347=CARTESIAN_POINT('Ctrl Pts',(-2.90166094043903,-2.65750124317521,
9.42679600530368));
#31348=CARTESIAN_POINT('Ctrl Pts',(-2.97876620509092,-2.57076946958095,
9.42093607852419));
#31349=CARTESIAN_POINT('Ctrl Pts',(-3.05182565235624,-2.48089685146731,
9.41507615174471));
#31350=CARTESIAN_POINT('Ctrl Pts',(-3.12493429214566,-2.39096372015383,
9.40921227934833));
#31351=CARTESIAN_POINT('Ctrl Pts',(-3.1939914445301,-2.29788586454191,9.40334840695194));
#31352=CARTESIAN_POINT('Ctrl Pts',(-3.25873592809101,-2.20207382959082,
9.39748453455556));
#31353=CARTESIAN_POINT('Ctrl Pts',(-3.32357592389546,-2.1061204509775,9.39161201166763));
#31354=CARTESIAN_POINT('Ctrl Pts',(-3.38409033796464,-2.00742519400292,
9.38573948877969));
#31355=CARTESIAN_POINT('Ctrl Pts',(-3.44006364760443,-1.9064236413847,9.37986696589175));
#31356=CARTESIAN_POINT('Ctrl Pts',(-3.45553264184485,-1.8785104726659,9.37824401339324));
#31357=CARTESIAN_POINT('Ctrl Pts',(-3.47065508372829,-1.85042127389786,
9.37662106089472));
#31358=CARTESIAN_POINT('Ctrl Pts',(-3.48542707898021,-1.82216549114274,
9.3749981083962));
#31359=CARTESIAN_POINT('Ctrl Pts',(-3.53887451052616,-1.71993156885758,
9.36912600777014));
#31360=CARTESIAN_POINT('Ctrl Pts',(-3.58790967536027,-1.61517268576546,
9.36325390714409));
#31361=CARTESIAN_POINT('Ctrl Pts',(-3.63228587862215,-1.50830643304407,
9.35738180651803));
#31362=CARTESIAN_POINT('Ctrl Pts',(-3.67660454692182,-1.40157873534451,
9.35151731923116));
#31363=CARTESIAN_POINT('Ctrl Pts',(-3.71627610887297,-1.29274947977079,
9.3456528319443));
#31364=CARTESIAN_POINT('Ctrl Pts',(-3.75109950768657,-1.18226117395166,
9.33978834465744));
#31365=CARTESIAN_POINT('Ctrl Pts',(-3.78588707350342,-1.07188655970882,
9.33392989188073));
#31366=CARTESIAN_POINT('Ctrl Pts',(-3.81583627545891,-0.959856682742663,
9.32807143910402));
#31367=CARTESIAN_POINT('Ctrl Pts',(-3.8407942275231,-0.846633747157065,
9.32221298632732));
#31368=CARTESIAN_POINT('Ctrl Pts',(-3.86673644534915,-0.728945643168742,
9.31612349398171));
#31369=CARTESIAN_POINT('Ctrl Pts',(-3.8872854590377,-0.609968863406854,
9.31003400163611));
#31370=CARTESIAN_POINT('Ctrl Pts',(-3.90232671628392,-0.490239940617599,
9.30394450929051));
#31371=CARTESIAN_POINT('Ctrl Pts',(-3.9167805227377,-0.375187146254242,
9.29809284793505));
#31372=CARTESIAN_POINT('Ctrl Pts',(-3.92614866336008,-0.25944030638907,
9.29224118657959));
#31373=CARTESIAN_POINT('Ctrl Pts',(-3.93038180241211,-0.143484798037018,
9.28638952522413));
#31374=CARTESIAN_POINT('Ctrl Pts',(-3.9346142958907,-0.0275469734405368,
9.28053875627431));
#31375=CARTESIAN_POINT('Ctrl Pts',(-3.93371332979162,0.0885990433418262,
9.2746879873245));
#31376=CARTESIAN_POINT('Ctrl Pts',(-3.92768162855818,0.204465216324347,
9.26883721837467));
#31377=CARTESIAN_POINT('Ctrl Pts',(-3.92164938621706,0.320341783733489,
9.26298592454872));
#31378=CARTESIAN_POINT('Ctrl Pts',(-3.91048551523794,0.435938044554662,
9.25713463072277));
#31379=CARTESIAN_POINT('Ctrl Pts',(-3.89424477246337,0.550769145960201,
9.25128333689682));
#31380=CARTESIAN_POINT('Ctrl Pts',(-3.87799863896647,0.665638362776525,
9.2454301008752));
#31381=CARTESIAN_POINT('Ctrl Pts',(-3.85667234073705,0.779741506036119,
9.23957686485357));
#31382=CARTESIAN_POINT('Ctrl Pts',(-3.83037196752621,0.892602705793224,
9.23372362883195));
#31383=CARTESIAN_POINT('Ctrl Pts',(-3.8040416708739,1.00559231420364,9.22786373324835));
#31384=CARTESIAN_POINT('Ctrl Pts',(-3.7727260973294,1.11733675587199,9.22200383766475));
#31385=CARTESIAN_POINT('Ctrl Pts',(-3.73658158551186,1.2273740484521,9.21614394208114));
#31386=CARTESIAN_POINT('Ctrl Pts',(-3.70041273542503,1.33748543574599,9.21028010067812));
#31387=CARTESIAN_POINT('Ctrl Pts',(-3.65940861837551,1.44588699928753,9.2044162592751));
#31388=CARTESIAN_POINT('Ctrl Pts',(-3.61377355483072,1.55213713775754,9.19855241787208));
#31389=CARTESIAN_POINT('Ctrl Pts',(-3.5680711650671,1.65854402894175,9.1926799254398));
#31390=CARTESIAN_POINT('Ctrl Pts',(-3.51772437228785,1.76279278938837,9.18680743300753));
#31391=CARTESIAN_POINT('Ctrl Pts',(-3.46298323625927,1.86446670803939,9.18093494057526));
#31392=CARTESIAN_POINT('Ctrl Pts',(-3.44785185466565,1.8925711094611,9.17931168372776));
#31393=CARTESIAN_POINT('Ctrl Pts',(-3.43238496946287,1.92047895135816,9.17768842688026));
#31394=CARTESIAN_POINT('Ctrl Pts',(-3.41658842808763,1.94818184804646,9.17606517003276));
#31395=CARTESIAN_POINT('Ctrl Pts',(-3.35944435675326,2.04839722221729,9.17019302986713));
#31396=CARTESIAN_POINT('Ctrl Pts',(-3.29779147050594,2.1462642476224,9.1643208897015));
#31397=CARTESIAN_POINT('Ctrl Pts',(-3.23184785157092,2.24134969701214,9.15844874953588));
#31398=CARTESIAN_POINT('Ctrl Pts',(-3.1659897311995,2.33631186427887,9.15258422283698));
#31399=CARTESIAN_POINT('Ctrl Pts',(-3.09585217456309,2.4284992908329,9.14671969613809));
#31400=CARTESIAN_POINT('Ctrl Pts',(-3.02169888992021,2.51750368791289,9.1408551694392));
#31401=CARTESIAN_POINT('Ctrl Pts',(-2.94762191005517,2.60641649821045,9.13499667742116));
#31402=CARTESIAN_POINT('Ctrl Pts',(-2.86953768443757,2.69215247821757,9.12913818540312));
#31403=CARTESIAN_POINT('Ctrl Pts',(-2.78775252360083,2.77433322929261,9.12327969338508));
#31404=CARTESIAN_POINT('Ctrl Pts',(-2.70274278029786,2.85975415995852,9.11719021581359));
#31405=CARTESIAN_POINT('Ctrl Pts',(-2.61373452063478,2.94133337332348,9.11110073824211));
#31406=CARTESIAN_POINT('Ctrl Pts',(-2.52111730152547,3.01868457311275,9.10501126067062));
#31407=CARTESIAN_POINT('Ctrl Pts',(-2.43211653445608,3.09301541764889,9.09915956073699));
#31408=CARTESIAN_POINT('Ctrl Pts',(-2.33978370694337,3.16344194809958,9.09330786080336));
#31409=CARTESIAN_POINT('Ctrl Pts',(-2.24450058085828,3.22966037572479,9.08745616086973));
#31410=CARTESIAN_POINT('Ctrl Pts',(-2.14923199081137,3.29586870131379,9.08160535364962));
#31411=CARTESIAN_POINT('Ctrl Pts',(-2.05101433649171,3.35786996465837,9.07575454642951));
#31412=CARTESIAN_POINT('Ctrl Pts',(-1.95025974780192,3.41540274581251,9.06990373920939));
#31413=CARTESIAN_POINT('Ctrl Pts',(-1.84949612638668,3.47294068482419,9.06405240745996));
#31414=CARTESIAN_POINT('Ctrl Pts',(-1.74619547750079,3.52600914027372,9.05820107571052));
#31415=CARTESIAN_POINT('Ctrl Pts',(-1.64079536833043,3.5743921943829,9.05234974396108));
#31416=CARTESIAN_POINT('Ctrl Pts',(-1.53536028131871,3.62279130478276,9.04649647040196));
#31417=CARTESIAN_POINT('Ctrl Pts',(-1.42782472415334,3.66650174967328,9.04064319684283));
#31418=CARTESIAN_POINT('Ctrl Pts',(-1.31864644328848,3.70535565871923,9.0347899232837));
#31419=CARTESIAN_POINT('Ctrl Pts',(-1.20934395898276,3.74425376876521,9.0289299909211));
#31420=CARTESIAN_POINT('Ctrl Pts',(-1.09839541062445,3.77828417673352,9.0230700585585));
#31421=CARTESIAN_POINT('Ctrl Pts',(-0.986274011150539,3.80732879784883,
9.0172101261959));
#31422=CARTESIAN_POINT('Ctrl Pts',(-0.874077121646961,3.83639297436856,
9.01134624840923));
#31423=CARTESIAN_POINT('Ctrl Pts',(-0.76070621205463,3.86046459419032,9.00548237062256));
#31424=CARTESIAN_POINT('Ctrl Pts',(-0.646643273153777,3.87947695924141,
8.99961849283589));
#31425=CARTESIAN_POINT('Ctrl Pts',(-0.532412072966534,3.8985173706065,8.9937459648809));
#31426=CARTESIAN_POINT('Ctrl Pts',(-0.417487214888083,3.91248358231421,
8.98787343692592));
#31427=CARTESIAN_POINT('Ctrl Pts',(-0.302354461510855,3.92136083261978,
8.98200090897094));
#31428=CARTESIAN_POINT('Ctrl Pts',(-0.270537146075454,3.92381408996737,
8.98037801653707));
#31429=CARTESIAN_POINT('Ctrl Pts',(-0.238703942649404,3.92587900404544,
8.9787551241032));
#31430=CARTESIAN_POINT('Ctrl Pts',(-0.206865060006896,3.9275559635667,8.97713223166932));
#31431=CARTESIAN_POINT('Ctrl Pts',(-0.0916611652256139,3.93362377286796,
8.97126005545973));
#31432=CARTESIAN_POINT('Ctrl Pts',(0.0240030410320682,3.93462867854233,
8.96538787925015));
#31433=CARTESIAN_POINT('Ctrl Pts',(0.139645176672874,3.93052009594557,8.95951570304056));
#31434=CARTESIAN_POINT('Ctrl Pts',(0.255137388099245,3.92641683991958,8.95365113981217));
#31435=CARTESIAN_POINT('Ctrl Pts',(0.370607176484888,3.91721329360362,8.94778657658379));
#31436=CARTESIAN_POINT('Ctrl Pts',(0.485568490821238,3.90291073952782,8.94192201335541));
#31437=CARTESIAN_POINT('Ctrl Pts',(0.600411517643439,3.88862290182489,8.93606348437089));
#31438=CARTESIAN_POINT('Ctrl Pts',(0.714746703286442,3.86924654271268,8.93020495538637));
#31439=CARTESIAN_POINT('Ctrl Pts',(0.82809012813836,3.84483494309961,8.92434642640185));
#31440=CARTESIAN_POINT('Ctrl Pts',(0.945901389870079,3.81946107289001,8.91825696252286));
#31441=CARTESIAN_POINT('Ctrl Pts',(1.06264064041209,3.78864685009729,8.91216749864386));
#31442=CARTESIAN_POINT('Ctrl Pts',(1.17777234658628,3.75251133237685,8.90607803476486));
#31443=CARTESIAN_POINT('Ctrl Pts',(1.28840943461754,3.71778650645406,8.90022629701483));
#31444=CARTESIAN_POINT('Ctrl Pts',(1.39756170571898,3.67814820215032,8.89437455926481));
#31445=CARTESIAN_POINT('Ctrl Pts',(1.50476725107607,3.63375350293453,8.88852282151479));
#31446=CARTESIAN_POINT('Ctrl Pts',(1.61195644619781,3.58936557448585,8.88267197623063));
#31447=CARTESIAN_POINT('Ctrl Pts',(1.71719912406298,3.54022285159701,8.87682113094647));
#31448=CARTESIAN_POINT('Ctrl Pts',(1.8200526177605,3.48653086442428,8.87097028566231));
#31449=CARTESIAN_POINT('Ctrl Pts',(1.92291533591624,3.43283406186343,8.86511891564266));
#31450=CARTESIAN_POINT('Ctrl Pts',(2.02338807744833,3.37458737526685,8.85926754562302));
#31451=CARTESIAN_POINT('Ctrl Pts',(2.12105271812888,3.31204232565317,8.85341617560337));
#31452=CARTESIAN_POINT('Ctrl Pts',(2.21874977211252,3.24947651835652,8.84756286360935));
#31453=CARTESIAN_POINT('Ctrl Pts',(2.31363652414597,3.18260973425628,8.84170955161533));
#31454=CARTESIAN_POINT('Ctrl Pts',(2.40532437545746,3.11173643627319,8.8358562396213));
#31455=CARTESIAN_POINT('Ctrl Pts',(2.49711653278522,3.04078251134479,8.8299962687772));
#31456=CARTESIAN_POINT('Ctrl Pts',(2.58570219849534,2.96581322807541,8.82413629793309));
#31457=CARTESIAN_POINT('Ctrl Pts',(2.67072630827555,2.88716296496836,8.81827632708898));
#31458=CARTESIAN_POINT('Ctrl Pts',(2.75580766450286,2.80845974690372,8.81241241074622));
#31459=CARTESIAN_POINT('Ctrl Pts',(2.83732239989423,2.72607090719513,8.80654849440346));
#31460=CARTESIAN_POINT('Ctrl Pts',(2.91495394598017,2.64036597705974,8.8006845780607));
#31461=CARTESIAN_POINT('Ctrl Pts',(2.99270000784788,2.55453462193901,8.79481201174253));
#31462=CARTESIAN_POINT('Ctrl Pts',(3.06655118532422,2.46537773078405,8.78893944542437));
#31463=CARTESIAN_POINT('Ctrl Pts',(3.13623257323649,2.37329607225276,8.7830668791062));
#31464=CARTESIAN_POINT('Ctrl Pts',(3.15548481129688,2.34785487390477,8.78144435050609));
#31465=CARTESIAN_POINT('Ctrl Pts',(3.1744190083362,2.32219056727557,8.77982182190599));
#31466=CARTESIAN_POINT('Ctrl Pts',(3.19302997863455,2.29631194647876,8.77819929330588));
#31467=CARTESIAN_POINT('Ctrl Pts',(3.26096126127469,2.20185325488431,8.77227695571904));
#31468=CARTESIAN_POINT('Ctrl Pts',(3.32480947415829,2.10422199904811,8.76635461813219));
#31469=CARTESIAN_POINT('Ctrl Pts',(3.38426712749915,2.00380263741933,8.76043228054534));
#31470=CARTESIAN_POINT('Ctrl Pts',(3.44364508310638,1.90351787907683,8.75451788132904));
#31471=CARTESIAN_POINT('Ctrl Pts',(3.49864397968998,1.8004527916056,8.74860348211273));
#31472=CARTESIAN_POINT('Ctrl Pts',(3.54899787998221,1.69502302281762,8.74268908289643));
#31473=CARTESIAN_POINT('Ctrl Pts',(3.59929577739263,1.5897105114982,8.73678126158964));
#31474=CARTESIAN_POINT('Ctrl Pts',(3.64495878208342,1.48203891261819,8.73087344028286));
#31475=CARTESIAN_POINT('Ctrl Pts',(3.68576573473105,1.37245034470559,8.72496561897608));
#31476=CARTESIAN_POINT('Ctrl Pts',(3.72653238350795,1.26297001431596,8.71906363265698));
#31477=CARTESIAN_POINT('Ctrl Pts',(3.76245238819303,1.15157686122514,8.71316164633788));
#31478=CARTESIAN_POINT('Ctrl Pts',(3.79335209321593,1.03873427636443,8.70725966001879));
#31479=CARTESIAN_POINT('Ctrl Pts',(3.82423340147542,0.92595887461549,8.70136118756644));
#31480=CARTESIAN_POINT('Ctrl Pts',(3.85010025013148,0.811736146639425,8.69546271511409));
#31481=CARTESIAN_POINT('Ctrl Pts',(3.87082848282112,0.696545660083203,8.68956424266174));
#31482=CARTESIAN_POINT('Ctrl Pts',(3.89156250563976,0.581322996747287,8.68366412255728));
#31483=CARTESIAN_POINT('Ctrl Pts',(3.9071549464799,0.465132427676677,8.67776400245282));
#31484=CARTESIAN_POINT('Ctrl Pts',(3.91753252051055,0.348465135619414,8.67186388234835));
#31485=CARTESIAN_POINT('Ctrl Pts',(3.9279100945412,0.231797843562152,8.66596376224389));
#31486=CARTESIAN_POINT('Ctrl Pts',(3.93307275953401,0.114654231718768,8.66006364213943));
#31487=CARTESIAN_POINT('Ctrl Pts',(3.93299922484218,-0.00246928954045427,
8.65416352203497));
#31488=CARTESIAN_POINT('Ctrl Pts',(3.92808040047205,-0.00249620959774103,
8.65416200846926));
#31489=CARTESIAN_POINT('Ctrl Pts',(3.93089496884793,-0.497463850130089,
8.62919679062698));
#31490=CARTESIAN_POINT('Ctrl Pts',(3.61407832683064,-2.30365100072786,8.53792059333025));
#31491=CARTESIAN_POINT('Ctrl Pts',(0.898627897229635,-4.56470309825019,
8.38033341657901));
#31492=CARTESIAN_POINT('Ctrl Pts',(-3.35540415369693,-3.22274549575858,
8.18140047821557));
#31493=CARTESIAN_POINT('Ctrl Pts',(-4.52475415810096,1.08211876658719,7.98246753985213));
#31494=CARTESIAN_POINT('Ctrl Pts',(-1.53456114674909,4.39176043556087,7.78353460148871));
#31495=CARTESIAN_POINT('Ctrl Pts',(2.73011925450327,3.68738255941635,7.5907671869393));
#31496=CARTESIAN_POINT('Ctrl Pts',(3.93032929473929,1.18226324547227,7.46431075184439));
#31497=CARTESIAN_POINT('Ctrl Pts',(3.93806266851679,-0.00234938565519546,
7.40416529620395));
#31498=CARTESIAN_POINT('Origin',(0.,0.,4.68922655072688));
#31499=CARTESIAN_POINT('',(-1.83231942908391,2.65117390457541,42.));
#31500=CARTESIAN_POINT('Ctrl Pts',(-1.83231942908391,2.65117390457541,42.));
#31501=CARTESIAN_POINT('Ctrl Pts',(-1.59286454902597,2.81666958494625,41.9809759492185));
#31502=CARTESIAN_POINT('Ctrl Pts',(-1.33201263913347,2.94901901405471,41.9607686073061));
#31503=CARTESIAN_POINT('Ctrl Pts',(-0.94038760612917,3.08496026826113,41.9333795023616));
#31504=CARTESIAN_POINT('Ctrl Pts',(-0.821717533680347,3.11866883638072,
41.9254078541967));
#31505=CARTESIAN_POINT('Ctrl Pts',(-0.671731090466772,3.15211335156219,
41.9157406907206));
#31506=CARTESIAN_POINT('Ctrl Pts',(-0.641974702652182,3.15830806302118,
41.9138420609115));
#31507=CARTESIAN_POINT('Ctrl Pts',(-0.598694209464382,3.16668126009764,
41.9111075101178));
#31508=CARTESIAN_POINT('Ctrl Pts',(-0.585237524082561,3.16919579847215,
41.9102610503663));
#31509=CARTESIAN_POINT('Ctrl Pts',(-0.561656668655719,3.17344684048019,
41.9087842018925));
#31510=CARTESIAN_POINT('Ctrl Pts',(-0.551539533996479,3.17522081264738,
41.9081526455468));
#31511=CARTESIAN_POINT('Ctrl Pts',(-0.531905083053156,3.17856690831476,
41.9069309206604));
#31512=CARTESIAN_POINT('Ctrl Pts',(-0.522388860922958,3.180144727703,41.9063405801605));
#31513=CARTESIAN_POINT('Ctrl Pts',(-0.49966244361569,3.18380807496898,41.9049349411649));
#31514=CARTESIAN_POINT('Ctrl Pts',(-0.486446001051586,3.18585415738281,
41.9041208777451));
#31515=CARTESIAN_POINT('Ctrl Pts',(-0.438906241083337,3.1929112181866,41.9012044743489));
#31516=CARTESIAN_POINT('Ctrl Pts',(-0.404514505945473,3.19745037307116,
41.8991167496231));
#31517=CARTESIAN_POINT('Ctrl Pts',(-0.112663242478015,3.23118559459845,
41.8815703265869));
#31518=CARTESIAN_POINT('Ctrl Pts',(0.147375533090322,3.22979078434417,41.8671569875167));
#31519=CARTESIAN_POINT('Ctrl Pts',(0.490901260419218,3.18633410705426,41.8476740325027));
#31520=CARTESIAN_POINT('Ctrl Pts',(0.576859467941198,3.17189865197372,41.8427508154163));
#31521=CARTESIAN_POINT('Ctrl Pts',(0.755107119359493,3.13447887242855,41.8322621000324));
#31522=CARTESIAN_POINT('Ctrl Pts',(0.847173105909439,3.11085819303723,41.8266838854335));
#31523=CARTESIAN_POINT('Ctrl Pts',(0.951039404733918,3.07925736302113,41.8200673721665));
#31524=CARTESIAN_POINT('Ctrl Pts',(0.964001760132938,3.07522396727318,41.8192357783498));
#31525=CARTESIAN_POINT('Ctrl Pts',(0.982384632964249,3.06937626616702,41.8180475754683));
#31526=CARTESIAN_POINT('Ctrl Pts',(0.98782661221302,3.06762918447521,41.8176947181694));
#31527=CARTESIAN_POINT('Ctrl Pts',(0.99866925401454,3.06411644173785,41.8169894190578));
#31528=CARTESIAN_POINT('Ctrl Pts',(1.00406995132958,3.06235095622799,41.8166369882612));
#31529=CARTESIAN_POINT('Ctrl Pts',(1.01527337855022,3.05865573825014,41.8159035035219));
#31530=CARTESIAN_POINT('Ctrl Pts',(1.02107530356226,3.05672376584055,41.8155223159985));
#31531=CARTESIAN_POINT('Ctrl Pts',(1.03623404439014,3.05162811097689,41.8145229451406));
#31532=CARTESIAN_POINT('Ctrl Pts',(1.04558181125822,3.04843792662141,41.8139032416118));
#31533=CARTESIAN_POINT('Ctrl Pts',(1.08473045582555,3.03487612066088,41.811293922843));
#31534=CARTESIAN_POINT('Ctrl Pts',(1.11439169949277,3.02411047992125,41.8092828759173));
#31535=CARTESIAN_POINT('Ctrl Pts',(1.39636947860304,2.91705416425172,41.7898688269073));
#31536=CARTESIAN_POINT('Ctrl Pts',(1.63579034605531,2.78984588992295,41.7712081228864));
#31537=CARTESIAN_POINT('Ctrl Pts',(1.98606021360407,2.54298862628443,41.7425745710956));
#31538=CARTESIAN_POINT('Ctrl Pts',(2.1086889113403,2.44226742333424,41.7322130210346));
#31539=CARTESIAN_POINT('Ctrl Pts',(2.24840109434542,2.30911251730484,41.7200350503971));
#31540=CARTESIAN_POINT('Ctrl Pts',(2.27299514247021,2.28490729120114,41.7178750524692));
#31541=CARTESIAN_POINT('Ctrl Pts',(2.30723339790549,2.25011030906333,41.7148436175089));
#31542=CARTESIAN_POINT('Ctrl Pts',(2.31720235528355,2.23984276470445,41.7139579489364));
#31543=CARTESIAN_POINT('Ctrl Pts',(2.33422185681955,2.22207825785498,41.7124405286845));
#31544=CARTESIAN_POINT('Ctrl Pts',(2.34130542534912,2.21461336806681,41.7118073492769));
#31545=CARTESIAN_POINT('Ctrl Pts',(2.35476003665294,2.20029776380871,41.7106015022732));
#31546=CARTESIAN_POINT('Ctrl Pts',(2.36113723067631,2.19345299937417,41.7100285738766));
#31547=CARTESIAN_POINT('Ctrl Pts',(2.37755960094831,2.1756719442829,41.7085495201214));
#31548=CARTESIAN_POINT('Ctrl Pts',(2.38755923215579,2.16469374037955,41.7076453351494));
#31549=CARTESIAN_POINT('Ctrl Pts',(2.42100037529773,2.12746638767069,41.7046089499004));
#31550=CARTESIAN_POINT('Ctrl Pts',(2.44408824537454,2.10090191198268,41.7024915326204));
#31551=CARTESIAN_POINT('Ctrl Pts',(2.64166159662193,1.86591154459648,41.6841675428929));
#31552=CARTESIAN_POINT('Ctrl Pts',(2.78956234557991,1.63656959213224,41.6691492568824));
#31553=CARTESIAN_POINT('Ctrl Pts',(2.9631727689299,1.27385138824258,41.6466322343774));
#31554=CARTESIAN_POINT('Ctrl Pts',(3.01223664969729,1.15304600177306,41.6392887354463));
#31555=CARTESIAN_POINT('Ctrl Pts',(3.07220569088834,0.97517694271233,41.6282728120498));
#31556=CARTESIAN_POINT('Ctrl Pts',(3.08909930036871,0.920262160881826,41.6248442994261));
#31557=CARTESIAN_POINT('Ctrl Pts',(3.10766907526759,0.853609146558072,41.6206176280295));
#31558=CARTESIAN_POINT('Ctrl Pts',(3.11076093109885,0.842271972773622,41.6198964499384));
#31559=CARTESIAN_POINT('Ctrl Pts',(3.11547387240395,0.824610655429433,41.6187691205578));
#31560=CARTESIAN_POINT('Ctrl Pts',(3.11713789855208,0.818297930040075,41.6183654116117));
#31561=CARTESIAN_POINT('Ctrl Pts',(3.12018501470388,0.806594082455271,41.6176154419066));
#31562=CARTESIAN_POINT('Ctrl Pts',(3.12157332435453,0.801204418065614,41.6172694890409));
#31563=CARTESIAN_POINT('Ctrl Pts',(3.12467900035397,0.789017024318631,41.616485859968));
#31564=CARTESIAN_POINT('Ctrl Pts',(3.12638812722437,0.78221735831384,41.6160477201379));
#31565=CARTESIAN_POINT('Ctrl Pts',(3.13138179104575,0.762072518982309,41.6147470314962));
#31566=CARTESIAN_POINT('Ctrl Pts',(3.13460311498892,0.748712054829437,41.6138809568673));
#31567=CARTESIAN_POINT('Ctrl Pts',(3.15789296760548,0.649331766262787,41.6074154191471));
#31568=CARTESIAN_POINT('Ctrl Pts',(3.17450101425351,0.562547741124929,41.6016405442463));
#31569=CARTESIAN_POINT('Ctrl Pts',(3.22464291288388,0.226208853058234,41.5790382922504));
#31570=CARTESIAN_POINT('Ctrl Pts',(3.2324633839039,-0.0262809476336652,
41.5616906602602));
#31571=CARTESIAN_POINT('Ctrl Pts',(3.20317956367178,-0.36556493571607,41.5391906679312));
#31572=CARTESIAN_POINT('Ctrl Pts',(3.19189540397188,-0.453655238773622,
41.5334135218898));
#31573=CARTESIAN_POINT('Ctrl Pts',(3.16781545345881,-0.595017718556564,
41.5242586274787));
#31574=CARTESIAN_POINT('Ctrl Pts',(3.15727585998227,-0.648622055070129,
41.5208140707945));
#31575=CARTESIAN_POINT('Ctrl Pts',(3.14169025986463,-0.718461258146075,
41.5163589284154));
#31576=CARTESIAN_POINT('Ctrl Pts',(3.1378720383408,-0.734958064892181,41.5153089607166));
#31577=CARTESIAN_POINT('Ctrl Pts',(3.13141869155242,-0.761872683687758,
41.5135996460059));
#31578=CARTESIAN_POINT('Ctrl Pts',(3.12886120447845,-0.77230860125507,41.5129377892687));
#31579=CARTESIAN_POINT('Ctrl Pts',(3.12381909303895,-0.792446932153368,
41.5116622968975));
#31580=CARTESIAN_POINT('Ctrl Pts',(3.12134134101052,-0.802150922729585,
41.511048445648));
#31581=CARTESIAN_POINT('Ctrl Pts',(3.11552963277203,-0.824477475842125,
41.5096378127874));
#31582=CARTESIAN_POINT('Ctrl Pts',(3.11216411713119,-0.837091701562125,
41.5088420722497));
#31583=CARTESIAN_POINT('Ctrl Pts',(3.10293794073369,-0.870847279490467,
41.5067158154903));
#31584=CARTESIAN_POINT('Ctrl Pts',(3.09693783837874,-0.891950060372449,
41.5053898721548));
#31585=CARTESIAN_POINT('Ctrl Pts',(3.04250168004785,-1.07623138051949,41.4938362706498));
#31586=CARTESIAN_POINT('Ctrl Pts',(2.98142123927022,-1.23540656099934,41.4840513901351));
#31587=CARTESIAN_POINT('Ctrl Pts',(2.79876588818634,-1.61780993259629,41.4601749296067));
#31588=CARTESIAN_POINT('Ctrl Pts',(2.66288760855944,-1.83286666833307,41.4464315698199));
#31589=CARTESIAN_POINT('Ctrl Pts',(2.46997401387528,-2.07078139298229,41.4284117466716));
#31590=CARTESIAN_POINT('Ctrl Pts',(2.4357074177198,-2.11097982633885,41.4252540008806));
#31591=CARTESIAN_POINT('Ctrl Pts',(2.39287369072687,-2.15879658908845,41.4213318078411));
#31592=CARTESIAN_POINT('Ctrl Pts',(2.38523157577708,-2.16723730441179,41.420632965618));
#31593=CARTESIAN_POINT('Ctrl Pts',(2.37321798558272,-2.18036580380949,41.4195354796457));
#31594=CARTESIAN_POINT('Ctrl Pts',(2.36887689230881,-2.18508144308042,41.4191391286467));
#31595=CARTESIAN_POINT('Ctrl Pts',(2.36073507443293,-2.19387295194582,41.4183961095489));
#31596=CARTESIAN_POINT('Ctrl Pts',(2.35693781790056,-2.19795194250644,41.4180497072395));
#31597=CARTESIAN_POINT('Ctrl Pts',(2.34825815720645,-2.20722722652227,41.4172582474309));
#31598=CARTESIAN_POINT('Ctrl Pts',(2.34336906204687,-2.21241719372926,41.4168126760375));
#31599=CARTESIAN_POINT('Ctrl Pts',(2.32836942123389,-2.22823440496519,41.4154465353617));
#31600=CARTESIAN_POINT('Ctrl Pts',(2.31820367673029,-2.23880870536164,41.4145218481882));
#31601=CARTESIAN_POINT('Ctrl Pts',(2.17773587137418,-2.38293936435441,41.4017656477714));
#31602=CARTESIAN_POINT('Ctrl Pts',(2.03616138166091,-2.50498781788348,41.3891734371723));
#31603=CARTESIAN_POINT('Ctrl Pts',(1.76919758739966,-2.69747762768972,41.3668955958529));
#31604=CARTESIAN_POINT('Ctrl Pts',(1.6481353518135,-2.77310298544616,41.3572445852661));
#31605=CARTESIAN_POINT('Ctrl Pts',(1.43845856146293,-2.88548734928111,41.3414825842501));
#31606=CARTESIAN_POINT('Ctrl Pts',(1.35249874248371,-2.92676446122756,41.3352641694782));
#31607=CARTESIAN_POINT('Ctrl Pts',(1.21185065068668,-2.98677974816566,41.3254872890444));
#31608=CARTESIAN_POINT('Ctrl Pts',(1.15827358394486,-3.00796247610289,41.3218512408999));
#31609=CARTESIAN_POINT('Ctrl Pts',(1.08784211499233,-3.03364773520101,41.3171817336116));
#31610=CARTESIAN_POINT('Ctrl Pts',(1.07148158967866,-3.03946479999321,41.3161046579275));
#31611=CARTESIAN_POINT('Ctrl Pts',(1.04476726808361,-3.04872070100536,41.3143580854135));
#31612=CARTESIAN_POINT('Ctrl Pts',(1.03444178187883,-3.05223963046383,41.3136859409618));
#31613=CARTESIAN_POINT('Ctrl Pts',(1.01452814382783,-3.05891354696338,41.3123952110237));
#31614=CARTESIAN_POINT('Ctrl Pts',(1.00494266174938,-3.0620760429295,41.3117763836653));
#31615=CARTESIAN_POINT('Ctrl Pts',(0.982927305668118,-3.06922496104284,
41.3103606740534));
#31616=CARTESIAN_POINT('Ctrl Pts',(0.970487699424704,-3.07318102018542,
41.3095647985493));
#31617=CARTESIAN_POINT('Ctrl Pts',(0.937295142849948,-3.08351531963327,
41.3074517434146));
#31618=CARTESIAN_POINT('Ctrl Pts',(0.91650096806394,-3.08975968677057,41.3061389440187));
#31619=CARTESIAN_POINT('Ctrl Pts',(0.747870976377588,-3.13854607580705,
41.2955777682768));
#31620=CARTESIAN_POINT('Ctrl Pts',(0.597215768152055,-3.1706662929314,41.2866818168707));
#31621=CARTESIAN_POINT('Ctrl Pts',(0.227708156346183,-3.22216107032286,
41.2655431921916));
#31622=CARTESIAN_POINT('Ctrl Pts',(0.00808524222401213,-3.23018542070195,
41.2535573529878));
#31623=CARTESIAN_POINT('Ctrl Pts',(-0.275934441114121,-3.2115820863583,
41.2372117431779));
#31624=CARTESIAN_POINT('Ctrl Pts',(-0.341080213456631,-3.20531785104832,
41.2334009724467));
#31625=CARTESIAN_POINT('Ctrl Pts',(-0.430285176728102,-3.19399001368724,
41.2280440695457));
#31626=CARTESIAN_POINT('Ctrl Pts',(-0.454547759379614,-3.1906274930175,
41.226572841367));
#31627=CARTESIAN_POINT('Ctrl Pts',(-0.496295232652938,-3.18435593329998,
41.2240131928583));
#31628=CARTESIAN_POINT('Ctrl Pts',(-0.513799116560879,-3.18157855522713,
41.2229314087993));
#31629=CARTESIAN_POINT('Ctrl Pts',(-0.53889257979365,-3.17738444949102,
41.2213670956979));
#31630=CARTESIAN_POINT('Ctrl Pts',(-0.546501725615189,-3.17608454129136,
41.2208909623499));
#31631=CARTESIAN_POINT('Ctrl Pts',(-0.559699609310544,-3.17378104963471,
41.220061908618));
#31632=CARTESIAN_POINT('Ctrl Pts',(-0.565290560236526,-3.1727900002629,
41.2197096980301));
#31633=CARTESIAN_POINT('Ctrl Pts',(-0.57695212672932,-3.17069107379149,
41.2189729173542));
#31634=CARTESIAN_POINT('Ctrl Pts',(-0.583022181376876,-3.16958053635803,
41.2185882028341));
#31635=CARTESIAN_POINT('Ctrl Pts',(-0.59905364401023,-3.16659991499425,
41.217569020439));
#31636=CARTESIAN_POINT('Ctrl Pts',(-0.609009387712006,-3.16470027794517,
41.2169329051342));
#31637=CARTESIAN_POINT('Ctrl Pts',(-0.650846525681272,-3.15651268470663,
41.2142467976182));
#31638=CARTESIAN_POINT('Ctrl Pts',(-0.682639560770881,-3.14978992422111,
41.2121738855381));
#31639=CARTESIAN_POINT('Ctrl Pts',(-0.978175688202822,-3.08261326551532,
41.1926425823373));
#31640=CARTESIAN_POINT('Ctrl Pts',(-1.23341415224436,-2.98965216311244,
41.1739231776421));
#31641=CARTESIAN_POINT('Ctrl Pts',(-1.47443971851644,-2.86568408750336,
41.1558028684421));
#31642=CARTESIAN_POINT('Ctrl Pts',(-1.47484758497728,-2.86547419705606,
41.155772203341));
#31643=CARTESIAN_POINT('Ctrl Pts',(-1.47525540498233,-2.86526422037662,
41.155741540048));
#31644=CARTESIAN_POINT('',(1.87158653173903,2.62360084935058,42.));
#31645=CARTESIAN_POINT('Origin',(0.,0.,42.));
#31646=CARTESIAN_POINT('',(3.2227499802754,-0.000356559795960891,41.8107734493069));
#31647=CARTESIAN_POINT('Ctrl Pts',(3.2227499802754,-0.000356559795960942,
41.8107734493069));
#31648=CARTESIAN_POINT('Ctrl Pts',(3.22276116218653,0.100710650400674,41.8170618951482));
#31649=CARTESIAN_POINT('Ctrl Pts',(3.21801377018382,0.201942216964461,41.8233503409896));
#31650=CARTESIAN_POINT('Ctrl Pts',(3.20848744225778,0.302862832605988,41.829638786831));
#31651=CARTESIAN_POINT('Ctrl Pts',(3.19897581006305,0.403627763679155,41.8359175318399));
#31652=CARTESIAN_POINT('Ctrl Pts',(3.18469994561519,0.504082287979816,41.8421962768489));
#31653=CARTESIAN_POINT('Ctrl Pts',(3.16569147799305,0.603750800133791,41.8484750218579));
#31654=CARTESIAN_POINT('Ctrl Pts',(3.14657766864607,0.703971658389041,41.8547885626138));
#31655=CARTESIAN_POINT('Ctrl Pts',(3.1226786188447,0.803397339300133,41.8611021033697));
#31656=CARTESIAN_POINT('Ctrl Pts',(3.09407959784692,0.901548115569805,41.8674156441256));
#31657=CARTESIAN_POINT('Ctrl Pts',(3.06570847649884,0.998916748718827,41.8736788735885));
#31658=CARTESIAN_POINT('Ctrl Pts',(3.03271212563611,1.09503031405381,41.8799421030514));
#31659=CARTESIAN_POINT('Ctrl Pts',(2.99522500802737,1.18943041569797,41.8862053325142));
#31660=CARTESIAN_POINT('Ctrl Pts',(2.95776305103302,1.28376715785475,41.8924643582209));
#31661=CARTESIAN_POINT('Ctrl Pts',(2.91581647617623,1.37639233915429,41.8987233839276));
#31662=CARTESIAN_POINT('Ctrl Pts',(2.86956900111435,1.46686444852399,41.9049824096343));
#31663=CARTESIAN_POINT('Ctrl Pts',(2.82334173867697,1.55729701673447,41.9112386998115));
#31664=CARTESIAN_POINT('Ctrl Pts',(2.77281750559416,1.64557801634918,41.9174949899886));
#31665=CARTESIAN_POINT('Ctrl Pts',(2.71822707715101,1.73128828319927,41.9237512801657));
#31666=CARTESIAN_POINT('Ctrl Pts',(2.66278353997809,1.81833798223493,41.9301053401519));
#31667=CARTESIAN_POINT('Ctrl Pts',(2.60314583319936,1.90273552374361,41.9364594001381));
#31668=CARTESIAN_POINT('Ctrl Pts',(2.53960259844331,1.98407061479172,41.9428134601242));
#31669=CARTESIAN_POINT('Ctrl Pts',(2.47703075709567,2.06416232609028,41.9490703847976));
#31670=CARTESIAN_POINT('Ctrl Pts',(2.41067225600933,2.14128425585093,41.955327309471));
#31671=CARTESIAN_POINT('Ctrl Pts',(2.34084384373137,2.21507734893501,41.9615842341443));
#31672=CARTESIAN_POINT('Ctrl Pts',(2.26938935993436,2.29058883777022,41.9679868617869));
#31673=CARTESIAN_POINT('Ctrl Pts',(2.19430165238688,2.3626141854434,41.9743894894295));
#31674=CARTESIAN_POINT('Ctrl Pts',(2.11595976478563,2.43080888518788,41.9807921170721));
#31675=CARTESIAN_POINT('Ctrl Pts',(2.03761787718438,2.49900358493236,41.9871947447148));
#31676=CARTESIAN_POINT('Ctrl Pts',(1.95602218416629,2.56336736150102,41.9935973723574));
#31677=CARTESIAN_POINT('Ctrl Pts',(1.87158653173903,2.62360084935058,42.));
#31678=CARTESIAN_POINT('Ctrl Pts',(-1.47525540501187,-2.86526422036141,
41.4036966894132));
#31679=CARTESIAN_POINT('Ctrl Pts',(-1.38677849737974,-2.91081884505378,
41.4098763065341));
#31680=CARTESIAN_POINT('Ctrl Pts',(-1.29603887642405,-2.95234909938083,
41.416055923655));
#31681=CARTESIAN_POINT('Ctrl Pts',(-1.20343783800877,-2.98962454708761,
41.4222355407759));
#31682=CARTESIAN_POINT('Ctrl Pts',(-1.11095940990869,-3.02685063946888,
41.4284069756473));
#31683=CARTESIAN_POINT('Ctrl Pts',(-1.01662486189503,-3.05983296337935,
41.4345784105186));
#31684=CARTESIAN_POINT('Ctrl Pts',(-0.920859674742334,-3.0883871230682,
41.44074984539));
#31685=CARTESIAN_POINT('Ctrl Pts',(-0.825193211592798,-3.1169118463717,
41.4469149181503));
#31686=CARTESIAN_POINT('Ctrl Pts',(-0.728099454503173,-3.14101735876284,
41.4530799909106));
#31687=CARTESIAN_POINT('Ctrl Pts',(-0.630022549005479,-3.16056785249813,
41.4592450636709));
#31688=CARTESIAN_POINT('Ctrl Pts',(-0.532013907618492,-3.1801047385746,
41.4654058453781));
#31689=CARTESIAN_POINT('Ctrl Pts',(-0.433023901818505,-3.19509282494601,
41.4715666270853));
#31690=CARTESIAN_POINT('Ctrl Pts',(-0.333509615403356,-3.20544675496779,
41.4777274087925));
#31691=CARTESIAN_POINT('Ctrl Pts',(-0.234030931931769,-3.21579698069343,
41.4838859863744));
#31692=CARTESIAN_POINT('Ctrl Pts',(-0.134028770862012,-3.22151629991976,
41.4900445639562));
#31693=CARTESIAN_POINT('Ctrl Pts',(-0.0339672538064622,-3.22257099040019,
41.4962031415381));
#31694=CARTESIAN_POINT('Ctrl Pts',(0.0660850270636717,-3.22362558352734,
41.502361150652));
#31695=CARTESIAN_POINT('Ctrl Pts',(0.166196220000049,-3.22001639951388,
41.5085191597658));
#31696=CARTESIAN_POINT('Ctrl Pts',(0.265901266663934,-3.21176183408523,
41.5146771688797));
#31697=CARTESIAN_POINT('Ctrl Pts',(0.365623577575643,-3.20350583935216,
41.5208362442726));
#31698=CARTESIAN_POINT('Ctrl Pts',(0.464939170920528,-3.19060290099849,
41.5269953196655));
#31699=CARTESIAN_POINT('Ctrl Pts',(0.563388166794329,-3.17312327778423,
41.5331543950584));
#31700=CARTESIAN_POINT('Ctrl Pts',(0.661943510286706,-3.15562477254597,
41.539320123673));
#31701=CARTESIAN_POINT('Ctrl Pts',(0.75962995985247,-3.13353978619853,41.5454858522876));
#31702=CARTESIAN_POINT('Ctrl Pts',(0.855997994093369,-3.10698970011298,
41.5516515809023));
#31703=CARTESIAN_POINT('Ctrl Pts',(0.95242092520818,-3.08042448954409,41.5578208218769));
#31704=CARTESIAN_POINT('Ctrl Pts',(1.0475235335995,-3.04938924786325,41.5639900628514));
#31705=CARTESIAN_POINT('Ctrl Pts',(1.14087360958332,-3.01405457307202,41.570159303826));
#31706=CARTESIAN_POINT('Ctrl Pts',(1.23437865913814,-2.97866123801002,41.5763387865631));
#31707=CARTESIAN_POINT('Ctrl Pts',(1.32612496744316,-2.93895438515914,41.5825182693002));
#31708=CARTESIAN_POINT('Ctrl Pts',(1.41570225115083,-2.89515193013881,41.5886977520372));
#31709=CARTESIAN_POINT('Ctrl Pts',(1.48062643598534,-2.86340461019075,41.5931765424492));
#31710=CARTESIAN_POINT('Ctrl Pts',(1.54441169411802,-2.82950680768233,41.5976553328612));
#31711=CARTESIAN_POINT('Ctrl Pts',(1.60691137623422,-2.79355568969531,41.6021341232732));
#31712=CARTESIAN_POINT('Ctrl Pts',(1.69211405879109,-2.74454533332714,41.6082398336511));
#31713=CARTESIAN_POINT('Ctrl Pts',(1.7752410144947,-2.69153627101615,41.614345544029));
#31714=CARTESIAN_POINT('Ctrl Pts',(1.85588634804178,-2.63473023773823,41.6204512544069));
#31715=CARTESIAN_POINT('Ctrl Pts',(1.9364206655874,-2.57800240338883,41.6265485596915));
#31716=CARTESIAN_POINT('Ctrl Pts',(2.0144797874966,-2.51748823444475,41.6326458649761));
#31717=CARTESIAN_POINT('Ctrl Pts',(2.08968262236008,-2.45343516325708,41.6387431702607));
#31718=CARTESIAN_POINT('Ctrl Pts',(2.16480531212943,-2.38945035464794,41.6448339775309));
#31719=CARTESIAN_POINT('Ctrl Pts',(2.23707742699188,-2.32193442402454,41.6509247848011));
#31720=CARTESIAN_POINT('Ctrl Pts',(2.30614799342743,-2.25117724644476,41.6570155920713));
#31721=CARTESIAN_POINT('Ctrl Pts',(2.37517089654546,-2.18046889605718,41.6631021962764));
#31722=CARTESIAN_POINT('Ctrl Pts',(2.4409963303577,-2.10652405872705,41.6691888004816));
#31723=CARTESIAN_POINT('Ctrl Pts',(2.50330825701889,-2.02967123762471,41.6752754046868));
#31724=CARTESIAN_POINT('Ctrl Pts',(2.56559822081552,-1.95284550456462,41.681359863568));
#31725=CARTESIAN_POINT('Ctrl Pts',(2.62437685666788,-1.87311416772567,41.6874443224494));
#31726=CARTESIAN_POINT('Ctrl Pts',(2.67936742746757,-1.79083995687102,41.6935287813306));
#31727=CARTESIAN_POINT('Ctrl Pts',(2.73435407531765,-1.70857161534231,41.6996128061552));
#31728=CARTESIAN_POINT('Ctrl Pts',(2.78555294787346,-1.62376112973534,41.7056968309798));
#31729=CARTESIAN_POINT('Ctrl Pts',(2.83273045137963,-1.53680049203746,41.7117808558044));
#31730=CARTESIAN_POINT('Ctrl Pts',(2.87991785314039,-1.44982160923401,41.7178661571109));
#31731=CARTESIAN_POINT('Ctrl Pts',(2.92308199852756,-1.36069206929212,41.7239514584173));
#31732=CARTESIAN_POINT('Ctrl Pts',(2.96203563656836,-1.26982772461428,41.7300367597237));
#31733=CARTESIAN_POINT('Ctrl Pts',(3.00103710447587,-1.17885181065272,41.7361295329677));
#31734=CARTESIAN_POINT('Ctrl Pts',(3.03581756728007,-1.08613724837081,41.7422223062117));
#31735=CARTESIAN_POINT('Ctrl Pts',(3.06623833561043,-0.992118960474475,
41.7483150794557));
#31736=CARTESIAN_POINT('Ctrl Pts',(3.09667812302572,-0.898041892281014,
41.7544116619056));
#31737=CARTESIAN_POINT('Ctrl Pts',(3.12275267596171,-0.802659905221281,
41.7605082443555));
#31738=CARTESIAN_POINT('Ctrl Pts',(3.1443741138857,-0.706419842887715,41.7666048268055));
#31739=CARTESIAN_POINT('Ctrl Pts',(3.16603678529099,-0.609996244527372,
41.7727130358327));
#31740=CARTESIAN_POINT('Ctrl Pts',(3.18322930403252,-0.51271174036668,41.7788212448598));
#31741=CARTESIAN_POINT('Ctrl Pts',(3.1959154811389,-0.415020240369924,41.784929453887));
#31742=CARTESIAN_POINT('Ctrl Pts',(3.20708758025298,-0.328988088097834,
41.7903086564702));
#31743=CARTESIAN_POINT('Ctrl Pts',(3.21476558175308,-0.242640549609535,
41.7956878590534));
#31744=CARTESIAN_POINT('Ctrl Pts',(3.21895823631987,-0.156286388813851,
41.8010670616366));
#31745=CARTESIAN_POINT('Ctrl Pts',(3.22148001842556,-0.104346412844581,
41.8043025241821));
#31746=CARTESIAN_POINT('Ctrl Pts',(3.22274422707167,-0.0523565586558018,
41.8075379867276));
#31747=CARTESIAN_POINT('Ctrl Pts',(3.22274998027534,-0.000356560338852404,
41.8107734492731));
#31748=CARTESIAN_POINT('Ctrl Pts',(1.43039598794072,-2.88162839993989,6.58668234580631));
#31749=CARTESIAN_POINT('Ctrl Pts',(2.3908869304735,-2.40485547853165,6.65299332526079));
#31750=CARTESIAN_POINT('Ctrl Pts',(3.78068485083689,-0.42330470969778,6.78561528416975));
#31751=CARTESIAN_POINT('Ctrl Pts',(2.39660828659712,2.9593008547868,6.98454822253319));
#31752=CARTESIAN_POINT('Ctrl Pts',(-1.19393826692811,3.61225397709376,7.18348116089663));
#31753=CARTESIAN_POINT('Ctrl Pts',(-3.68522155716544,0.949002744436199,
7.38241409926007));
#31754=CARTESIAN_POINT('Ctrl Pts',(-2.78953196244949,-2.58902355773568,
7.5813470376235));
#31755=CARTESIAN_POINT('Ctrl Pts',(0.671039291373588,-3.74572463321816,
7.78027997598695));
#31756=CARTESIAN_POINT('Ctrl Pts',(3.51448527473695,-1.45960212386322,7.97921291435037));
#31757=CARTESIAN_POINT('Ctrl Pts',(3.12717197768531,2.16867191230057,8.17814585271383));
#31758=CARTESIAN_POINT('Ctrl Pts',(-0.135028807280012,3.80310255787661,
8.37707879107726));
#31759=CARTESIAN_POINT('Ctrl Pts',(-3.27306356366253,1.94141424541036,8.5760117294407));
#31760=CARTESIAN_POINT('Ctrl Pts',(-3.40217358758694,-1.70507215059562,
8.77494466780414));
#31761=CARTESIAN_POINT('Ctrl Pts',(-0.403640923403273,-3.78405339475958,
8.97387760616759));
#31762=CARTESIAN_POINT('Ctrl Pts',(2.96595593022244,-2.38435003081143,9.172810544531));
#31763=CARTESIAN_POINT('Ctrl Pts',(3.60893852822567,1.20730380998424,9.37174348289446));
#31764=CARTESIAN_POINT('Ctrl Pts',(0.934206293343398,3.68907429945195,9.57067642125789));
#31765=CARTESIAN_POINT('Ctrl Pts',(-2.59934534842778,2.77946388606067,9.76960935962134));
#31766=CARTESIAN_POINT('Ctrl Pts',(-3.7433073822935,-0.685321221973841,
9.96854229798476));
#31767=CARTESIAN_POINT('Ctrl Pts',(-1.4460297930754,-3.52008693042821,10.1674752363482));
#31768=CARTESIAN_POINT('Ctrl Pts',(2.18058944266648,-3.11882102941849,10.3664081747117));
#31769=CARTESIAN_POINT('Ctrl Pts',(3.80258297155867,0.14959131214445,10.5653411130751));
#31770=CARTESIAN_POINT('Ctrl Pts',(1.92884471639216,3.28048361242447,10.7642740514386));
#31771=CARTESIAN_POINT('Ctrl Pts',(-1.71808921409888,3.39561249800469,10.963206989802));
#31772=CARTESIAN_POINT('Ctrl Pts',(-3.78557595114969,0.389139407006486,
11.1621399281654));
#31773=CARTESIAN_POINT('Ctrl Pts',(-2.37296555731667,-2.97507129439684,
11.3610728665289));
#31774=CARTESIAN_POINT('Ctrl Pts',(1.2211228251491,-3.60428547773973,11.5600058048923));
#31775=CARTESIAN_POINT('Ctrl Pts',(3.69262746162031,-0.920063684940536,
11.7589387432558));
#31776=CARTESIAN_POINT('Ctrl Pts',(2.76948293800576,2.60997682152157,11.9578716816192));
#31777=CARTESIAN_POINT('Ctrl Pts',(-0.699659800874596,3.74065380890841,
12.1568046199826));
#31778=CARTESIAN_POINT('Ctrl Pts',(-3.52560211426312,1.43253079764144,12.3557375583461));
#31779=CARTESIAN_POINT('Ctrl Pts',(-3.11044242675709,-2.19252426758155,
12.5546704967095));
#31780=CARTESIAN_POINT('Ctrl Pts',(0.164161079403195,-3.8019818377298,12.7536034350729));
#31781=CARTESIAN_POINT('Ctrl Pts',(3.2878505613498,-1.91626027473385,12.9525363734364));
#31782=CARTESIAN_POINT('Ctrl Pts',(3.38900412249117,1.73108804282604,13.1514693117998));
#31783=CARTESIAN_POINT('Ctrl Pts',(0.374630835682455,3.78703927775718,13.3504022501632));
#31784=CARTESIAN_POINT('Ctrl Pts',(-2.98414227610861,2.36154814268967,13.5493351885267));
#31785=CARTESIAN_POINT('Ctrl Pts',(-3.59957987005836,-1.23492490191512,
13.7482681268901));
#31786=CARTESIAN_POINT('Ctrl Pts',(-0.905907377036315,-3.69612588780959,
13.9472010652536));
#31787=CARTESIAN_POINT('Ctrl Pts',(2.6205698730494,-2.7594615950884,14.146134003617));
#31788=CARTESIAN_POINT('Ctrl Pts',(3.73794536304987,0.713988247211487,14.3450669419804));
#31789=CARTESIAN_POINT('Ctrl Pts',(1.41901074133174,3.53106545822759,14.5439998803439));
#31790=CARTESIAN_POINT('Ctrl Pts',(-2.2044268855072,3.10201819155779,14.7429328187073));
#31791=CARTESIAN_POINT('Ctrl Pts',(-3.8013248865683,-0.178728456209389,
14.9418657570708));
#31792=CARTESIAN_POINT('Ctrl Pts',(-1.90364769271949,-3.29516922422906,
15.1407986954342));
#31793=CARTESIAN_POINT('Ctrl Pts',(1.74406145191863,-3.38234599150264,15.3397316337976));
#31794=CARTESIAN_POINT('Ctrl Pts',(3.78844700014203,-0.360116760811474,
15.5386645721611));
#31795=CARTESIAN_POINT('Ctrl Pts',(2.35009605280664,2.993169440056,15.7375975105245));
#31796=CARTESIAN_POINT('Ctrl Pts',(-1.24870884594248,3.59482141035789,15.9365304488879));
#31797=CARTESIAN_POINT('Ctrl Pts',(-3.69957004376932,0.891737767254035,
16.1354633872514));
#31798=CARTESIAN_POINT('Ctrl Pts',(-2.74939973479973,-2.63112444642698,
16.3343963256148));
#31799=CARTESIAN_POINT('Ctrl Pts',(0.728306209987826,-3.73518203288617,
16.5333292639783));
#31800=CARTESIAN_POINT('Ctrl Pts',(3.53647695542546,-1.40546984956888,16.7322622023417));
#31801=CARTESIAN_POINT('Ctrl Pts',(3.09354840927974,2.21629713570752,16.9311951407051));
#31802=CARTESIAN_POINT('Ctrl Pts',(-0.193293208732243,3.80061212040383,
17.1301280790686));
#31803=CARTESIAN_POINT('Ctrl Pts',(-3.30243950399845,1.89100715935529,17.329061017432));
#31804=CARTESIAN_POINT('Ctrl Pts',(-3.37563819737945,-1.75700925287699,
17.5279939557954));
#31805=CARTESIAN_POINT('Ctrl Pts',(-0.345597398331251,-3.78979909659722,
17.7269268941589));
#31806=CARTESIAN_POINT('Ctrl Pts',(3.00215265516693,-2.33860945636005,17.9258598325223));
#31807=CARTESIAN_POINT('Ctrl Pts',(3.5900101677383,1.26247445512302,18.1247927708858));
#31808=CARTESIAN_POINT('Ctrl Pts',(0.877555064047497,3.70295987878172,18.3237257092492));
#31809=CARTESIAN_POINT('Ctrl Pts',(-2.6416403868901,2.73929750495517,18.5226586476126));
#31810=CARTESIAN_POINT('Ctrl Pts',(-3.73236385888241,-0.742613479012362,
18.7215915859761));
#31811=CARTESIAN_POINT('Ctrl Pts',(-1.39190832123119,-3.54183652637864,
18.9205245243395));
#31812=CARTESIAN_POINT('Ctrl Pts',(2.22813484392072,-3.085033204296,19.119457462703));
#31813=CARTESIAN_POINT('Ctrl Pts',(3.79984354968653,0.20785512312247,19.3183904010664));
#31814=CARTESIAN_POINT('Ctrl Pts',(1.87833886025086,3.30966129390517,19.5173233394298));
#31815=CARTESIAN_POINT('Ctrl Pts',(-1.76993125559216,3.36888083861398,19.7162562777933));
#31816=CARTESIAN_POINT('Ctrl Pts',(-3.79109554726769,0.331072961429409,
19.9151892161567));
#31817=CARTESIAN_POINT('Ctrl Pts',(-2.32708852200922,-3.01109178954004,
20.1141221545202));
#31818=CARTESIAN_POINT('Ctrl Pts',(1.27622152733633,-3.58514621284347,20.3130550928836));
#31819=CARTESIAN_POINT('Ctrl Pts',(3.70629534307339,-0.863359475661814,
20.511988031247));
#31820=CARTESIAN_POINT('Ctrl Pts',(2.72915505388636,2.65211754003269,20.7109209696104));
#31821=CARTESIAN_POINT('Ctrl Pts',(-0.756909844210963,3.729490882418,20.9098539079739));
#31822=CARTESIAN_POINT('Ctrl Pts',(-3.54714409239226,1.37832635544315,21.1087868463373));
#31823=CARTESIAN_POINT('Ctrl Pts',(-3.07647270163572,-2.23993983633326,
21.3077197847008));
#31824=CARTESIAN_POINT('Ctrl Pts',(0.222413985566929,-3.79901918570132,
21.5066527230642));
#31825=CARTESIAN_POINT('Ctrl Pts',(3.31683448791136,-1.86564298141534,21.7055856614276));
#31826=CARTESIAN_POINT('Ctrl Pts',(3.36207401442483,1.78282727032986,21.9045185997911));
#31827=CARTESIAN_POINT('Ctrl Pts',(0.316543663368888,3.79233633311756,22.1034515381545));
#31828=CARTESIAN_POINT('Ctrl Pts',(-3.01998671192163,2.31553341891654,22.3023844765179));
#31829=CARTESIAN_POINT('Ctrl Pts',(-3.58022961709107,-1.28994986073349,
22.5013174148814));
#31830=CARTESIAN_POINT('Ctrl Pts',(-0.849151210531485,-3.70957638766954,
22.7002503532448));
#31831=CARTESIAN_POINT('Ctrl Pts',(2.66255575201821,-2.71897253051539,22.8991832916083));
#31832=CARTESIAN_POINT('Ctrl Pts',(3.72656314567699,0.771195095669392,23.0981162299717));
#31833=CARTESIAN_POINT('Ctrl Pts',(1.3647241516294,3.55239957553509,23.2970491683351));
#31834=CARTESIAN_POINT('Ctrl Pts',(-2.25171193961186,3.06786702699317,23.4959821066986));
#31835=CARTESIAN_POINT('Ctrl Pts',(-3.79813904055242,-0.236969582297126,
23.694915045062));
#31836=CARTESIAN_POINT('Ctrl Pts',(-1.85291970926293,-3.32395898069267,
23.8938479834255));
#31837=CARTESIAN_POINT('Ctrl Pts',(1.79569710773726,-3.35521782475692,24.0927809217889));
#31838=CARTESIAN_POINT('Ctrl Pts',(3.79352143592832,-0.302009717484061,
24.2917138601523));
#31839=CARTESIAN_POINT('Ctrl Pts',(2.30394431674614,3.02883729170711,24.4906467985158));
#31840=CARTESIAN_POINT('Ctrl Pts',(-1.30365925374081,3.57526045267173,24.6895797368792));
#31841=CARTESIAN_POINT('Ctrl Pts',(-3.71280296439449,0.834930477277034,
24.8885126752426));
#31842=CARTESIAN_POINT('Ctrl Pts',(-2.70875008435262,-2.67295486958203,
25.0874456136061));
#31843=CARTESIAN_POINT('Ctrl Pts',(0.785469023636781,-3.72358069164743,
25.2863785519695));
#31844=CARTESIAN_POINT('Ctrl Pts',(3.55760289864069,-1.35110190951161,25.485311490333));
#31845=CARTESIAN_POINT('Ctrl Pts',(3.05921630672578,2.26345098090627,25.6842444286964));
#31846=CARTESIAN_POINT('Ctrl Pts',(-0.251521699592702,3.79720312716301,
25.8831773670599));
#31847=CARTESIAN_POINT('Ctrl Pts',(-3.33103466763993,1.84016923060991,26.0821103054233));
#31848=CARTESIAN_POINT('Ctrl Pts',(-3.34831237027993,-1.80854057884607,
26.2810432437867));
#31849=CARTESIAN_POINT('Ctrl Pts',(-0.287471337177379,-3.79465083829908,
26.4799761821502));
#31850=CARTESIAN_POINT('Ctrl Pts',(3.03764339894311,-2.29232138566123,26.6789091205136));
#31851=CARTESIAN_POINT('Ctrl Pts',(3.57023879254785,1.31734950506271,26.877842058877));
#31852=CARTESIAN_POINT('Ctrl Pts',(0.820697484702102,3.71597502587224,27.0767749972405));
#31853=CARTESIAN_POINT('Ctrl Pts',(-2.68331474003338,2.69848786549469,27.2757079356039));
#31854=CARTESIAN_POINT('Ctrl Pts',(-3.72054356412085,-0.799731418528385,
27.4746408739674));
#31855=CARTESIAN_POINT('Ctrl Pts',(-1.3374598291058,-3.56275398530838,27.6735738123308));
#31856=CARTESIAN_POINT('Ctrl Pts',(2.27515678785163,-3.05052066785249,27.8725067506942));
#31857=CARTESIAN_POINT('Ctrl Pts',(3.79621145927515,0.266070123784241,28.0714396890576));
#31858=CARTESIAN_POINT('Ctrl Pts',(1.82739173267215,3.33806144486047,28.2703726274211));
#31859=CARTESIAN_POINT('Ctrl Pts',(-1.82135749507502,3.34135775238698,28.4693055657845));
#31860=CARTESIAN_POINT('Ctrl Pts',(-3.79572452364676,0.272928735916584,
28.668238504148));
#31861=CARTESIAN_POINT('Ctrl Pts',(-2.28066479632187,-3.04640490432913,
28.8671714425114));
#31862=CARTESIAN_POINT('Ctrl Pts',(1.33102041368457,-3.56516471045272,29.0661043808749));
#31863=CARTESIAN_POINT('Ctrl Pts',(3.71909252552727,-0.806452441790404,
29.2650373192383));
#31864=CARTESIAN_POINT('Ctrl Pts',(2.68818602462228,2.69363521125782,29.4639702576017));
#31865=CARTESIAN_POINT('Ctrl Pts',(-0.81398207092878,3.71745180769153,29.6629031959652));
#31866=CARTESIAN_POINT('Ctrl Pts',(-3.56785275990456,1.32379811071928,29.8618361343286));
#31867=CARTESIAN_POINT('Ctrl Pts',(-3.04178023805176,-2.286829188571,30.060769072692));
#31868=CARTESIAN_POINT('Ctrl Pts',(0.280614641256556,-3.79516405144956,
30.2597020110555));
#31869=CARTESIAN_POINT('Ctrl Pts',(3.34503920917982,-1.81458740306222,30.4586349494189));
#31870=CARTESIAN_POINT('Ctrl Pts',(3.33435407319303,1.83414766823269,30.6575678877823));
#31871=CARTESIAN_POINT('Ctrl Pts',(0.258382127231354,3.7967424762064,30.8565008261458));
#31872=CARTESIAN_POINT('Ctrl Pts',(-3.05512167921966,2.26897471988225,31.0554337645092));
#31873=CARTESIAN_POINT('Ctrl Pts',(-3.56003828088928,-1.34467177887595,
31.2543667028727));
#31874=CARTESIAN_POINT('Ctrl Pts',(-0.792195557702424,-3.7221554175852,
31.4532996412361));
#31875=CARTESIAN_POINT('Ctrl Pts',(2.70391613171949,-2.67784471299768,31.6522325795996));
#31876=CARTESIAN_POINT('Ctrl Pts',(3.71430546775585,0.828220771595132,31.851165517963));
#31877=CARTESIAN_POINT('Ctrl Pts',(1.31011695494754,3.57289914756372,32.0500984563264));
#31878=CARTESIAN_POINT('Ctrl Pts',(-2.29846801167811,3.03299514565962,32.2490313946898));
#31879=CARTESIAN_POINT('Ctrl Pts',(-3.79406091906533,-0.295155038451869,
32.4479643330533));
#31880=CARTESIAN_POINT('Ctrl Pts',(-1.8017564297867,-3.35196785814317,32.6468972714167));
#31881=CARTESIAN_POINT('Ctrl Pts',(1.84691091052057,-3.32730143553342,32.8458302097802));
#31882=CARTESIAN_POINT('Ctrl Pts',(3.79770468103133,-0.243831724710034,
33.0447631481436));
#31883=CARTESIAN_POINT('Ctrl Pts',(2.25725132798827,3.06379359562579,33.2436960865071));
#31884=CARTESIAN_POINT('Ctrl Pts',(-1.35830340019312,3.55485957912918,33.4426290248705));
#31885=CARTESIAN_POINT('Ctrl Pts',(-3.72516365707354,0.777927041772669,
33.6415619632339));
#31886=CARTESIAN_POINT('Ctrl Pts',(-2.66746408246281,-2.71415735046314,
33.8404949015973));
#31887=CARTESIAN_POINT('Ctrl Pts',(0.842447311459858,-3.71110459051167,
34.0394278399608));
#31888=CARTESIAN_POINT('Ctrl Pts',(3.57789307418948,-1.29641656267163,34.2383607783242));
#31889=CARTESIAN_POINT('Ctrl Pts',(3.02416551966811,2.31007308627943,34.4372937166877));
#31890=CARTESIAN_POINT('Ctrl Pts',(-0.309691101873131,3.79290207832017,
34.6362266550511));
#31891=CARTESIAN_POINT('Ctrl Pts',(-3.35884729001673,1.78889900124255,34.8351595934145));
#31892=CARTESIAN_POINT('Ctrl Pts',(-3.32019994296254,-1.85964703453407,
35.034092531778));
#31893=CARTESIAN_POINT('Ctrl Pts',(-0.229277741996502,-3.79861112399583,
35.2330254701414));
#31894=CARTESIAN_POINT('Ctrl Pts',(3.07242052621671,-2.24549479277051,35.4319584085049));
#31895=CARTESIAN_POINT('Ctrl Pts',(3.54962868121306,1.37191507747408,35.6308913468683));
#31896=CARTESIAN_POINT('Ctrl Pts',(0.763647103503218,3.72811719983819,35.8298242852317));
#31897=CARTESIAN_POINT('Ctrl Pts',(-2.72435871711047,2.65704428540604,36.0287572235952));
#31898=CARTESIAN_POINT('Ctrl Pts',(-3.70784922296926,-0.856661481574834,
36.2276901619586));
#31899=CARTESIAN_POINT('Ctrl Pts',(-1.28269713503262,-3.58283446656971,
36.426623100322));
#31900=CARTESIAN_POINT('Ctrl Pts',(2.3216442419344,-3.01529148950444,36.6255560386855));
#31901=CARTESIAN_POINT('Ctrl Pts',(3.79168754631124,0.324222617667434,36.8244889770489));
#31902=CARTESIAN_POINT('Ctrl Pts',(1.77601530605909,3.36567740459321,37.0234219154124));
#31903=CARTESIAN_POINT('Ctrl Pts',(-1.8723558529673,3.31304969821073,37.2223548537758));
#31904=CARTESIAN_POINT('Ctrl Pts',(-3.7994617923675,0.214720395742962,37.4212877921392));
#31905=CARTESIAN_POINT('Ctrl Pts',(-2.23370528574428,-3.08100234999048,
37.6202207305027));
#31906=CARTESIAN_POINT('Ctrl Pts',(1.38550660873585,-3.54434565307739,37.8191536688661));
#31907=CARTESIAN_POINT('Ctrl Pts',(3.73101600658191,-0.749355973410843,
38.0180866072295));
#31908=CARTESIAN_POINT('Ctrl Pts',(2.64658546701708,2.7345201218469,38.217019545593));
#31909=CARTESIAN_POINT('Ctrl Pts',(-0.870863058265686,3.70453933627131,
38.4159524839564));
#31910=CARTESIAN_POINT('Ctrl Pts',(-3.58772328085212,1.26895902047793,38.6148854223199));
#31911=CARTESIAN_POINT('Ctrl Pts',(-3.00637313042353,-2.33318159065596,
38.8138183606833));
#31912=CARTESIAN_POINT('Ctrl Pts',(0.338749266911483,-3.79041680024323,
39.0127512990467));
#31913=CARTESIAN_POINT('Ctrl Pts',(3.37245830401273,-1.76310657017941,39.2116842374102));
#31914=CARTESIAN_POINT('Ctrl Pts',(3.30585041806794,1.88503916744779,39.4106171757737));
#31915=CARTESIAN_POINT('Ctrl Pts',(0.200160644147806,3.80025286079382,39.609550114137));
#31916=CARTESIAN_POINT('Ctrl Pts',(-3.08954036858721,2.2218902919993,39.8084830525005));
#31917=CARTESIAN_POINT('Ctrl Pts',(-3.53900783447175,-1.39909181671731,
40.0074159908639));
#31918=CARTESIAN_POINT('Ctrl Pts',(-0.735059111694563,-3.73383314394713,
40.2063489292274));
#31919=CARTESIAN_POINT('Ctrl Pts',(2.74465148416864,-2.63613934982058,40.4052818675907));
#31920=CARTESIAN_POINT('Ctrl Pts',(3.70115567014427,0.885150728230919,40.6042148059543));
#31921=CARTESIAN_POINT('Ctrl Pts',(1.25523944945949,3.59236978650378,40.8031477443176));
#31922=CARTESIAN_POINT('Ctrl Pts',(-2.34475597191911,2.99777433843635,41.0020806826812));
#31923=CARTESIAN_POINT('Ctrl Pts',(-3.78895369938313,-0.353968922753305,
41.2010136210445));
#31924=CARTESIAN_POINT('Ctrl Pts',(-1.75043395750614,-3.37784670177234,
41.399946559408));
#31925=CARTESIAN_POINT('Ctrl Pts',(1.89819598814578,-3.30121868695718,41.5988794977715));
#31926=CARTESIAN_POINT('Ctrl Pts',(3.80045064895368,-0.179534356723371,
41.7978556019462));
#31927=CARTESIAN_POINT('Ctrl Pts',(2.74058008982409,1.99769120286346,41.9305207266665));
#31928=CARTESIAN_POINT('Ctrl Pts',(1.86660756886202,2.62022723339283,41.9968748719324));
#31929=CARTESIAN_POINT('Ctrl Pts',(1.53698740838146,-3.09636394654476,6.72509367227838));
#31930=CARTESIAN_POINT('Ctrl Pts',(2.56905300209345,-2.58406246986299,6.79140465173286));
#31931=CARTESIAN_POINT('Ctrl Pts',(4.06241702282764,-0.454848876953752,
6.92402661064182));
#31932=CARTESIAN_POINT('Ctrl Pts',(2.5752007069213,3.17982446103466,7.12295954900526));
#31933=CARTESIAN_POINT('Ctrl Pts',(-1.28290913713704,3.88143487920559,7.32189248736869));
#31934=CARTESIAN_POINT('Ctrl Pts',(-3.9598399172061,1.01972130865502,7.52082542573213));
#31935=CARTESIAN_POINT('Ctrl Pts',(-2.9974045912523,-2.78195453691917,7.71975836409557));
#31936=CARTESIAN_POINT('Ctrl Pts',(0.721044347205764,-4.02485161106244,
7.91869130245901));
#31937=CARTESIAN_POINT('Ctrl Pts',(3.776380568565,-1.56836995107503,8.11762424082243));
#31938=CARTESIAN_POINT('Ctrl Pts',(3.36020514183989,2.33027878309083,8.3165571791859));
#31939=CARTESIAN_POINT('Ctrl Pts',(-0.145090994597224,4.08650527093188,
8.51549011754931));
#31940=CARTESIAN_POINT('Ctrl Pts',(-3.51696839657934,2.08608614314127,8.71442305591277));
#31941=CARTESIAN_POINT('Ctrl Pts',(-3.65569954707234,-1.83213211442255,
8.91335599427619));
#31942=CARTESIAN_POINT('Ctrl Pts',(-0.433719768517655,-4.06603658666688,
9.11228893263964));
#31943=CARTESIAN_POINT('Ctrl Pts',(3.18697546483547,-2.5620289803853,9.31122187100306));
#31944=CARTESIAN_POINT('Ctrl Pts',(3.87787236700172,1.2972706646837,9.51015480936652));
#31945=CARTESIAN_POINT('Ctrl Pts',(1.00382224349398,3.96397976129963,9.70908774772995));
#31946=CARTESIAN_POINT('Ctrl Pts',(-2.7930454952688,2.98658625369632,9.90802068609338));
#31947=CARTESIAN_POINT('Ctrl Pts',(-4.02225422945243,-0.736390550414543,
10.1069536244569));
#31948=CARTESIAN_POINT('Ctrl Pts',(-1.55378622621903,-3.78239965302563,
10.3058865628203));
#31949=CARTESIAN_POINT('Ctrl Pts',(2.34308439375097,-3.3512318907665,10.5048195011837));
#31950=CARTESIAN_POINT('Ctrl Pts',(4.08594696565489,0.160738680133138,10.7037524395472));
#31951=CARTESIAN_POINT('Ctrl Pts',(2.07257994765896,3.52494137861565,10.9026853779106));
#31952=CARTESIAN_POINT('Ctrl Pts',(-1.84611919413145,3.64864953283978,11.101618316274));
#31953=CARTESIAN_POINT('Ctrl Pts',(-4.06767260216181,0.418137616238003,
11.3005512546375));
#31954=CARTESIAN_POINT('Ctrl Pts',(-2.54979614936507,-3.19677009518745,
11.4994841930009));
#31955=CARTESIAN_POINT('Ctrl Pts',(1.31211945654531,-3.87287257668649,11.6984171313644));
#31956=CARTESIAN_POINT('Ctrl Pts',(3.96779770091828,-0.98862574460827,11.8973500697278));
#31957=CARTESIAN_POINT('Ctrl Pts',(2.97586153717486,2.80446921318709,12.0962830080912));
#31958=CARTESIAN_POINT('Ctrl Pts',(-0.75179762328831,4.01940291491122,12.2952159464547));
#31959=CARTESIAN_POINT('Ctrl Pts',(-3.78832582184925,1.53928130158088,12.4941488848181));
#31960=CARTESIAN_POINT('Ctrl Pts',(-3.34222892452571,-2.35590858772967,
12.6930818231815));
#31961=CARTESIAN_POINT('Ctrl Pts',(0.176394169248418,-4.08530103604272,
12.892014761545));
#31962=CARTESIAN_POINT('Ctrl Pts',(3.53285730387823,-2.05905772826418,13.0909476999084));
#31963=CARTESIAN_POINT('Ctrl Pts',(3.64154870898418,1.86008668023026,13.2898806382719));
#31964=CARTESIAN_POINT('Ctrl Pts',(0.402547883306248,4.06924497414062,13.4888135766353));
#31965=CARTESIAN_POINT('Ctrl Pts',(-3.20651703574811,2.53752792247832,13.6877465149988));
#31966=CARTESIAN_POINT('Ctrl Pts',(-3.86781631267568,-1.32695004777861,
13.8866794533622));
#31967=CARTESIAN_POINT('Ctrl Pts',(-0.973414525350525,-3.97155682569729,
14.0856123917256));
#31968=CARTESIAN_POINT('Ctrl Pts',(2.81585164640969,-2.96509341561348,14.284545330089));
#31969=CARTESIAN_POINT('Ctrl Pts',(4.01649263886463,0.767193808531516,14.4834782684525));
#31970=CARTESIAN_POINT('Ctrl Pts',(1.52475374663538,3.79419628775648,14.6824112068159));
#31971=CARTESIAN_POINT('Ctrl Pts',(-2.36869817469211,3.33317692526415,14.8813441451794));
#31972=CARTESIAN_POINT('Ctrl Pts',(-4.08459512965621,-0.192047089777438,
15.0802770835428));
#31973=CARTESIAN_POINT('Ctrl Pts',(-2.04550527152725,-3.54072134487557,
15.2792100219063));
#31974=CARTESIAN_POINT('Ctrl Pts',(1.87402685245334,-3.63439442193429,15.4781429602697));
#31975=CARTESIAN_POINT('Ctrl Pts',(4.07075759833579,-0.386952236709728,
15.6770758986331));
#31976=CARTESIAN_POINT('Ctrl Pts',(2.52522243637638,3.21621689329631,15.8760088369966));
#31977=CARTESIAN_POINT('Ctrl Pts',(-1.34176115504296,3.86270325817569,16.07494177536));
#31978=CARTESIAN_POINT('Ctrl Pts',(-3.97525763609332,0.958189012974472,
16.2738747137235));
#31979=CARTESIAN_POINT('Ctrl Pts',(-2.95428175737412,-2.8271927341357,16.4728076520868));
#31980=CARTESIAN_POINT('Ctrl Pts',(0.782578728991608,-4.01352338859924,
16.6717405904503));
#31981=CARTESIAN_POINT('Ctrl Pts',(3.80001104333727,-1.51020380360336,16.8706735288137));
#31982=CARTESIAN_POINT('Ctrl Pts',(3.3240759848093,2.38145298192455,17.0696064671772));
#31983=CARTESIAN_POINT('Ctrl Pts',(-0.207697190464619,4.08382924899859,
17.2685394055406));
#31984=CARTESIAN_POINT('Ctrl Pts',(-3.54853339731083,2.03192278053888,17.4674723439041));
#31985=CARTESIAN_POINT('Ctrl Pts',(-3.62718677091157,-1.88793950825425,
17.6664052822675));
#31986=CARTESIAN_POINT('Ctrl Pts',(-0.37135090847757,-4.07221045142267,
17.8653382206309));
#31987=CARTESIAN_POINT('Ctrl Pts',(3.22586952699263,-2.51287987232251,18.0642711589944));
#31988=CARTESIAN_POINT('Ctrl Pts',(3.85753348743574,1.35655256116935,18.2632040973578));
#31989=CARTESIAN_POINT('Ctrl Pts',(0.942949431467649,3.97890007760914,18.4621370357212));
#31990=CARTESIAN_POINT('Ctrl Pts',(-2.83849231006808,2.94342672128722,18.6610699740847));
#31991=CARTESIAN_POINT('Ctrl Pts',(-4.01049520759558,-0.797952158814143,
18.8600029124481));
#31992=CARTESIAN_POINT('Ctrl Pts',(-1.49563168618331,-3.80577000319091,
19.0589358508116));
#31993=CARTESIAN_POINT('Ctrl Pts',(2.3941728221794,-3.31492623680237,19.257868789175));
#31994=CARTESIAN_POINT('Ctrl Pts',(4.08300340529871,0.223344241524889,19.4568017275385));
#31995=CARTESIAN_POINT('Ctrl Pts',(2.01831045474011,3.55629334647608,19.6557346659019));
#31996=CARTESIAN_POINT('Ctrl Pts',(-1.90182444335736,3.61992586174797,19.8546676042653));
#31997=CARTESIAN_POINT('Ctrl Pts',(-4.07360351206664,0.355744127683883,
20.0536005426287));
#31998=CARTESIAN_POINT('Ctrl Pts',(-2.5005004115443,-3.23547479510659,20.2525334809922));
#31999=CARTESIAN_POINT('Ctrl Pts',(1.37132404897559,-3.85230707636404,20.4514664193556));
#32000=CARTESIAN_POINT('Ctrl Pts',(3.98248409676232,-0.927696004593339,
20.6503993577191));
#32001=CARTESIAN_POINT('Ctrl Pts',(2.93252846673791,2.84975020829459,20.8493322960825));
#32002=CARTESIAN_POINT('Ctrl Pts',(-0.813313872270502,4.00740814031659,
21.0482652344459));
#32003=CARTESIAN_POINT('Ctrl Pts',(-3.8114730827583,1.48103760833823,21.2471981728094));
#32004=CARTESIAN_POINT('Ctrl Pts',(-3.30572781558952,-2.40685750869074,
21.4461311111728));
#32005=CARTESIAN_POINT('Ctrl Pts',(0.238988013211991,-4.0821176106825,21.6450640495362));
#32006=CARTESIAN_POINT('Ctrl Pts',(3.56400107843168,-2.00466849400123,21.8439969878997));
#32007=CARTESIAN_POINT('Ctrl Pts',(3.61261180105568,1.91568145388957,22.0429299262631));
#32008=CARTESIAN_POINT('Ctrl Pts',(0.340132123483712,4.0749367598133,22.2418628646266));
#32009=CARTESIAN_POINT('Ctrl Pts',(-3.24503255660361,2.48808423580994,22.44079580299));
#32010=CARTESIAN_POINT('Ctrl Pts',(-3.84702410170021,-1.38607540157123,
22.6397287413534));
#32011=CARTESIAN_POINT('Ctrl Pts',(-0.912428956318338,-3.98600964092851,
22.8386616797169));
#32012=CARTESIAN_POINT('Ctrl Pts',(2.86096626351498,-2.92158715374577,23.0375946180803));
#32013=CARTESIAN_POINT('Ctrl Pts',(4.00426223208981,0.828663643803887,23.2365275564438));
#32014=CARTESIAN_POINT('Ctrl Pts',(1.46642178435367,3.81712019830084,23.4354604948072));
#32015=CARTESIAN_POINT('Ctrl Pts',(-2.4195068552087,3.29648085623159,23.6343934331707));
#32016=CARTESIAN_POINT('Ctrl Pts',(-4.08117187815611,-0.254628275827654,
23.8333263715341));
#32017=CARTESIAN_POINT('Ctrl Pts',(-1.99099709862783,-3.57165648000459,
24.0322593098975));
#32018=CARTESIAN_POINT('Ctrl Pts',(1.92951033638773,-3.60524469622744,24.2311922482609));
#32019=CARTESIAN_POINT('Ctrl Pts',(4.07621017508652,-0.324515125108852,
24.4301251866244));
#32020=CARTESIAN_POINT('Ctrl Pts',(2.47563152742672,3.2545426711466,24.6290581249878));
#32021=CARTESIAN_POINT('Ctrl Pts',(-1.40080640236154,3.84168464101443,24.8279910633513));
#32022=CARTESIAN_POINT('Ctrl Pts',(-3.98947665834203,0.897148510809323,
25.0269240017147));
#32023=CARTESIAN_POINT('Ctrl Pts',(-2.91060294296254,-2.8721403110435,25.2258569400782));
#32024=CARTESIAN_POINT('Ctrl Pts',(0.844001248033056,-4.00105752910675,
25.4247898784416));
#32025=CARTESIAN_POINT('Ctrl Pts',(3.82271126690174,-1.45178442883431,25.623722816805));
#32026=CARTESIAN_POINT('Ctrl Pts',(3.28718549450203,2.43212067600246,25.8226557551684));
#32027=CARTESIAN_POINT('Ctrl Pts',(-0.270264799725342,4.08016622160577,
26.0215886935319));
#32028=CARTESIAN_POINT('Ctrl Pts',(-3.57925943879032,1.97729646935751,26.2205216318953));
#32029=CARTESIAN_POINT('Ctrl Pts',(-3.59782465543471,-1.94331088780188,
26.4194545702588));
#32030=CARTESIAN_POINT('Ctrl Pts',(-0.308893361864258,-4.07742373918868,
26.6183875086222));
#32031=CARTESIAN_POINT('Ctrl Pts',(3.26400499909824,-2.46314246923822,26.8173204469857));
#32032=CARTESIAN_POINT('Ctrl Pts',(3.83628877270618,1.41551683505063,27.016253385349));
#32033=CARTESIAN_POINT('Ctrl Pts',(0.881854892429735,3.99288509809649,27.2151863237125));
#32034=CARTESIAN_POINT('Ctrl Pts',(-2.88327218681108,2.89957599566987,27.4141192620759));
#32035=CARTESIAN_POINT('Ctrl Pts',(-3.99779407842222,-0.859326459755243,
27.6130522004394));
#32036=CARTESIAN_POINT('Ctrl Pts',(-1.43712575670111,-3.82824620646707,
27.8119851388028));
#32037=CARTESIAN_POINT('Ctrl Pts',(2.44469878586269,-3.2778418668851,28.0109180771663));
#32038=CARTESIAN_POINT('Ctrl Pts',(4.07910065579756,0.285897355313241,28.2098510155297));
#32039=CARTESIAN_POINT('Ctrl Pts',(1.96356680735725,3.58680984315424,28.4087839538932));
#32040=CARTESIAN_POINT('Ctrl Pts',(-1.95708290549785,3.59035178762629,28.6077168922566));
#32041=CARTESIAN_POINT('Ctrl Pts',(-4.07857743430098,0.293267063125026,
28.80664983062));
#32042=CARTESIAN_POINT('Ctrl Pts',(-2.45061724462188,-3.27341940152267,
29.0055827689835));
#32043=CARTESIAN_POINT('Ctrl Pts',(1.43020648364449,-3.83083657600328,29.2045157073469));
#32044=CARTESIAN_POINT('Ctrl Pts',(3.99623491014561,-0.866548325736514,
29.4034486457103));
#32045=CARTESIAN_POINT('Ctrl Pts',(2.88850647377694,2.89436172736787,29.6023815840738));
#32046=CARTESIAN_POINT('Ctrl Pts',(-0.874639053949637,3.9944719279536,29.8013145224372));
#32047=CARTESIAN_POINT('Ctrl Pts',(-3.83372493572705,1.42244598318807,30.0002474608007));
#32048=CARTESIAN_POINT('Ctrl Pts',(-3.26845011057368,-2.45724100010441,
30.1991803991641));
#32049=CARTESIAN_POINT('Ctrl Pts',(0.301525713057809,-4.07797519637728,
30.3981133375275));
#32050=CARTESIAN_POINT('Ctrl Pts',(3.59430758223343,-1.94980831422029,30.5970462758909));
#32051=CARTESIAN_POINT('Ctrl Pts',(3.58282620252664,1.97082618726046,30.7959792142544));
#32052=CARTESIAN_POINT('Ctrl Pts',(0.277636458332829,4.07967124348368,30.9949121526178));
#32053=CARTESIAN_POINT('Ctrl Pts',(-3.2827857401879,2.4380560374861,31.1938450909813));
#32054=CARTESIAN_POINT('Ctrl Pts',(-3.82532813096051,-1.44487513245452,
31.3927780293447));
#32055=CARTESIAN_POINT('Ctrl Pts',(-0.851229035476529,-3.99952604530396,
31.5917109677081));
#32056=CARTESIAN_POINT('Ctrl Pts',(2.90540876988572,-2.877394539818,31.7906439060716));
#32057=CARTESIAN_POINT('Ctrl Pts',(3.99109112648016,0.889938805780879,31.989576844435));
#32058=CARTESIAN_POINT('Ctrl Pts',(1.4077453238388,3.83914737423731,32.1885097827985));
#32059=CARTESIAN_POINT('Ctrl Pts',(-2.46974713456985,3.25901036346728,32.3874427211619));
#32060=CARTESIAN_POINT('Ctrl Pts',(-4.07678985987002,-0.317149643487198,
32.5863756595253));
#32061=CARTESIAN_POINT('Ctrl Pts',(-1.93602119196322,-3.60175254593826,
32.7853085978888));
#32062=CARTESIAN_POINT('Ctrl Pts',(1.98454053129662,-3.57524801063428,32.9842415362522));
#32063=CARTESIAN_POINT('Ctrl Pts',(4.08070515067628,-0.262001776992349,
33.1831744746156));
#32064=CARTESIAN_POINT('Ctrl Pts',(2.42545903226761,3.29210387756742,33.3821074129791));
#32065=CARTESIAN_POINT('Ctrl Pts',(-1.45952256610013,3.81976351845869,33.5810403513425));
#32066=CARTESIAN_POINT('Ctrl Pts',(-4.00275845524774,0.835897246583656,
33.7799732897059));
#32067=CARTESIAN_POINT('Ctrl Pts',(-2.86624035694998,-2.91641315216041,
33.9789062280695));
#32068=CARTESIAN_POINT('Ctrl Pts',(0.905225490601913,-3.98765172364236,
34.1778391664328));
#32069=CARTESIAN_POINT('Ctrl Pts',(3.84451344237989,-1.3930239945038,34.3767721047963));
#32070=CARTESIAN_POINT('Ctrl Pts',(3.24952276417025,2.48221700563069,34.5757050431597));
#32071=CARTESIAN_POINT('Ctrl Pts',(-0.332768917194808,4.07554466368054,
34.7746379815232));
#32072=CARTESIAN_POINT('Ctrl Pts',(-3.60914462495387,1.92220564302213,34.9735709198866));
#32073=CARTESIAN_POINT('Ctrl Pts',(-3.56761732322031,-1.99822573623664,
35.17250385825));
#32074=CARTESIAN_POINT('Ctrl Pts',(-0.246363248667963,-4.08167914070044,
35.3714367966135));
#32075=CARTESIAN_POINT('Ctrl Pts',(3.30137367684192,-2.41282641392402,35.5703697349769));
#32076=CARTESIAN_POINT('Ctrl Pts',(3.81414282020493,1.47414856950349,35.7693026733403));
#32077=CARTESIAN_POINT('Ctrl Pts',(0.820553184171816,4.00593209253256,35.9682356117038));
#32078=CARTESIAN_POINT('Ctrl Pts',(-2.9273747126076,2.8550440889171,36.1671685500672));
#32079=CARTESIAN_POINT('Ctrl Pts',(-3.98415376995365,-0.920498883894049,
36.3661014884307));
#32080=CARTESIAN_POINT('Ctrl Pts',(-1.37828221131289,-3.849823061487,36.5650344267941));
#32081=CARTESIAN_POINT('Ctrl Pts',(2.49465043014533,-3.23998745175455,36.7639673651575));
#32082=CARTESIAN_POINT('Ctrl Pts',(4.07423962618006,0.348383304391666,36.962900303521));
#32083=CARTESIAN_POINT('Ctrl Pts',(1.90836187008279,3.61648371160565,37.1618332418844));
#32084=CARTESIAN_POINT('Ctrl Pts',(-2.01188160081678,3.55993425067045,37.3607661802478));
#32085=CARTESIAN_POINT('Ctrl Pts',(-4.08259319987495,0.230721106156537,
37.5596991186113));
#32086=CARTESIAN_POINT('Ctrl Pts',(-2.40015836675168,-3.31059500799247,
37.7586320569747));
#32087=CARTESIAN_POINT('Ctrl Pts',(1.48875292563011,-3.8084661070492,37.9575649953382));
#32088=CARTESIAN_POINT('Ctrl Pts',(4.00904691493279,-0.805197095935613,
38.1564979337016));
#32089=CARTESIAN_POINT('Ctrl Pts',(2.84380589172842,2.93829333322945,38.3554308720651));
#32090=CARTESIAN_POINT('Ctrl Pts',(-0.935758745314963,3.9805972344063,38.5543638104285));
#32091=CARTESIAN_POINT('Ctrl Pts',(-3.85507618443849,1.3635203486794,38.7532967487919));
#32092=CARTESIAN_POINT('Ctrl Pts',(-3.23040450708304,-2.50704752847379,
38.9522296871554));
#32093=CARTESIAN_POINT('Ctrl Pts',(0.363992462388689,-4.07287418561517,
39.1511626255188));
#32094=CARTESIAN_POINT('Ctrl Pts',(3.62376991564507,-1.8944911904441,39.3500955638822));
#32095=CARTESIAN_POINT('Ctrl Pts',(3.55219848867015,2.02551006091971,39.5490285022457));
#32096=CARTESIAN_POINT('Ctrl Pts',(0.215076379060282,4.08344321778653,39.7479614406091));
#32097=CARTESIAN_POINT('Ctrl Pts',(-3.31976926965591,2.38746293362043,39.9468943789726));
#32098=CARTESIAN_POINT('Ctrl Pts',(-3.80273052050235,-1.50335048727303,
40.145827317336));
#32099=CARTESIAN_POINT('Ctrl Pts',(-0.789834848961668,-4.01207398204883,
40.3447602556994));
#32100=CARTESIAN_POINT('Ctrl Pts',(2.94917967271135,-2.83258134221006,40.5436931940629));
#32101=CARTESIAN_POINT('Ctrl Pts',(3.97696142147388,0.951111115579423,40.7426261324263));
#32102=CARTESIAN_POINT('Ctrl Pts',(1.34877841142462,3.86006894220613,40.9415590707897));
#32103=CARTESIAN_POINT('Ctrl Pts',(-2.51948441896513,3.22116494326784,41.1404920091532));
#32104=CARTESIAN_POINT('Ctrl Pts',(-4.07130205620617,-0.380346269017061,
41.3394249475166));
#32105=CARTESIAN_POINT('Ctrl Pts',(-1.88087422963442,-3.62955985044473,
41.5383578858801));
#32106=CARTESIAN_POINT('Ctrl Pts',(2.0396473123645,-3.54722160642478,41.7372908242435));
#32107=CARTESIAN_POINT('Ctrl Pts',(4.08365574488659,-0.19291304504628,41.9362669284183));
#32108=CARTESIAN_POINT('Ctrl Pts',(2.94480488286648,2.14655679302897,42.0689320531386));
#32109=CARTESIAN_POINT('Ctrl Pts',(2.00570496136574,2.81548347365039,42.1352861984045));
#32110=CARTESIAN_POINT('Ctrl Pts',(1.6435788288222,-3.31109949314964,6.86350499875044));
#32111=CARTESIAN_POINT('Ctrl Pts',(2.74721907371341,-2.76326946119434,6.92981597820492));
#32112=CARTESIAN_POINT('Ctrl Pts',(4.34414919481839,-0.486393044209725,
7.06243793711388));
#32113=CARTESIAN_POINT('Ctrl Pts',(2.75379312724547,3.40034806728253,7.26137087547732));
#32114=CARTESIAN_POINT('Ctrl Pts',(-1.37188000734597,4.15061578131742,7.46030381384076));
#32115=CARTESIAN_POINT('Ctrl Pts',(-4.23445827724675,1.09043987287385,7.65923675220419));
#32116=CARTESIAN_POINT('Ctrl Pts',(-3.2052772200551,-2.97488551610267,7.85816969056764));
#32117=CARTESIAN_POINT('Ctrl Pts',(0.771049403037938,-4.30397858890673,
8.05710262893107));
#32118=CARTESIAN_POINT('Ctrl Pts',(4.03827586239305,-1.67713777828685,8.25603556729451));
#32119=CARTESIAN_POINT('Ctrl Pts',(3.59323830599447,2.49188565388108,8.45496850565795));
#32120=CARTESIAN_POINT('Ctrl Pts',(-0.155153181914435,4.36990798398716,
8.65390144402138));
#32121=CARTESIAN_POINT('Ctrl Pts',(-3.76087322949614,2.23075804087219,8.85283438238483));
#32122=CARTESIAN_POINT('Ctrl Pts',(-3.90922550655774,-1.95919207824947,
9.05176732074826));
#32123=CARTESIAN_POINT('Ctrl Pts',(-0.463798613632033,-4.34801977857419,
9.2507002591117));
#32124=CARTESIAN_POINT('Ctrl Pts',(3.40799499944848,-2.73970792995919,9.44963319747514));
#32125=CARTESIAN_POINT('Ctrl Pts',(4.14680620577778,1.38723751938316,9.64856613583857));
#32126=CARTESIAN_POINT('Ctrl Pts',(1.07343819364456,4.23888522314733,9.84749907420202));
#32127=CARTESIAN_POINT('Ctrl Pts',(-2.9867456421098,3.19370862133198,10.0464320125655));
#32128=CARTESIAN_POINT('Ctrl Pts',(-4.30120107661137,-0.787459878855247,
10.2453649509289));
#32129=CARTESIAN_POINT('Ctrl Pts',(-1.66154265936265,-4.04471237562304,
10.4442978892923));
#32130=CARTESIAN_POINT('Ctrl Pts',(2.50557934483546,-3.58364275211452,10.6432308276558));
#32131=CARTESIAN_POINT('Ctrl Pts',(4.36931095975112,0.171886048121829,10.8421637660192));
#32132=CARTESIAN_POINT('Ctrl Pts',(2.21631517892575,3.76939914480685,11.0410967043827));
#32133=CARTESIAN_POINT('Ctrl Pts',(-1.97414917416402,3.90168656767488,11.2400296427461));
#32134=CARTESIAN_POINT('Ctrl Pts',(-4.34976925317394,0.447135825469514,
11.4389625811095));
#32135=CARTESIAN_POINT('Ctrl Pts',(-2.72662674141349,-3.41846889597808,
11.6378955194729));
#32136=CARTESIAN_POINT('Ctrl Pts',(1.40311608794153,-4.14145967563326,11.8368284578364));
#32137=CARTESIAN_POINT('Ctrl Pts',(4.24296794021624,-1.057187804276,12.0357613961998));
#32138=CARTESIAN_POINT('Ctrl Pts',(3.18224013634397,2.99896160485262,12.2346943345633));
#32139=CARTESIAN_POINT('Ctrl Pts',(-0.803935445702029,4.29815202091405,
12.4336272729267));
#32140=CARTESIAN_POINT('Ctrl Pts',(-4.05104952943537,1.64603180552031,12.6325602112902));
#32141=CARTESIAN_POINT('Ctrl Pts',(-3.57401542229434,-2.51929290787779,
12.8314931496536));
#32142=CARTESIAN_POINT('Ctrl Pts',(0.18862725909364,-4.36862023435567,13.030426088017));
#32143=CARTESIAN_POINT('Ctrl Pts',(3.77786404640665,-2.20185518179452,13.2293590263804));
#32144=CARTESIAN_POINT('Ctrl Pts',(3.89409329547718,1.98908531763447,13.4282919647439));
#32145=CARTESIAN_POINT('Ctrl Pts',(0.430464930930045,4.35145067052408,13.6272249031073));
#32146=CARTESIAN_POINT('Ctrl Pts',(-3.42889179538761,2.71350770226696,13.8261578414708));
#32147=CARTESIAN_POINT('Ctrl Pts',(-4.13605275529299,-1.4189751936421,14.0250907798342));
#32148=CARTESIAN_POINT('Ctrl Pts',(-1.04092167366474,-4.246987763585,14.2240237181976));
#32149=CARTESIAN_POINT('Ctrl Pts',(3.01113341976998,-3.17072523613856,14.4229566565611));
#32150=CARTESIAN_POINT('Ctrl Pts',(4.29503991467939,0.820399369851541,14.6218895949245));
#32151=CARTESIAN_POINT('Ctrl Pts',(1.63049675193903,4.05732711728536,14.820822533288));
#32152=CARTESIAN_POINT('Ctrl Pts',(-2.53296946387702,3.56433565897051,15.0197554716514));
#32153=CARTESIAN_POINT('Ctrl Pts',(-4.36786537274413,-0.205365723345486,
15.2186884100148));
#32154=CARTESIAN_POINT('Ctrl Pts',(-2.18736285033501,-3.7862734655221,15.4176213483783));
#32155=CARTESIAN_POINT('Ctrl Pts',(2.00399225298804,-3.88644285236594,15.6165542867417));
#32156=CARTESIAN_POINT('Ctrl Pts',(4.35306819652955,-0.41378771260799,15.8154872251052));
#32157=CARTESIAN_POINT('Ctrl Pts',(2.70034881994612,3.43926434653661,16.0144201634686));
#32158=CARTESIAN_POINT('Ctrl Pts',(-1.43481346414344,4.13058510599347,16.213353101832));
#32159=CARTESIAN_POINT('Ctrl Pts',(-4.25094522841732,1.02464025869492,16.4122860401955));
#32160=CARTESIAN_POINT('Ctrl Pts',(-3.15916377994851,-3.02326102184444,
16.6112189785589));
#32161=CARTESIAN_POINT('Ctrl Pts',(0.836851247995388,-4.29186474431231,
16.8101519169224));
#32162=CARTESIAN_POINT('Ctrl Pts',(4.06354513124908,-1.61493775763784,17.0090848552858));
#32163=CARTESIAN_POINT('Ctrl Pts',(3.55460356033887,2.54660882814157,17.2080177936493));
#32164=CARTESIAN_POINT('Ctrl Pts',(-0.222101172196999,4.36704637759334,
17.4069507320126));
#32165=CARTESIAN_POINT('Ctrl Pts',(-3.79462729062322,2.17283840172248,17.6058836703761));
#32166=CARTESIAN_POINT('Ctrl Pts',(-3.87873534444371,-2.0188697636315,17.8048166087395));
#32167=CARTESIAN_POINT('Ctrl Pts',(-0.397104418623892,-4.35462180624813,
18.003749547103));
#32168=CARTESIAN_POINT('Ctrl Pts',(3.44958639881833,-2.68715028828496,18.2026824854664));
#32169=CARTESIAN_POINT('Ctrl Pts',(4.12505680713318,1.45063066721568,18.4016154238299));
#32170=CARTESIAN_POINT('Ctrl Pts',(1.00834379888781,4.25484027643657,18.6005483621933));
#32171=CARTESIAN_POINT('Ctrl Pts',(-3.03534423324606,3.14755593761926,18.7994813005568));
#32172=CARTESIAN_POINT('Ctrl Pts',(-4.28862655630873,-0.853290838615923,
18.9984142389201));
#32173=CARTESIAN_POINT('Ctrl Pts',(-1.59935505113543,-4.06970348000317,
19.1973471772837));
#32174=CARTESIAN_POINT('Ctrl Pts',(2.56021080043808,-3.54481926930875,19.396280115647));
#32175=CARTESIAN_POINT('Ctrl Pts',(4.36616326091091,0.238833359927311,19.5952130540105));
#32176=CARTESIAN_POINT('Ctrl Pts',(2.15828204922935,3.802925399047,19.7941459923739));
#32177=CARTESIAN_POINT('Ctrl Pts',(-2.03371763112254,3.87097088488195,19.9930789307374));
#32178=CARTESIAN_POINT('Ctrl Pts',(-4.3561114768656,0.380415293938357,20.1920118691008));
#32179=CARTESIAN_POINT('Ctrl Pts',(-2.67391230107938,-3.45985780067314,
20.3909448074643));
#32180=CARTESIAN_POINT('Ctrl Pts',(1.46642657061485,-4.11946793988461,20.5898777458277));
#32181=CARTESIAN_POINT('Ctrl Pts',(4.25867285045125,-0.992032533524869,
20.7888106841911));
#32182=CARTESIAN_POINT('Ctrl Pts',(3.13590187958944,3.0473828765565,20.9877436225545));
#32183=CARTESIAN_POINT('Ctrl Pts',(-0.869717900330041,4.28532539821516,
21.186676560918));
#32184=CARTESIAN_POINT('Ctrl Pts',(-4.07580207312432,1.58374886123332,21.3856094992814));
#32185=CARTESIAN_POINT('Ctrl Pts',(-3.53498292954331,-2.57377518104822,
21.5845424376449));
#32186=CARTESIAN_POINT('Ctrl Pts',(0.255562040857054,-4.36521603566368,
21.7834753760083));
#32187=CARTESIAN_POINT('Ctrl Pts',(3.81116766895198,-2.14369400658712,21.9824083143717));
#32188=CARTESIAN_POINT('Ctrl Pts',(3.86314958768654,2.04853563744927,22.1813412527352));
#32189=CARTESIAN_POINT('Ctrl Pts',(0.363720583598531,4.35753718650904,22.3802741910986));
#32190=CARTESIAN_POINT('Ctrl Pts',(-3.47007840128558,2.66063505270333,22.5792071294621));
#32191=CARTESIAN_POINT('Ctrl Pts',(-4.11381858630935,-1.48220094240897,
22.7781400678255));
#32192=CARTESIAN_POINT('Ctrl Pts',(-0.975706702105193,-4.26244289418747,
22.9770730061889));
#32193=CARTESIAN_POINT('Ctrl Pts',(3.05937677501175,-3.12420177697617,23.1760059445524));
#32194=CARTESIAN_POINT('Ctrl Pts',(4.28196131850264,0.886132191938384,23.3749388829158));
#32195=CARTESIAN_POINT('Ctrl Pts',(1.56811941707795,4.08184082106659,23.5738718212792));
#32196=CARTESIAN_POINT('Ctrl Pts',(-2.58730177080555,3.52509468547,23.7728047596427));
#32197=CARTESIAN_POINT('Ctrl Pts',(-4.3642047157598,-0.272286969358187,
23.9717376980061));
#32198=CARTESIAN_POINT('Ctrl Pts',(-2.12907448799273,-3.81935397931651,
24.1706706363695));
#32199=CARTESIAN_POINT('Ctrl Pts',(2.06332356503822,-3.85527156769798,24.369603574733));
#32200=CARTESIAN_POINT('Ctrl Pts',(4.3588989142447,-0.347020532733638,24.5685365130964));
#32201=CARTESIAN_POINT('Ctrl Pts',(2.6473187381073,3.4802480505861,24.7674694514599));
#32202=CARTESIAN_POINT('Ctrl Pts',(-1.49795355098226,4.10810882935714,24.9664023898233));
#32203=CARTESIAN_POINT('Ctrl Pts',(-4.26615035228957,0.959366544341607,
25.1653353281867));
#32204=CARTESIAN_POINT('Ctrl Pts',(-3.11245580157246,-3.07132575250498,
25.3642682665502));
#32205=CARTESIAN_POINT('Ctrl Pts',(0.902533472429329,-4.27853436656609,
25.5632012049136));
#32206=CARTESIAN_POINT('Ctrl Pts',(4.0878196351628,-1.55246694815701,25.7621341432771));
#32207=CARTESIAN_POINT('Ctrl Pts',(3.51515468227829,2.60079037109864,25.9610670816405));
#32208=CARTESIAN_POINT('Ctrl Pts',(-0.289007899857984,4.36312931604853,
26.160000020004));
#32209=CARTESIAN_POINT('Ctrl Pts',(-3.8274842099407,2.11442370810511,26.3589329583674));
#32210=CARTESIAN_POINT('Ctrl Pts',(-3.8473369405895,-2.07808119675769,26.5578658967308));
#32211=CARTESIAN_POINT('Ctrl Pts',(-0.330315386551131,-4.36019664007829,
26.7567988350943));
#32212=CARTESIAN_POINT('Ctrl Pts',(3.49036659925336,-2.6339635528152,26.9557317734577));
#32213=CARTESIAN_POINT('Ctrl Pts',(4.10233875286451,1.51368416503854,27.1546647118211));
#32214=CARTESIAN_POINT('Ctrl Pts',(0.943012300157368,4.26979517032074,27.3535976501846));
#32215=CARTESIAN_POINT('Ctrl Pts',(-3.08322963358878,3.10066412584504,27.552530588548));
#32216=CARTESIAN_POINT('Ctrl Pts',(-4.27504459272359,-0.9189215009821,27.7514635269115));
#32217=CARTESIAN_POINT('Ctrl Pts',(-1.53679168429643,-4.09373842762575,
27.9503964652748));
#32218=CARTESIAN_POINT('Ctrl Pts',(2.61424078387375,-3.50516306591769,28.1493294036383));
#32219=CARTESIAN_POINT('Ctrl Pts',(4.36198985231999,0.305724586842239,28.3482623420017));
#32220=CARTESIAN_POINT('Ctrl Pts',(2.09974188204234,3.835558241448,28.5471952803652));
#32221=CARTESIAN_POINT('Ctrl Pts',(-2.09280831592068,3.83934582286561,28.7461282187286));
#32222=CARTESIAN_POINT('Ctrl Pts',(-4.36143034495521,0.313605390333471,
28.9450611570921));
#32223=CARTESIAN_POINT('Ctrl Pts',(-2.62056969292188,-3.50043389871622,
29.1439940954555));
#32224=CARTESIAN_POINT('Ctrl Pts',(1.52939255360441,-4.09650844155383,29.342927033819));
#32225=CARTESIAN_POINT('Ctrl Pts',(4.27337729476395,-0.926644209682624,
29.5418599721824));
#32226=CARTESIAN_POINT('Ctrl Pts',(3.08882692293162,3.09508824347791,29.7407929105458));
#32227=CARTESIAN_POINT('Ctrl Pts',(-0.935296036970499,4.27149204821567,
29.9397258489092));
#32228=CARTESIAN_POINT('Ctrl Pts',(-4.09959711154953,1.52109385565686,30.1386587872727));
#32229=CARTESIAN_POINT('Ctrl Pts',(-3.49511998309561,-2.62765281163783,
30.3375917256362));
#32230=CARTESIAN_POINT('Ctrl Pts',(0.322436784859063,-4.360786341305,30.5365246639996));
#32231=CARTESIAN_POINT('Ctrl Pts',(3.84357595528703,-2.08502922537836,30.735457602363));
#32232=CARTESIAN_POINT('Ctrl Pts',(3.83129833186026,2.10750470628822,30.9343905407264));
#32233=CARTESIAN_POINT('Ctrl Pts',(0.296890789434302,4.36260001076095,31.1333234790899));
#32234=CARTESIAN_POINT('Ctrl Pts',(-3.51044980115615,2.60713735508994,31.3322564174533));
#32235=CARTESIAN_POINT('Ctrl Pts',(-4.09061798103173,-1.54507848603308,
31.5311893558168));
#32236=CARTESIAN_POINT('Ctrl Pts',(-0.910262513250637,-4.27689667302272,
31.7301222941802));
#32237=CARTESIAN_POINT('Ctrl Pts',(3.10690140805196,-3.07694436663831,31.9290552325437));
#32238=CARTESIAN_POINT('Ctrl Pts',(4.26787678520448,0.951656839966625,32.127988170907));
#32239=CARTESIAN_POINT('Ctrl Pts',(1.50537369273006,4.10539560091092,32.3269211092706));
#32240=CARTESIAN_POINT('Ctrl Pts',(-2.64102625746159,3.48502558127492,32.5258540476339));
#32241=CARTESIAN_POINT('Ctrl Pts',(-4.35951880067472,-0.339144248522522,
32.7247869859974));
#32242=CARTESIAN_POINT('Ctrl Pts',(-2.07028595413972,-3.85153723373335,
32.9237199243608));
#32243=CARTESIAN_POINT('Ctrl Pts',(2.12217015207268,-3.82319458573513,33.1226528627243));
#32244=CARTESIAN_POINT('Ctrl Pts',(4.36370562032123,-0.280171829274663,
33.3215858010877));
#32245=CARTESIAN_POINT('Ctrl Pts',(2.59366673654697,3.52041415950907,33.5205187394511));
#32246=CARTESIAN_POINT('Ctrl Pts',(-1.56074173200713,4.08466745778821,33.7194516778146));
#32247=CARTESIAN_POINT('Ctrl Pts',(-4.28035325342194,0.893867451394637,
33.9183846161781));
#32248=CARTESIAN_POINT('Ctrl Pts',(-3.06501663143715,-3.11866895385767,
34.1173175545414));
#32249=CARTESIAN_POINT('Ctrl Pts',(0.968003669743968,-4.26419885677308,
34.3162504929049));
#32250=CARTESIAN_POINT('Ctrl Pts',(4.11113381057032,-1.48963142633595,34.5151834312683));
#32251=CARTESIAN_POINT('Ctrl Pts',(3.47488000867237,2.65436092498193,34.7141163696317));
#32252=CARTESIAN_POINT('Ctrl Pts',(-0.355846732516481,4.35818724904092,
34.9130493079952));
#32253=CARTESIAN_POINT('Ctrl Pts',(-3.85944195989102,2.05551228480171,35.1119822463586));
#32254=CARTESIAN_POINT('Ctrl Pts',(-3.81503470347808,-2.13680443793921,
35.3109151847221));
#32255=CARTESIAN_POINT('Ctrl Pts',(-0.263448755339423,-4.36474715740505,
35.5098481230855));
#32256=CARTESIAN_POINT('Ctrl Pts',(3.53032682746711,-2.58015803507752,35.708781061449));
#32257=CARTESIAN_POINT('Ctrl Pts',(4.07865695919681,1.5763820615329,35.9077139998124));
#32258=CARTESIAN_POINT('Ctrl Pts',(0.87745926484041,4.28374698522694,36.1066469381758));
#32259=CARTESIAN_POINT('Ctrl Pts',(-3.13039070810472,3.05304389242815,36.3055798765393));
#32260=CARTESIAN_POINT('Ctrl Pts',(-4.26045831693806,-0.984336286213261,
36.5045128149027));
#32261=CARTESIAN_POINT('Ctrl Pts',(-1.47386728759316,-4.11681165640429,
36.7034457532661));
#32262=CARTESIAN_POINT('Ctrl Pts',(2.66765661835625,-3.46468341400465,36.9023786916296));
#32263=CARTESIAN_POINT('Ctrl Pts',(4.35679170604889,0.372543991115891,37.101311629993));
#32264=CARTESIAN_POINT('Ctrl Pts',(2.04070843410648,3.86729001861809,37.3002445683564));
#32265=CARTESIAN_POINT('Ctrl Pts',(-2.15140734866625,3.80681880313016,37.4991775067199));
#32266=CARTESIAN_POINT('Ctrl Pts',(-4.3657246073824,0.246721816570115,37.6981104450834));
#32267=CARTESIAN_POINT('Ctrl Pts',(-2.56661144775907,-3.54018766599446,
37.8970433834468));
#32268=CARTESIAN_POINT('Ctrl Pts',(1.59199924252436,-4.07258656102101,38.0959763218102));
#32269=CARTESIAN_POINT('Ctrl Pts',(4.28707782328367,-0.861038218460384,
38.2949092601736));
#32270=CARTESIAN_POINT('Ctrl Pts',(3.04102631643975,3.14206654461201,38.4938421985371));
#32271=CARTESIAN_POINT('Ctrl Pts',(-1.00065443236423,4.25665513254129,38.6927751369005));
#32272=CARTESIAN_POINT('Ctrl Pts',(-4.12242908802487,1.45808167688089,38.8917080752639));
#32273=CARTESIAN_POINT('Ctrl Pts',(-3.45443588374254,-2.68091346629163,
39.0906410136274));
#32274=CARTESIAN_POINT('Ctrl Pts',(0.389235657865896,-4.35533157098711,
39.2895739519908));
#32275=CARTESIAN_POINT('Ctrl Pts',(3.8750815272774,-2.02587581070879,39.4885068903542));
#32276=CARTESIAN_POINT('Ctrl Pts',(3.79854655927238,2.16598095439164,39.6874398287178));
#32277=CARTESIAN_POINT('Ctrl Pts',(0.22999211397275,4.36663357477926,39.8863727670811));
#32278=CARTESIAN_POINT('Ctrl Pts',(-3.5499981707246,2.55303557524153,40.0853057054446));
#32279=CARTESIAN_POINT('Ctrl Pts',(-4.06645320653296,-1.60760915782874,
40.284238643808));
#32280=CARTESIAN_POINT('Ctrl Pts',(-0.844610586228765,-4.29031482015054,
40.4831715821715));
#32281=CARTESIAN_POINT('Ctrl Pts',(3.15370786125407,-3.02902333459953,40.6821045205349));
#32282=CARTESIAN_POINT('Ctrl Pts',(4.2527671728035,1.01707150292793,40.8810374588983));
#32283=CARTESIAN_POINT('Ctrl Pts',(1.44231737338975,4.12776809790848,41.0799703972618));
#32284=CARTESIAN_POINT('Ctrl Pts',(-2.69421286601115,3.44455554809932,41.2789033356252));
#32285=CARTESIAN_POINT('Ctrl Pts',(-4.3536504130292,-0.406723615280815,
41.4778362739886));
#32286=CARTESIAN_POINT('Ctrl Pts',(-2.0113145017627,-3.88127299911711,41.6767692123521));
#32287=CARTESIAN_POINT('Ctrl Pts',(2.18109863658322,-3.79322452589238,41.8757021507155));
#32288=CARTESIAN_POINT('Ctrl Pts',(4.3668608408195,-0.206291733369188,42.0746782548904));
#32289=CARTESIAN_POINT('Ctrl Pts',(3.14902967590887,2.29542238319448,42.2073433796106));
#32290=CARTESIAN_POINT('Ctrl Pts',(2.14480235386948,3.01073971390795,42.2736975248765));
#32291=CARTESIAN_POINT('Ctrl Pts',(1.75017024926294,-3.52583503975451,7.00191632522251));
#32292=CARTESIAN_POINT('Ctrl Pts',(2.92538514533336,-2.94247645252568,7.06822730467699));
#32293=CARTESIAN_POINT('Ctrl Pts',(4.62588136680913,-0.517937211465701,
7.20084926358595));
#32294=CARTESIAN_POINT('Ctrl Pts',(2.93238554756965,3.6208716735304,7.39978220194938));
#32295=CARTESIAN_POINT('Ctrl Pts',(-1.46085087755489,4.41979668342923,7.59871514031282));
#32296=CARTESIAN_POINT('Ctrl Pts',(-4.5090766372874,1.16115843709268,7.79764807867627));
#32297=CARTESIAN_POINT('Ctrl Pts',(-3.4131498488579,-3.16781649528616,7.99658101703969));
#32298=CARTESIAN_POINT('Ctrl Pts',(0.821054458870111,-4.58310556675101,
8.19551395540314));
#32299=CARTESIAN_POINT('Ctrl Pts',(4.30017115622109,-1.78590560549867,8.39444689376657));
#32300=CARTESIAN_POINT('Ctrl Pts',(3.82627147014904,2.65349252467134,8.59337983213001));
#32301=CARTESIAN_POINT('Ctrl Pts',(-0.165215369231643,4.65331069704242,
8.79231277049345));
#32302=CARTESIAN_POINT('Ctrl Pts',(-4.00477806241297,2.37542993860311,8.99124570885689));
#32303=CARTESIAN_POINT('Ctrl Pts',(-4.16275146604314,-2.0862520420764,9.19017864722033));
#32304=CARTESIAN_POINT('Ctrl Pts',(-0.493877458746418,-4.63000297048149,
9.38911158558376));
#32305=CARTESIAN_POINT('Ctrl Pts',(3.62901453406151,-2.91738687953307,9.5880445239472));
#32306=CARTESIAN_POINT('Ctrl Pts',(4.41574004455383,1.47720437408262,9.78697746231064));
#32307=CARTESIAN_POINT('Ctrl Pts',(1.14305414379514,4.513790684995,9.98591040067408));
#32308=CARTESIAN_POINT('Ctrl Pts',(-3.18044578895083,3.40083098896765,10.1848433390375));
#32309=CARTESIAN_POINT('Ctrl Pts',(-4.58014792377031,-0.838529207295953,
10.3837762774009));
#32310=CARTESIAN_POINT('Ctrl Pts',(-1.76929909250628,-4.30702509822045,
10.5827092157644));
#32311=CARTESIAN_POINT('Ctrl Pts',(2.66807429591995,-3.81605361346254,10.7816421541278));
#32312=CARTESIAN_POINT('Ctrl Pts',(4.65267495384734,0.183033416110524,10.9805750924913));
#32313=CARTESIAN_POINT('Ctrl Pts',(2.36005041019255,4.01385691099803,11.1795080308547));
#32314=CARTESIAN_POINT('Ctrl Pts',(-2.10217915419658,4.15472360250998,11.3784409692181));
#32315=CARTESIAN_POINT('Ctrl Pts',(-4.63186590418606,0.476134034701025,
11.5773739075816));
#32316=CARTESIAN_POINT('Ctrl Pts',(-2.90345733346189,-3.6401676967687,11.776306845945));
#32317=CARTESIAN_POINT('Ctrl Pts',(1.49411271933775,-4.41004677458003,11.9752397843084));
#32318=CARTESIAN_POINT('Ctrl Pts',(4.51813817951421,-1.12574986394373,12.1741727226719));
#32319=CARTESIAN_POINT('Ctrl Pts',(3.38861873551307,3.19345399651813,12.3731056610353));
#32320=CARTESIAN_POINT('Ctrl Pts',(-0.856073268115742,4.57690112691687,
12.5720385993988));
#32321=CARTESIAN_POINT('Ctrl Pts',(-4.3137732370215,1.75278230945974,12.7709715377622));
#32322=CARTESIAN_POINT('Ctrl Pts',(-3.80580192006295,-2.68267722802591,
12.9699044761256));
#32323=CARTESIAN_POINT('Ctrl Pts',(0.200860348938858,-4.6519394326686,13.1688374144891));
#32324=CARTESIAN_POINT('Ctrl Pts',(4.0228707889351,-2.34465263532486,13.3677703528525));
#32325=CARTESIAN_POINT('Ctrl Pts',(4.14663788197017,2.11808395503869,13.566703291216));
#32326=CARTESIAN_POINT('Ctrl Pts',(0.458381978553845,4.63365636690753,13.7656362295794));
#32327=CARTESIAN_POINT('Ctrl Pts',(-3.65126655502712,2.88948748205561,13.9645691679428));
#32328=CARTESIAN_POINT('Ctrl Pts',(-4.4042891979103,-1.51100033950559,14.1635021063063));
#32329=CARTESIAN_POINT('Ctrl Pts',(-1.10842882197895,-4.52241870147271,
14.3624350446697));
#32330=CARTESIAN_POINT('Ctrl Pts',(3.20641519313028,-3.37635705666365,14.5613679830331));
#32331=CARTESIAN_POINT('Ctrl Pts',(4.57358719049415,0.873604931171569,14.7603009213966));
#32332=CARTESIAN_POINT('Ctrl Pts',(1.73623975724267,4.32045794681424,14.95923385976));
#32333=CARTESIAN_POINT('Ctrl Pts',(-2.69724075306194,3.79549439267688,15.1581667981235));
#32334=CARTESIAN_POINT('Ctrl Pts',(-4.65113561583202,-0.218684356913533,
15.3570997364869));
#32335=CARTESIAN_POINT('Ctrl Pts',(-2.32922042914278,-4.03182558616862,
15.5560326748503));
#32336=CARTESIAN_POINT('Ctrl Pts',(2.13395765352274,-4.13849128279759,15.7549656132138));
#32337=CARTESIAN_POINT('Ctrl Pts',(4.63537879472331,-0.44062318850625,15.9538985515772));
#32338=CARTESIAN_POINT('Ctrl Pts',(2.87547520351587,3.66231179977693,16.1528314899406));
#32339=CARTESIAN_POINT('Ctrl Pts',(-1.52786577324392,4.39846695381126,16.3517644283041));
#32340=CARTESIAN_POINT('Ctrl Pts',(-4.52663282074132,1.09109150441536,16.5506973666675));
#32341=CARTESIAN_POINT('Ctrl Pts',(-3.36404580252289,-3.21932930955316,
16.749630305031));
#32342=CARTESIAN_POINT('Ctrl Pts',(0.891123766999176,-4.57020610002538,
16.9485632433944));
#32343=CARTESIAN_POINT('Ctrl Pts',(4.32707921916088,-1.71967171167232,17.1474961817578));
#32344=CARTESIAN_POINT('Ctrl Pts',(3.78513113586845,2.7117646743586,17.3464291201213));
#32345=CARTESIAN_POINT('Ctrl Pts',(-0.236505153929377,4.65026350618809,
17.5453620584847));
#32346=CARTESIAN_POINT('Ctrl Pts',(-4.0407211839356,2.31375402290608,17.7442949968481));
#32347=CARTESIAN_POINT('Ctrl Pts',(-4.13028391797584,-2.14980001900876,
17.9432279352116));
#32348=CARTESIAN_POINT('Ctrl Pts',(-0.422857928770215,-4.63703316107358,
18.142160873575));
#32349=CARTESIAN_POINT('Ctrl Pts',(3.67330327064404,-2.86142070424742,18.3410938119385));
#32350=CARTESIAN_POINT('Ctrl Pts',(4.39258012683063,1.544708773262,18.5400267503019));
#32351=CARTESIAN_POINT('Ctrl Pts',(1.07373816630795,4.53078047526401,18.7389596886653));
#32352=CARTESIAN_POINT('Ctrl Pts',(-3.23219615642406,3.35168515395129,18.9378926270288));
#32353=CARTESIAN_POINT('Ctrl Pts',(-4.56675790502189,-0.9086295184177,19.1368255653922));
#32354=CARTESIAN_POINT('Ctrl Pts',(-1.70307841608756,-4.33363695681545,
19.3357585037557));
#32355=CARTESIAN_POINT('Ctrl Pts',(2.72624877869676,-3.77471230181512,19.5346914421191));
#32356=CARTESIAN_POINT('Ctrl Pts',(4.6493231165231,0.254322478329726,19.7336243804825));
#32357=CARTESIAN_POINT('Ctrl Pts',(2.2982536437186,4.04955745161791,19.932557318846));
#32358=CARTESIAN_POINT('Ctrl Pts',(-2.16561081888772,4.12201590801593,20.1314902572094));
#32359=CARTESIAN_POINT('Ctrl Pts',(-4.63861944166455,0.405086460192834,
20.3304231955728));
#32360=CARTESIAN_POINT('Ctrl Pts',(-2.84732419061446,-3.68424080623969,
20.5293561339363));
#32361=CARTESIAN_POINT('Ctrl Pts',(1.56152909225411,-4.38662880340519,20.7282890722997));
#32362=CARTESIAN_POINT('Ctrl Pts',(4.53486160414019,-1.05636906245639,20.9272220106632));
#32363=CARTESIAN_POINT('Ctrl Pts',(3.33927529244099,3.24501554481841,21.1261549490266));
#32364=CARTESIAN_POINT('Ctrl Pts',(-0.926121928389577,4.56324265611374,
21.32508788739));
#32365=CARTESIAN_POINT('Ctrl Pts',(-4.34013106349035,1.68646011412841,21.5240208257534));
#32366=CARTESIAN_POINT('Ctrl Pts',(-3.76423804349709,-2.74069285340571,
21.7229537641169));
#32367=CARTESIAN_POINT('Ctrl Pts',(0.272136068502114,-4.64831446064486,
21.9218867024803));
#32368=CARTESIAN_POINT('Ctrl Pts',(4.05833425947229,-2.282719519173,22.1208196408438));
#32369=CARTESIAN_POINT('Ctrl Pts',(4.1136873743174,2.18138982100898,22.3197525792072));
#32370=CARTESIAN_POINT('Ctrl Pts',(0.387309043713353,4.64013761320478,22.5186855175706));
#32371=CARTESIAN_POINT('Ctrl Pts',(-3.69512424596756,2.83318586959673,22.7176184559341));
#32372=CARTESIAN_POINT('Ctrl Pts',(-4.38061307091849,-1.5783264832467,22.9165513942975));
#32373=CARTESIAN_POINT('Ctrl Pts',(-1.03898444789204,-4.53887614744645,
23.115484332661));
#32374=CARTESIAN_POINT('Ctrl Pts',(3.25778728650852,-3.32681640020656,23.3144172710244));
#32375=CARTESIAN_POINT('Ctrl Pts',(4.55966040491547,0.943600740072882,23.5133502093879));
#32376=CARTESIAN_POINT('Ctrl Pts',(1.66981704980222,4.34656144383233,23.7122831477513));
#32377=CARTESIAN_POINT('Ctrl Pts',(-2.7550966864024,3.75370851470842,23.9112160861147));
#32378=CARTESIAN_POINT('Ctrl Pts',(-4.6472375533635,-0.289945662888717,
24.1101490244782));
#32379=CARTESIAN_POINT('Ctrl Pts',(-2.26715187735763,-4.06705147862843,
24.3090819628416));
#32380=CARTESIAN_POINT('Ctrl Pts',(2.19713679368869,-4.10529843916849,24.508014901205));
#32381=CARTESIAN_POINT('Ctrl Pts',(4.6415876534029,-0.369525940358427,24.7069478395685));
#32382=CARTESIAN_POINT('Ctrl Pts',(2.81900594878788,3.70595343002559,24.9058807779319));
#32383=CARTESIAN_POINT('Ctrl Pts',(-1.59510069960298,4.37453301769984,25.1048137162954));
#32384=CARTESIAN_POINT('Ctrl Pts',(-4.54282404623711,1.02158457787389,25.3037466546588));
#32385=CARTESIAN_POINT('Ctrl Pts',(-3.31430866018239,-3.27051119396646,
25.5026795930222));
#32386=CARTESIAN_POINT('Ctrl Pts',(0.961065696825607,-4.55601120402541,
25.7016125313856));
#32387=CARTESIAN_POINT('Ctrl Pts',(4.35292800342385,-1.65314946747969,25.9005454697491));
#32388=CARTESIAN_POINT('Ctrl Pts',(3.74312387005455,2.76946006619482,26.0994784081125));
#32389=CARTESIAN_POINT('Ctrl Pts',(-0.307750999990631,4.64609241049128,
26.298411346476));
#32390=CARTESIAN_POINT('Ctrl Pts',(-4.0757089810911,2.25155094685271,26.4973442848394));
#32391=CARTESIAN_POINT('Ctrl Pts',(-4.09684922574428,-2.21285150571349,
26.6962772232029));
#32392=CARTESIAN_POINT('Ctrl Pts',(-0.351737411238005,-4.64296954096788,
26.8952101615663));
#32393=CARTESIAN_POINT('Ctrl Pts',(3.71672819940849,-2.8047846363922,27.0941430999298));
#32394=CARTESIAN_POINT('Ctrl Pts',(4.36838873302285,1.61185149502644,27.2930760382932));
#32395=CARTESIAN_POINT('Ctrl Pts',(1.00416970788501,4.54670524254498,27.4920089766566));
#32396=CARTESIAN_POINT('Ctrl Pts',(-3.28318708036648,3.30175225602021,27.69094191502));
#32397=CARTESIAN_POINT('Ctrl Pts',(-4.55229510702496,-0.97851654220896,
27.8898748533835));
#32398=CARTESIAN_POINT('Ctrl Pts',(-1.63645761189174,-4.35923064878442,
28.0888077917469));
#32399=CARTESIAN_POINT('Ctrl Pts',(2.78378278188482,-3.7324842649503,28.2877407301104));
#32400=CARTESIAN_POINT('Ctrl Pts',(4.6448790488424,0.32555181837124,28.4866736684738));
#32401=CARTESIAN_POINT('Ctrl Pts',(2.23591695672744,4.08430663974176,28.6856066068372));
#32402=CARTESIAN_POINT('Ctrl Pts',(-2.22853372634353,4.08833985810493,28.8845395452007));
#32403=CARTESIAN_POINT('Ctrl Pts',(-4.64428325560944,0.333943717541912,
29.0834724835641));
#32404=CARTESIAN_POINT('Ctrl Pts',(-2.79052214122188,-3.72744839590976,
29.2824054219276));
#32405=CARTESIAN_POINT('Ctrl Pts',(1.62857862356433,-4.36218030710437,29.481338360291));
#32406=CARTESIAN_POINT('Ctrl Pts',(4.55051967938229,-0.986740093628734,
29.6802712986544));
#32407=CARTESIAN_POINT('Ctrl Pts',(3.28914737208629,3.29581475958795,29.8792042370179));
#32408=CARTESIAN_POINT('Ctrl Pts',(-0.995953019991353,4.54851216847773,
30.0781371753813));
#32409=CARTESIAN_POINT('Ctrl Pts',(-4.36546928737203,1.61974172812565,30.2770701137447));
#32410=CARTESIAN_POINT('Ctrl Pts',(-3.72178985561752,-2.79806462317125,
30.4760030521082));
#32411=CARTESIAN_POINT('Ctrl Pts',(0.343347856660311,-4.64359748623272,
30.6749359904716));
#32412=CARTESIAN_POINT('Ctrl Pts',(4.09284432834063,-2.22025013653641,30.8738689288351));
#32413=CARTESIAN_POINT('Ctrl Pts',(4.07977046119387,2.24418322531598,31.0728018671985));
#32414=CARTESIAN_POINT('Ctrl Pts',(0.316145120535775,4.64552877803824,31.2717348055619));
#32415=CARTESIAN_POINT('Ctrl Pts',(-3.73811386212439,2.77621867269378,31.4706677439254));
#32416=CARTESIAN_POINT('Ctrl Pts',(-4.35590783110296,-1.64528183961164,
31.6696006822888));
#32417=CARTESIAN_POINT('Ctrl Pts',(-0.969295991024743,-4.55426730074148,
31.8685336206522));
#32418=CARTESIAN_POINT('Ctrl Pts',(3.30839404621819,-3.27649419345861,32.0674665590156));
#32419=CARTESIAN_POINT('Ctrl Pts',(4.54466244392879,1.01337487415237,32.2663994973791));
#32420=CARTESIAN_POINT('Ctrl Pts',(1.60300206162132,4.3716438275845,32.4653324357425));
#32421=CARTESIAN_POINT('Ctrl Pts',(-2.81230538035333,3.71104079908257,32.664265374106));
#32422=CARTESIAN_POINT('Ctrl Pts',(-4.64224774147941,-0.361138853557849,
32.8631983124694));
#32423=CARTESIAN_POINT('Ctrl Pts',(-2.20455071631624,-4.10132192152844,
33.0621312508329));
#32424=CARTESIAN_POINT('Ctrl Pts',(2.25979977284874,-4.07114116083598,33.2610641891963));
#32425=CARTESIAN_POINT('Ctrl Pts',(4.64670608996618,-0.298341881556976,
33.4599971275598));
#32426=CARTESIAN_POINT('Ctrl Pts',(2.76187444082632,3.74872444145071,33.6589300659231));
#32427=CARTESIAN_POINT('Ctrl Pts',(-1.66196089791414,4.34957139711773,33.8578630042867));
#32428=CARTESIAN_POINT('Ctrl Pts',(-4.55794805159614,0.951837656205623,
34.05679594265));
#32429=CARTESIAN_POINT('Ctrl Pts',(-3.26379290592433,-3.32092475555494,
34.2557288810135));
#32430=CARTESIAN_POINT('Ctrl Pts',(1.03078184888602,-4.54074598990379,34.4546618193769));
#32431=CARTESIAN_POINT('Ctrl Pts',(4.37775417876074,-1.58623885816811,34.6535947577404));
#32432=CARTESIAN_POINT('Ctrl Pts',(3.70023725317449,2.82650484433319,34.8525276961038));
#32433=CARTESIAN_POINT('Ctrl Pts',(-0.378924547838154,4.64082983440129,
35.0514606344673));
#32434=CARTESIAN_POINT('Ctrl Pts',(-4.10973929482816,2.18881892658129,35.2503935728307));
#32435=CARTESIAN_POINT('Ctrl Pts',(-4.06245208373585,-2.27538313964179,
35.4493265111941));
#32436=CARTESIAN_POINT('Ctrl Pts',(-0.280534262010886,-4.64781517410965,
35.6482594495575));
#32437=CARTESIAN_POINT('Ctrl Pts',(3.75927997809232,-2.74748965623102,35.847192387921));
#32438=CARTESIAN_POINT('Ctrl Pts',(4.34317109818868,1.67861555356232,36.0461253262844));
#32439=CARTESIAN_POINT('Ctrl Pts',(0.934365345509009,4.56156187792131,36.2450582646479));
#32440=CARTESIAN_POINT('Ctrl Pts',(-3.33340670360185,3.25104369593922,36.4439912030113));
#32441=CARTESIAN_POINT('Ctrl Pts',(-4.53676286392246,-1.04817368853247,
36.6429241413748));
#32442=CARTESIAN_POINT('Ctrl Pts',(-1.56945236387344,-4.38380025132158,
36.8418570797382));
#32443=CARTESIAN_POINT('Ctrl Pts',(2.84066280656719,-3.68937937625476,37.0407900181016));
#32444=CARTESIAN_POINT('Ctrl Pts',(4.63934378591771,0.396704677840125,37.239722956465));
#32445=CARTESIAN_POINT('Ctrl Pts',(2.17305499813018,4.11809632563053,37.4386558948285));
#32446=CARTESIAN_POINT('Ctrl Pts',(-2.29093309651572,4.05370335558988,37.6375888331919));
#32447=CARTESIAN_POINT('Ctrl Pts',(-4.64885601488985,0.262722526983691,
37.8365217715554));
#32448=CARTESIAN_POINT('Ctrl Pts',(-2.73306452876649,-3.76978032399644,
38.0354547099188));
#32449=CARTESIAN_POINT('Ctrl Pts',(1.69524555941862,-4.33670701499282,38.2343876482823));
#32450=CARTESIAN_POINT('Ctrl Pts',(4.56510873163454,-0.91687934098516,38.4333205866457));
#32451=CARTESIAN_POINT('Ctrl Pts',(3.23824674115109,3.34583975599457,38.6322535250092));
#32452=CARTESIAN_POINT('Ctrl Pts',(-1.0655501194135,4.53271303067627,38.8311864633726));
#32453=CARTESIAN_POINT('Ctrl Pts',(-4.38978199161124,1.55264300508237,39.030119401736));
#32454=CARTESIAN_POINT('Ctrl Pts',(-3.67846726040206,-2.85477940410947,
39.2290523400994));
#32455=CARTESIAN_POINT('Ctrl Pts',(0.414478853343105,-4.63778895635907,
39.4279852784629));
#32456=CARTESIAN_POINT('Ctrl Pts',(4.12639313890974,-2.15726043097348,39.6269182168263));
#32457=CARTESIAN_POINT('Ctrl Pts',(4.04489462987461,2.30645184786356,39.8258511551898));
#32458=CARTESIAN_POINT('Ctrl Pts',(0.244907848885221,4.64982393177198,40.0247840935532));
#32459=CARTESIAN_POINT('Ctrl Pts',(-3.7802270717933,2.71860821686265,40.2237170319166));
#32460=CARTESIAN_POINT('Ctrl Pts',(-4.33017589256357,-1.71186782838445,
40.4226499702801));
#32461=CARTESIAN_POINT('Ctrl Pts',(-0.899386323495868,-4.56855565825224,
40.6215829086435));
#32462=CARTESIAN_POINT('Ctrl Pts',(3.35823604979678,-3.22546532698901,40.820515847007));
#32463=CARTESIAN_POINT('Ctrl Pts',(4.52857292413312,1.08303189027643,41.0194487853703));
#32464=CARTESIAN_POINT('Ctrl Pts',(1.53585633535487,4.39546725361082,41.2183817237339));
#32465=CARTESIAN_POINT('Ctrl Pts',(-2.86894131305717,3.66794615293081,41.4173146620972));
#32466=CARTESIAN_POINT('Ctrl Pts',(-4.63599876985225,-0.433100961544568,
41.6162476004607));
#32467=CARTESIAN_POINT('Ctrl Pts',(-2.14175477389098,-4.13298614778951,
41.8151805388241));
#32468=CARTESIAN_POINT('Ctrl Pts',(2.32254996080195,-4.03922744535998,42.0141134771876));
#32469=CARTESIAN_POINT('Ctrl Pts',(4.65006593675241,-0.219670421692099,
42.2130895813624));
#32470=CARTESIAN_POINT('Ctrl Pts',(3.35325446895125,2.44428797335999,42.3457547060828));
#32471=CARTESIAN_POINT('Ctrl Pts',(2.28389974637321,3.20599595416551,42.4121088513486));
#32472=CARTESIAN_POINT('Ctrl Pts',(1.75279798770009,-3.52836018667712,42.));
#32473=CARTESIAN_POINT('Ctrl Pts',(1.82143554149094,-3.48681209294754,42.0000000000001));
#32474=CARTESIAN_POINT('Ctrl Pts',(1.8885815825096,-3.44308219441033,42.0000000000001));
#32475=CARTESIAN_POINT('Ctrl Pts',(1.95412305121373,-3.3971702788484,42.0000000000001));
#32476=CARTESIAN_POINT('Ctrl Pts',(2.05256290803176,-3.32821298381799,42.0000000000001));
#32477=CARTESIAN_POINT('Ctrl Pts',(2.14738503498556,-3.25433510156145,42.0000000000001));
#32478=CARTESIAN_POINT('Ctrl Pts',(2.23843406813092,-3.17595253897366,42.));
#32479=CARTESIAN_POINT('Ctrl Pts',(2.33061707260172,-3.09659375977688,42.));
#32480=CARTESIAN_POINT('Ctrl Pts',(2.41893285168275,-3.01261656500042,42.));
#32481=CARTESIAN_POINT('Ctrl Pts',(2.50317836884662,-2.92441884813481,42.));
#32482=CARTESIAN_POINT('Ctrl Pts',(2.58733330463444,-2.83631596207834,42.));
#32483=CARTESIAN_POINT('Ctrl Pts',(2.66742707573242,-2.74400073281455,42.));
#32484=CARTESIAN_POINT('Ctrl Pts',(2.74321006647546,-2.64784937809448,42.));
#32485=CARTESIAN_POINT('Ctrl Pts',(2.77126704941009,-2.61225145708249,42.));
#32486=CARTESIAN_POINT('Ctrl Pts',(2.79873266663842,-2.5761275893848,42.));
#32487=CARTESIAN_POINT('Ctrl Pts',(2.82559245821946,-2.53949653137926,42.));
#32488=CARTESIAN_POINT('Ctrl Pts',(2.83828839352235,-2.52218196878813,42.));
#32489=CARTESIAN_POINT('Ctrl Pts',(2.85085105627574,-2.50475098317605,42.));
#32490=CARTESIAN_POINT('Ctrl Pts',(2.86326365969319,-2.48722741801918,42.));
#32491=CARTESIAN_POINT('Ctrl Pts',(2.93259154223295,-2.38935337612672,42.));
#32492=CARTESIAN_POINT('Ctrl Pts',(2.99733691489821,-2.28846731280446,42.));
#32493=CARTESIAN_POINT('Ctrl Pts',(3.05733405014049,-2.18496333662957,42.));
#32494=CARTESIAN_POINT('Ctrl Pts',(3.1172049553746,-2.08167712598138,42.));
#32495=CARTESIAN_POINT('Ctrl Pts',(3.17234788189958,-1.975783114258,42.));
#32496=CARTESIAN_POINT('Ctrl Pts',(3.22255028201254,-1.86765340308612,42.));
#32497=CARTESIAN_POINT('Ctrl Pts',(3.27167533988857,-1.76184415278164,42.));
#32498=CARTESIAN_POINT('Ctrl Pts',(3.31606975722882,-1.65389331291347,42.));
#32499=CARTESIAN_POINT('Ctrl Pts',(3.35548570303569,-1.54414347432169,42.));
#32500=CARTESIAN_POINT('Ctrl Pts',(3.38624649344917,-1.45849306777363,41.9999999999999));
#32501=CARTESIAN_POINT('Ctrl Pts',(3.41397424609095,-1.3717467549663,42.));
#32502=CARTESIAN_POINT('Ctrl Pts',(3.43852910267749,-1.28406938692554,42.));
#32503=CARTESIAN_POINT('Ctrl Pts',(3.44533961773349,-1.25975126342081,42.));
#32504=CARTESIAN_POINT('Ctrl Pts',(3.45190592873417,-1.23536153850306,42.));
#32505=CARTESIAN_POINT('Ctrl Pts',(3.45822477341065,-1.21090379238842,42.));
#32506=CARTESIAN_POINT('Ctrl Pts',(3.46235621786795,-1.19491260653134,42.));
#32507=CARTESIAN_POINT('Ctrl Pts',(3.4663797310686,-1.17890055560633,42.));
#32508=CARTESIAN_POINT('Ctrl Pts',(3.47029389106376,-1.16287225647867,42.));
#32509=CARTESIAN_POINT('Ctrl Pts',(3.49750979687016,-1.05142441586034,42.));
#32510=CARTESIAN_POINT('Ctrl Pts',(3.5194575163352,-0.939135267477813,42.));
#32511=CARTESIAN_POINT('Ctrl Pts',(3.5359436815247,-0.826341686230967,41.9999999999999));
#32512=CARTESIAN_POINT('Ctrl Pts',(3.55198728298497,-0.716575998213669,
42.));
#32513=CARTESIAN_POINT('Ctrl Pts',(3.56285862720728,-0.606331891956589,
42.));
#32514=CARTESIAN_POINT('Ctrl Pts',(3.56833123257986,-0.495921126813228,
42.));
#32515=CARTESIAN_POINT('Ctrl Pts',(3.57365916987809,-0.388429065229428,
42.));
#32516=CARTESIAN_POINT('Ctrl Pts',(3.57387001615029,-0.280778481168261,
41.9999999999999));
#32517=CARTESIAN_POINT('Ctrl Pts',(3.56870842791254,-0.173267408887965,
42.));
#32518=CARTESIAN_POINT('Ctrl Pts',(3.5653222936604,-0.102737388366562,42.));
#32519=CARTESIAN_POINT('Ctrl Pts',(3.55962285067617,-0.0322676353425919,
42.));
#32520=CARTESIAN_POINT('Ctrl Pts',(3.55165143284768,0.0380520659533637,
42.));
#32521=CARTESIAN_POINT('Ctrl Pts',(3.54710154953435,0.0781887696624734,
42.));
#32522=CARTESIAN_POINT('Ctrl Pts',(3.54181137670787,0.118276518513767,42.));
#32523=CARTESIAN_POINT('Ctrl Pts',(3.53578772847455,0.158297966652038,42.));
#32524=CARTESIAN_POINT('Ctrl Pts',(3.53344572120281,0.173858390988625,42.));
#32525=CARTESIAN_POINT('Ctrl Pts',(3.53099300975283,0.18940721262173,42.));
#32526=CARTESIAN_POINT('Ctrl Pts',(3.52843217698487,0.204931472988267,42.));
#32527=CARTESIAN_POINT('Ctrl Pts',(3.51031326577749,0.314771794722974,42.));
#32528=CARTESIAN_POINT('Ctrl Pts',(3.48676167369221,0.42354871924747,42.));
#32529=CARTESIAN_POINT('Ctrl Pts',(3.45802915101404,0.530939049228676,42.));
#32530=CARTESIAN_POINT('Ctrl Pts',(3.42903674042542,0.639300733127319,42.));
#32531=CARTESIAN_POINT('Ctrl Pts',(3.39476873131307,0.746251421507866,42.));
#32532=CARTESIAN_POINT('Ctrl Pts',(3.35543440096621,0.851438324429188,42.));
#32533=CARTESIAN_POINT('Ctrl Pts',(3.31638563898292,0.955861567426199,42.));
#32534=CARTESIAN_POINT('Ctrl Pts',(3.27234323949019,1.05854724171231,42.));
#32535=CARTESIAN_POINT('Ctrl Pts',(3.22347219448623,1.15911873378746,42.));
#32536=CARTESIAN_POINT('Ctrl Pts',(3.18696786157772,1.23424082760639,42.));
#32537=CARTESIAN_POINT('Ctrl Pts',(3.14776858641996,1.30818275664874,42.));
#32538=CARTESIAN_POINT('Ctrl Pts',(3.10593149822866,1.3807724923263,42.));
#32539=CARTESIAN_POINT('Ctrl Pts',(3.09665122555106,1.39687429505223,42.));
#32540=CARTESIAN_POINT('Ctrl Pts',(3.08724034026875,1.41291082564143,42.));
#32541=CARTESIAN_POINT('Ctrl Pts',(3.07770186971861,1.42887599560449,42.));
#32542=CARTESIAN_POINT('Ctrl Pts',(3.02142512756762,1.52307010656646,42.));
#32543=CARTESIAN_POINT('Ctrl Pts',(2.96086891636547,1.61451905005572,42.));
#32544=CARTESIAN_POINT('Ctrl Pts',(2.8962164722944,1.70287781084587,42.));
#32545=CARTESIAN_POINT('Ctrl Pts',(2.83191557546761,1.79075612144872,42.));
#32546=CARTESIAN_POINT('Ctrl Pts',(2.76356229636571,1.87557839552669,42.));
#32547=CARTESIAN_POINT('Ctrl Pts',(2.69130548220896,1.95696485393201,42.));
#32548=CARTESIAN_POINT('Ctrl Pts',(2.66190509140716,1.9900799823945,42.));
#32549=CARTESIAN_POINT('Ctrl Pts',(2.63185812650358,2.02262576678383,42.));
#32550=CARTESIAN_POINT('Ctrl Pts',(2.60117344348306,2.05457433130465,42.));
#32551=CARTESIAN_POINT('Ctrl Pts',(2.58410938875368,2.07234124299619,42.));
#32552=CARTESIAN_POINT('Ctrl Pts',(2.56684810362444,2.08992343448043,42.));
#32553=CARTESIAN_POINT('Ctrl Pts',(2.54939103594971,2.10731591519684,42.));
#32554=CARTESIAN_POINT('Ctrl Pts',(2.53487042035394,2.12178280800183,42.));
#32555=CARTESIAN_POINT('Ctrl Pts',(2.5202196449902,2.13611310176088,42.));
#32556=CARTESIAN_POINT('Ctrl Pts',(2.50544496557298,2.15029937598748,42.));
#32557=CARTESIAN_POINT('Ctrl Pts',(2.42926706246224,2.22344347563389,42.));
#32558=CARTESIAN_POINT('Ctrl Pts',(2.34975495167501,2.29280482501271,42.));
#32559=CARTESIAN_POINT('Ctrl Pts',(2.26705277020889,2.3580370020813,42.));
#32560=CARTESIAN_POINT('Ctrl Pts',(2.18660232836131,2.42149309688814,42.));
#32561=CARTESIAN_POINT('Ctrl Pts',(2.10313261859417,2.48104212527174,42.));
#32562=CARTESIAN_POINT('Ctrl Pts',(2.01675730739135,2.53632015288963,42.));
#32563=CARTESIAN_POINT('Ctrl Pts',(1.96924090736295,2.56672945430337,42.));
#32564=CARTESIAN_POINT('Ctrl Pts',(1.9208449031706,2.59584540845355,42.));
#32565=CARTESIAN_POINT('Ctrl Pts',(1.87158653173888,2.62360084935068,42.));
#32566=CARTESIAN_POINT('Ctrl Pts',(1.87561947885753,2.62751737394877,7.));
#32567=CARTESIAN_POINT('Ctrl Pts',(1.93354269965564,2.59525298287931,7.));
#32568=CARTESIAN_POINT('Ctrl Pts',(1.9902828570607,2.5611368520897,7.));
#32569=CARTESIAN_POINT('Ctrl Pts',(2.04574146644465,2.52519262124126,7.));
#32570=CARTESIAN_POINT('Ctrl Pts',(2.13162955029859,2.46952622160611,7.));
#32571=CARTESIAN_POINT('Ctrl Pts',(2.21444518497691,2.40947818555694,7.));
#32572=CARTESIAN_POINT('Ctrl Pts',(2.29410632613084,2.34545806303941,7.));
#32573=CARTESIAN_POINT('Ctrl Pts',(2.37532784153249,2.28018393701321,7.));
#32574=CARTESIAN_POINT('Ctrl Pts',(2.45327056143154,2.2107801777211,7.));
#32575=CARTESIAN_POINT('Ctrl Pts',(2.52782839274206,2.13762915775039,7.));
#32576=CARTESIAN_POINT('Ctrl Pts',(2.58531053735377,2.08123162801354,7.));
#32577=CARTESIAN_POINT('Ctrl Pts',(2.64078037491381,2.02260559094313,7.00000000000001));
#32578=CARTESIAN_POINT('Ctrl Pts',(2.69417895438683,1.96190848496968,7.00000000000001));
#32579=CARTESIAN_POINT('Ctrl Pts',(2.72087824412334,1.93155993198295,7.00000000000001));
#32580=CARTESIAN_POINT('Ctrl Pts',(2.74705956481114,1.90069338875978,7.));
#32581=CARTESIAN_POINT('Ctrl Pts',(2.7727145409719,1.86932730444631,7.));
#32582=CARTESIAN_POINT('Ctrl Pts',(2.78884149611167,1.84961029393483,7.));
#32583=CARTESIAN_POINT('Ctrl Pts',(2.80476051079127,1.82969580151675,7.));
#32584=CARTESIAN_POINT('Ctrl Pts',(2.82046926811514,1.80958836864072,7.));
#32585=CARTESIAN_POINT('Ctrl Pts',(2.82975021226723,1.79770862807838,7.));
#32586=CARTESIAN_POINT('Ctrl Pts',(2.83895676410696,1.78576273312009,7.));
#32587=CARTESIAN_POINT('Ctrl Pts',(2.84808162916198,1.77376089666299,7.));
#32588=CARTESIAN_POINT('Ctrl Pts',(2.91426843550152,1.68670610511091,7.));
#32589=CARTESIAN_POINT('Ctrl Pts',(2.97625815391462,1.5965866592015,7.00000000000001));
#32590=CARTESIAN_POINT('Ctrl Pts',(3.03395162804767,1.5038370359648,7.));
#32591=CARTESIAN_POINT('Ctrl Pts',(3.09256315555186,1.40961152476044,7.));
#32592=CARTESIAN_POINT('Ctrl Pts',(3.14674118550069,1.31267085407981,7.));
#32593=CARTESIAN_POINT('Ctrl Pts',(3.19635279807365,1.21342385387171,7.));
#32594=CARTESIAN_POINT('Ctrl Pts',(3.24632307395247,1.11345935517188,7.));
#32595=CARTESIAN_POINT('Ctrl Pts',(3.29166123872158,1.01115432229022,7.00000000000001));
#32596=CARTESIAN_POINT('Ctrl Pts',(3.33219378964199,0.906889812914124,7.00000000000001));
#32597=CARTESIAN_POINT('Ctrl Pts',(3.36732095539704,0.816529926352442,7.00000000000001));
#32598=CARTESIAN_POINT('Ctrl Pts',(3.39883841274255,0.724697453060791,7.));
#32599=CARTESIAN_POINT('Ctrl Pts',(3.42660553724382,0.631625023031459,7.00000000000001));
#32600=CARTESIAN_POINT('Ctrl Pts',(3.4306454355836,0.618083716097167,7.00000000000001));
#32601=CARTESIAN_POINT('Ctrl Pts',(3.43460534260238,0.604517877724185,7.00000000000001));
#32602=CARTESIAN_POINT('Ctrl Pts',(3.4384824016501,0.590937153688084,7.00000000000001));
#32603=CARTESIAN_POINT('Ctrl Pts',(3.47005153049162,0.480355493316353,7.));
#32604=CARTESIAN_POINT('Ctrl Pts',(3.49618019043182,0.36862583872353,7.00000000000001));
#32605=CARTESIAN_POINT('Ctrl Pts',(3.51673404290034,0.256178310679654,7.00000000000001));
#32606=CARTESIAN_POINT('Ctrl Pts',(3.53722278462116,0.144086995303895,7.00000000000001));
#32607=CARTESIAN_POINT('Ctrl Pts',(3.55217247491514,0.0312815018845697,
7.00000000000001));
#32608=CARTESIAN_POINT('Ctrl Pts',(3.56140843844997,-0.0818418576713709,
7.00000000000001));
#32609=CARTESIAN_POINT('Ctrl Pts',(3.56994121560687,-0.186352493155338,
7.00000000000001));
#32610=CARTESIAN_POINT('Ctrl Pts',(3.57359707077813,-0.291135254734413,
7.00000000000001));
#32611=CARTESIAN_POINT('Ctrl Pts',(3.5722009810671,-0.395890897501032,7.00000000000001));
#32612=CARTESIAN_POINT('Ctrl Pts',(3.57116150285243,-0.473888183534262,
7.00000000000001));
#32613=CARTESIAN_POINT('Ctrl Pts',(3.56732059981105,-0.551870737087469,
7.00000000000001));
#32614=CARTESIAN_POINT('Ctrl Pts',(3.56075400606168,-0.629740882624065,
7.00000000000001));
#32615=CARTESIAN_POINT('Ctrl Pts',(3.55856368150232,-0.655714910974234,
7.00000000000001));
#32616=CARTESIAN_POINT('Ctrl Pts',(3.55606999420635,-0.681676435082942,
7.00000000000001));
#32617=CARTESIAN_POINT('Ctrl Pts',(3.55327544641143,-0.707621825224809,
7.00000000000001));
#32618=CARTESIAN_POINT('Ctrl Pts',(3.55068069240703,-0.731712272018656,
7.00000000000001));
#32619=CARTESIAN_POINT('Ctrl Pts',(3.54782600396051,-0.755791644275436,
7.00000000000001));
#32620=CARTESIAN_POINT('Ctrl Pts',(3.54471830098374,-0.779822457946214,
7.00000000000001));
#32621=CARTESIAN_POINT('Ctrl Pts',(3.53000284143865,-0.893612118364699,
7.00000000000001));
#32622=CARTESIAN_POINT('Ctrl Pts',(3.50960228158218,-1.00648399764322,7.));
#32623=CARTESIAN_POINT('Ctrl Pts',(3.48384809250374,-1.11812566925976,7.));
#32624=CARTESIAN_POINT('Ctrl Pts',(3.45807685458176,-1.22984124580054,7.));
#32625=CARTESIAN_POINT('Ctrl Pts',(3.42694460602159,-1.34032567693087,7.00000000000001));
#32626=CARTESIAN_POINT('Ctrl Pts',(3.39072803041029,-1.44927444241835,7.));
#32627=CARTESIAN_POINT('Ctrl Pts',(3.35380189025642,-1.5603577603764,7.));
#32628=CARTESIAN_POINT('Ctrl Pts',(3.31159010115209,-1.6698454102589,7.));
#32629=CARTESIAN_POINT('Ctrl Pts',(3.26433136408276,-1.77741247295867,7.));
#32630=CARTESIAN_POINT('Ctrl Pts',(3.21898084301654,-1.88063618661486,7.));
#32631=CARTESIAN_POINT('Ctrl Pts',(3.16898212705041,-1.98209189032465,7.));
#32632=CARTESIAN_POINT('Ctrl Pts',(3.11450263572912,-2.08148053262523,7.));
#32633=CARTESIAN_POINT('Ctrl Pts',(3.10547063707986,-2.09795789064087,7.));
#32634=CARTESIAN_POINT('Ctrl Pts',(3.09631995779018,-2.11437003247308,7.));
#32635=CARTESIAN_POINT('Ctrl Pts',(3.08705342909664,-2.13071264965695,7.));
#32636=CARTESIAN_POINT('Ctrl Pts',(3.02764224096765,-2.23549129289445,7.));
#32637=CARTESIAN_POINT('Ctrl Pts',(2.96345098277208,-2.33745331367609,7.));
#32638=CARTESIAN_POINT('Ctrl Pts',(2.89475462679644,-2.43626425908663,7.));
#32639=CARTESIAN_POINT('Ctrl Pts',(2.825598931564,-2.53573590542643,7.));
#32640=CARTESIAN_POINT('Ctrl Pts',(2.7518773740215,-2.63201502957476,7.));
#32641=CARTESIAN_POINT('Ctrl Pts',(2.67381996723917,-2.72474601970096,7.));
#32642=CARTESIAN_POINT('Ctrl Pts',(2.6386340070233,-2.76654639539699,7.));
#32643=CARTESIAN_POINT('Ctrl Pts',(2.60256637930229,-2.80762554190717,7.));
#32644=CARTESIAN_POINT('Ctrl Pts',(2.56563509704846,-2.84794923462997,7.));
#32645=CARTESIAN_POINT('Ctrl Pts',(2.54298515597624,-2.87267973972611,7.));
#32646=CARTESIAN_POINT('Ctrl Pts',(2.52000527689653,-2.89713102952822,7.));
#32647=CARTESIAN_POINT('Ctrl Pts',(2.49672981813975,-2.92126413124198,7.));
#32648=CARTESIAN_POINT('Ctrl Pts',(2.411100096883,-3.01004909545701,7.));
#32649=CARTESIAN_POINT('Ctrl Pts',(2.32140840071681,-3.09460368152808,7.));
#32650=CARTESIAN_POINT('Ctrl Pts',(2.22790870923994,-3.17457235277157,7.));
#32651=CARTESIAN_POINT('Ctrl Pts',(2.13564011139915,-3.25348809089092,7.));
#32652=CARTESIAN_POINT('Ctrl Pts',(2.03966265549336,-3.32793863516635,7.));
#32653=CARTESIAN_POINT('Ctrl Pts',(1.94017790140973,-3.39755587824315,7.));
#32654=CARTESIAN_POINT('Ctrl Pts',(1.87771921844902,-3.44126309101144,7.));
#32655=CARTESIAN_POINT('Ctrl Pts',(1.81387727843869,-3.48306464631677,7.));
#32656=CARTESIAN_POINT('Ctrl Pts',(1.74869447533099,-3.52286199445094,7.));
#32657=CARTESIAN_POINT('Ctrl Pts',(-2.28358776666034,3.20569428094324,6.5881335146371));
#32658=CARTESIAN_POINT('Ctrl Pts',(-3.35286492248133,2.44407649255814,6.65448899198165));
#32659=CARTESIAN_POINT('Ctrl Pts',(-4.64957922564859,-0.219617924792526,
6.78715544878067));
#32660=CARTESIAN_POINT('Ctrl Pts',(-2.32229699647965,-4.03879127370882,
6.98613288503415));
#32661=CARTESIAN_POINT('Ctrl Pts',(2.14152197144423,-4.13253673306908,7.18506582339759));
#32662=CARTESIAN_POINT('Ctrl Pts',(4.6354962344389,-0.433054729749735,7.38399876176103));
#32663=CARTESIAN_POINT('Ctrl Pts',(2.86863005376323,3.66754880853003,7.58293170012447));
#32664=CARTESIAN_POINT('Ctrl Pts',(-1.53568971473972,4.39499028421212,7.7818646384879));
#32665=CARTESIAN_POINT('Ctrl Pts',(-4.52808181481838,1.08291459320159,7.98079757685135));
#32666=CARTESIAN_POINT('Ctrl Pts',(-3.35787183100746,-3.22511561142074,
8.17973051521478));
#32667=CARTESIAN_POINT('Ctrl Pts',(0.899288778474051,-4.56806013476469,
8.37866345357823));
#32668=CARTESIAN_POINT('Ctrl Pts',(4.32970627742076,-1.7116822031998,8.57759639194166));
#32669=CARTESIAN_POINT('Ctrl Pts',(3.77981709720475,2.71831339521054,8.77652933030509));
#32670=CARTESIAN_POINT('Ctrl Pts',(-0.244881287865563,4.64931963845551,
8.97546226866854));
#32671=CARTESIAN_POINT('Ctrl Pts',(-4.04445595226873,2.30620171359066,9.17439520703196));
#32672=CARTESIAN_POINT('Ctrl Pts',(-4.12594562258144,-2.15702647441609,
9.37332814539542));
#32673=CARTESIAN_POINT('Ctrl Pts',(-0.414433902178747,-4.63728597633392,
9.57226108375884));
#32674=CARTESIAN_POINT('Ctrl Pts',(3.6780683225737,-2.85446979798575,9.77119402212229));
#32675=CARTESIAN_POINT('Ctrl Pts',(4.38930591019076,1.55247461807464,9.97012696048572));
#32676=CARTESIAN_POINT('Ctrl Pts',(1.06543455816436,4.53222144777138,10.1690598988492));
#32677=CARTESIAN_POINT('Ctrl Pts',(-3.23789554621589,3.34547689252468,10.3679928372126));
#32678=CARTESIAN_POINT('Ctrl Pts',(-4.56461363563294,-0.916779903504382,
10.566925775576));
#32679=CARTESIAN_POINT('Ctrl Pts',(-1.69506170633405,-4.33623668960493,
10.7658587139395));
#32680=CARTESIAN_POINT('Ctrl Pts',(2.73276812195122,-3.76937148311671,10.9647916523029));
#32681=CARTESIAN_POINT('Ctrl Pts',(4.64835183630865,0.262694034166192,11.1637245906663));
#32682=CARTESIAN_POINT('Ctrl Pts',(2.29068463981999,4.05326372260543,11.3626575290298));
#32683=CARTESIAN_POINT('Ctrl Pts',(-2.17281932557235,4.11764970909905,11.5615904673932));
#32684=CARTESIAN_POINT('Ctrl Pts',(-4.63884063895772,0.396661654349383,
11.7605234057567));
#32685=CARTESIAN_POINT('Ctrl Pts',(-2.84035473048496,-3.68897925500734,
11.9594563441201));
#32686=CARTESIAN_POINT('Ctrl Pts',(1.56928215333904,-4.38332481861607,12.1583892824835));
#32687=CARTESIAN_POINT('Ctrl Pts',(4.53627084208731,-1.04806001180736,12.357322220847));
#32688=CARTESIAN_POINT('Ctrl Pts',(3.33304518836854,3.25069111315414,12.5562551592104));
#32689=CARTESIAN_POINT('Ctrl Pts',(-0.934264011548026,4.56106716657885,
12.7551880975738));
#32690=CARTESIAN_POINT('Ctrl Pts',(-4.34270007180307,1.67843350404123,12.9541210359373));
#32691=CARTESIAN_POINT('Ctrl Pts',(-3.75887227597289,-2.74719168498093,
13.1530539743007));
#32692=CARTESIAN_POINT('Ctrl Pts',(0.280503837458128,-4.6473111084089,13.3519869126642));
#32693=CARTESIAN_POINT('Ctrl Pts',(4.0620115019401,-2.27513636937342,13.5509198510276));
#32694=CARTESIAN_POINT('Ctrl Pts',(4.10929358463094,2.18858154439125,13.749852789391));
#32695=CARTESIAN_POINT('Ctrl Pts',(0.378883452643525,4.64032652627596,13.9487857277545));
#32696=CARTESIAN_POINT('Ctrl Pts',(-3.6998359543678,2.82619830371296,14.1477186661179));
#32697=CARTESIAN_POINT('Ctrl Pts',(-4.37727940176434,-1.5860668271018,14.3466516044813));
#32698=CARTESIAN_POINT('Ctrl Pts',(-1.03067005834432,-4.54025353608988,
14.5455845428448));
#32699=CARTESIAN_POINT('Ctrl Pts',(3.26343894045982,-3.32056459401619,14.7445174812082));
#32700=CARTESIAN_POINT('Ctrl Pts',(4.55745373218093,0.951734427334463,14.9434504195717));
#32701=CARTESIAN_POINT('Ctrl Pts',(1.66178065462684,4.34909967660568,15.1423833579351));
#32702=CARTESIAN_POINT('Ctrl Pts',(-2.7615749095149,3.74831788410233,15.3413162962985));
#32703=CARTESIAN_POINT('Ctrl Pts',(-4.64620214454805,-0.298309525729033,
15.540249234662));
#32704=CARTESIAN_POINT('Ctrl Pts',(-2.25955469263049,-4.07069963669087,
15.7391821730254));
#32705=CARTESIAN_POINT('Ctrl Pts',(2.20431162797926,-4.10087712421368,15.9381151113889));
#32706=CARTESIAN_POINT('Ctrl Pts',(4.64174427957893,-0.361099687260673,
16.1370480497523));
#32707=CARTESIAN_POINT('Ctrl Pts',(2.81200037969602,3.71063832860775,16.3359809881157));
#32708=CARTESIAN_POINT('Ctrl Pts',(-1.60282821254903,4.37116971326904,16.5349139264792));
#32709=CARTESIAN_POINT('Ctrl Pts',(-4.54416956536685,1.01326497143505,16.7338468648426));
#32710=CARTESIAN_POINT('Ctrl Pts',(-3.30803524366227,-3.27613885051165,
16.932779803206));
#32711=CARTESIAN_POINT('Ctrl Pts',(0.969190868759014,-4.55377338051179,
17.1317127415695));
#32712=CARTESIAN_POINT('Ctrl Pts',(4.35543542339085,-1.6451034052046,17.3306456799329));
#32713=CARTESIAN_POINT('Ctrl Pts',(3.73770845551644,2.77591758571908,17.5295786182963));
#32714=CARTESIAN_POINT('Ctrl Pts',(-0.316110833907594,4.64502496030214,
17.7285115566598));
#32715=CARTESIAN_POINT('Ctrl Pts',(-4.07932800118232,2.24393983874646,17.9274444950232));
#32716=CARTESIAN_POINT('Ctrl Pts',(-4.09240045043936,-2.22000934556306,
18.1263774333867));
#32717=CARTESIAN_POINT('Ctrl Pts',(-0.343310619835542,-4.64309387794946,
18.3253103717501));
#32718=CARTESIAN_POINT('Ctrl Pts',(3.72138621938403,-2.79776116695515,18.5242433101136));
#32719=CARTESIAN_POINT('Ctrl Pts',(4.36499584269893,1.61956606359996,18.723176248477));
#32720=CARTESIAN_POINT('Ctrl Pts',(0.995845006712163,4.54801887240478,18.9221091868404));
#32721=CARTESIAN_POINT('Ctrl Pts',(-3.28879065687452,3.29545732128312,19.1210421252039));
#32722=CARTESIAN_POINT('Ctrl Pts',(-4.55002616559029,-0.986633079511998,
19.3199750635673));
#32723=CARTESIAN_POINT('Ctrl Pts',(-1.62840200065756,-4.36170721912855,
19.5189080019307));
#32724=CARTESIAN_POINT('Ctrl Pts',(2.79021950300484,-3.72704414599493,19.7178409402942));
#32725=CARTESIAN_POINT('Ctrl Pts',(4.64377957295296,0.333907500617121,19.9167738786576));
#32726=CARTESIAN_POINT('Ctrl Pts',(2.22829203699626,4.08789646872357,20.115706817021));
#32727=CARTESIAN_POINT('Ctrl Pts',(-2.23567446665327,4.08386368777145,20.3146397553845));
#32728=CARTESIAN_POINT('Ctrl Pts',(-4.6443753015709,0.325516511565617,20.5135726937479));
#32729=CARTESIAN_POINT('Ctrl Pts',(-2.78348087456552,-3.73207946888481,
20.7125056321114));
#32730=CARTESIAN_POINT('Ctrl Pts',(1.63628013449202,-4.35875788070528,20.9114385704748));
#32731=CARTESIAN_POINT('Ctrl Pts',(4.55180140068407,-0.978410419953773,
21.1103715088382));
#32732=CARTESIAN_POINT('Ctrl Pts',(3.28283101156097,3.30139417378129,21.3093044472017));
#32733=CARTESIAN_POINT('Ctrl Pts',(-1.00406080348858,4.54621214243697,21.5082373855651));
#32734=CARTESIAN_POINT('Ctrl Pts',(-4.36791497172966,1.61167668621328,21.7071703239285));
#32735=CARTESIAN_POINT('Ctrl Pts',(-3.71632511212236,-2.80448045137639,
21.906103262292));
#32736=CARTESIAN_POINT('Ctrl Pts',(0.351699264548243,-4.64246600078663,
22.1050362006554));
#32737=CARTESIAN_POINT('Ctrl Pts',(4.0964049135034,-2.21261151713735,22.3039691390189));
#32738=CARTESIAN_POINT('Ctrl Pts',(4.07526696155566,2.25130676123813,22.5029020773823));
#32739=CARTESIAN_POINT('Ctrl Pts',(0.307717623722685,4.64558853162805,22.7018350157458));
#32740=CARTESIAN_POINT('Ctrl Pts',(-3.74271792010062,2.76915971220537,22.9007679541091));
#32741=CARTESIAN_POINT('Ctrl Pts',(-4.35245591888036,-1.65297017981175,
23.0997008924726));
#32742=CARTESIAN_POINT('Ctrl Pts',(-0.96096146715276,-4.55551709466568,
23.298633830836));
#32743=CARTESIAN_POINT('Ctrl Pts',(3.31394921617401,-3.27015649988854,23.4975667691995));
#32744=CARTESIAN_POINT('Ctrl Pts',(4.54233136705332,1.02147378479679,23.6964997075629));
#32745=CARTESIAN_POINT('Ctrl Pts',(1.59492770745015,4.37405859004556,23.8954326459263));
#32746=CARTESIAN_POINT('Ctrl Pts',(-2.8187002214397,3.70555151128673,24.0943655842898));
#32747=CARTESIAN_POINT('Ctrl Pts',(-4.64108426309036,-0.369485864463859,
24.2932985226532));
#32748=CARTESIAN_POINT('Ctrl Pts',(-2.19689850940736,-4.10485321059198,
24.4922314610167));
#32749=CARTESIAN_POINT('Ctrl Pts',(2.26690599978809,-4.06661039801803,24.6911643993801));
#32750=CARTESIAN_POINT('Ctrl Pts',(4.64673355030702,-0.289914217648445,
24.8900973377435));
#32751=CARTESIAN_POINT('Ctrl Pts',(2.75479789015282,3.75330141682668,25.089030276107));
#32752=CARTESIAN_POINT('Ctrl Pts',(-1.66963595449858,4.34609004975612,25.2879632144704));
#32753=CARTESIAN_POINT('Ctrl Pts',(-4.55916589979193,0.943498404512721,
25.4868961528339));
#32754=CARTESIAN_POINT('Ctrl Pts',(-3.25743397236614,-3.32645559970645,
25.6858290911973));
#32755=CARTESIAN_POINT('Ctrl Pts',(1.03887176776102,-4.5383838964209,25.8847620295608));
#32756=CARTESIAN_POINT('Ctrl Pts',(4.38013798386919,-1.57815531029427,26.0836949679242));
#32757=CARTESIAN_POINT('Ctrl Pts',(3.69472350167733,2.8328786044052,26.2826279062876));
#32758=CARTESIAN_POINT('Ctrl Pts',(-0.387267039202406,4.63963438015227,
26.4815608446511));
#32759=CARTESIAN_POINT('Ctrl Pts',(-4.11324123594255,2.18115324452121,26.6804937830145));
#32760=CARTESIAN_POINT('Ctrl Pts',(-4.05789412426333,-2.28247195325872,
26.8794267213779));
#32761=CARTESIAN_POINT('Ctrl Pts',(-0.272106554751227,-4.64781034079544,
27.0783596597414));
#32762=CARTESIAN_POINT('Ctrl Pts',(3.76382980366497,-2.74039561928326,27.2772925981048));
#32763=CARTESIAN_POINT('Ctrl Pts',(4.33966036680293,1.68627721384812,27.4762255364683));
#32764=CARTESIAN_POINT('Ctrl Pts',(0.926021488444692,4.56274776248724,27.6751584748317));
#32765=CARTESIAN_POINT('Ctrl Pts',(-3.33891314074683,3.24466361579928,27.8740914131951));
#32766=CARTESIAN_POINT('Ctrl Pts',(-4.53436978850062,-1.056254496926,28.0730243515586));
#32767=CARTESIAN_POINT('Ctrl Pts',(-1.56135974101536,-4.38615306393655,
28.271957289922));
#32768=CARTESIAN_POINT('Ctrl Pts',(2.84701539209114,-3.68384124228226,28.4708902282854));
#32769=CARTESIAN_POINT('Ctrl Pts',(4.63811637326107,0.405042527682263,28.6698231666489));
#32770=CARTESIAN_POINT('Ctrl Pts',(2.16537595366717,4.12156886639343,28.8687561050123));
#32771=CARTESIAN_POINT('Ctrl Pts',(-2.29800439309459,4.04911826827293,29.0676890433758));
#32772=CARTESIAN_POINT('Ctrl Pts',(-4.64881888728275,0.254294896501576,
29.2666219817392));
#32773=CARTESIAN_POINT('Ctrl Pts',(-2.72595311106574,-3.77430292602682,
29.4655549201026));
#32774=CARTESIAN_POINT('Ctrl Pts',(1.70289371351612,-4.33316696442807,29.6644878584661));
#32775=CARTESIAN_POINT('Ctrl Pts',(4.56626263015895,-0.908530975562921,
29.8634207968295));
#32776=CARTESIAN_POINT('Ctrl Pts',(3.23184561769564,3.35132165638052,30.0623537351929));
#32777=CARTESIAN_POINT('Ctrl Pts',(-1.07362171706024,4.53028910223179,30.2612866735564));
#32778=CARTESIAN_POINT('Ctrl Pts',(-4.39210374192795,1.54454124622366,30.4602196119198));
#32779=CARTESIAN_POINT('Ctrl Pts',(-3.67290489288628,-2.86111037692635,
30.6591525502832));
#32780=CARTESIAN_POINT('Ctrl Pts',(0.422812068905003,-4.63653026470569,
30.8580854886467));
#32781=CARTESIAN_POINT('Ctrl Pts',(4.12983597966957,-2.14956686850405,31.0570184270101));
#32782=CARTESIAN_POINT('Ctrl Pts',(4.04028295890316,2.31350309123207,31.2559513653736));
#32783=CARTESIAN_POINT('Ctrl Pts',(0.236479504429024,4.64975917496042,31.454884303737));
#32784=CARTESIAN_POINT('Ctrl Pts',(-3.78472063013482,2.71147057756036,31.6538172421005));
#32785=CARTESIAN_POINT('Ctrl Pts',(-4.32660993797449,-1.71948520952171,
31.8527501804639));
#32786=CARTESIAN_POINT('Ctrl Pts',(-0.891027122681378,-4.56971045119814,
32.0516831188273));
#32787=CARTESIAN_POINT('Ctrl Pts',(3.36368096441276,-3.21898016626241,32.2506160571907));
#32788=CARTESIAN_POINT('Ctrl Pts',(4.5261418975313,1.09097317316021,32.4495489955542));
#32789=CARTESIAN_POINT('Ctrl Pts',(1.52770007286572,4.39798993046933,32.6484819339176));
#32790=CARTESIAN_POINT('Ctrl Pts',(-2.87516335195365,3.66191461406821,32.8474148722811));
#32791=CARTESIAN_POINT('Ctrl Pts',(-4.63487607777506,-0.4405754019598,33.0463478106445));
#32792=CARTESIAN_POINT('Ctrl Pts',(-2.13372622115719,-4.13804245438466,
33.245280749008));
#32793=CARTESIAN_POINT('Ctrl Pts',(2.3289678201032,-4.03138832588321,33.4442136873714));
#32794=CARTESIAN_POINT('Ctrl Pts',(4.65063119002216,-0.218660640117578,
33.6431466257348));
#32795=CARTESIAN_POINT('Ctrl Pts',(2.69694823141472,3.79508276302539,33.8420795640982));
#32796=CARTESIAN_POINT('Ctrl Pts',(-1.73605145825132,4.31998938371931,34.0410125024617));
#32797=CARTESIAN_POINT('Ctrl Pts',(-4.57309117498029,0.873510186809756,
34.2399454408251));
#32798=CARTESIAN_POINT('Ctrl Pts',(-3.20606745040362,-3.37599088337116,
34.4388783791886));
#32799=CARTESIAN_POINT('Ctrl Pts',(1.10830861045392,-4.52192823529311,34.637811317552));
#32800=CARTESIAN_POINT('Ctrl Pts',(4.4038115431333,-1.51083646822047,34.8367442559154));
#32801=CARTESIAN_POINT('Ctrl Pts',(3.65087056719927,2.88917411083122,35.0356771942789));
#32802=CARTESIAN_POINT('Ctrl Pts',(-0.458332266027874,4.63315383676036,
35.2346101326423));
#32803=CARTESIAN_POINT('Ctrl Pts',(-4.1461881700408,2.11785424421031,35.4335430710058));
#32804=CARTESIAN_POINT('Ctrl Pts',(-4.02243449981698,-2.3443983526288,35.6324760093692));
#32805=CARTESIAN_POINT('Ctrl Pts',(-0.200838565195405,-4.65143491968315,
35.8314089477326));
#32806=CARTESIAN_POINT('Ctrl Pts',(3.80538917253758,-2.68238628582457,36.0303418860961));
#32807=CARTESIAN_POINT('Ctrl Pts',(4.313305398898,1.75259221639213,36.2292748244595));
#32808=CARTESIAN_POINT('Ctrl Pts',(0.855980425100957,4.57640475199999,36.428207762823));
#32809=CARTESIAN_POINT('Ctrl Pts',(-3.3882512324144,3.19310765946044,36.6271407011864));
#32810=CARTESIAN_POINT('Ctrl Pts',(-4.51764817756711,-1.1256277739117,36.8260736395498));
#32811=CARTESIAN_POINT('Ctrl Pts',(-1.49395067955099,-4.40956849538517,
37.0250065779133));
#32812=CARTESIAN_POINT('Ctrl Pts',(2.90314244717482,-3.63977291262905,37.2239395162767));
#32813=CARTESIAN_POINT('Ctrl Pts',(4.63136356822164,0.476082396912402,37.4228724546401));
#32814=CARTESIAN_POINT('Ctrl Pts',(2.10195116827292,4.15427301369114,37.6218053930036));
#32815=CARTESIAN_POINT('Ctrl Pts',(-2.35979445756394,4.01342159940947,37.820738331367));
#32816=CARTESIAN_POINT('Ctrl Pts',(-4.6521703611112,0.183013565819844,38.0196712697305));
#32817=CARTESIAN_POINT('Ctrl Pts',(-2.66778493740627,-3.81563975427051,
38.2186042080939));
#32818=CARTESIAN_POINT('Ctrl Pts',(1.76910720810075,-4.30655799166989,38.4175371464573));
#32819=CARTESIAN_POINT('Ctrl Pts',(4.57965119683031,-0.838438267478442,
38.6164700848208));
#32820=CARTESIAN_POINT('Ctrl Pts',(3.18010086249031,3.40046216234224,38.8154030231842));
#32821=CARTESIAN_POINT('Ctrl Pts',(-1.14293017678358,4.51330115287866,39.0143359615477));
#32822=CARTESIAN_POINT('Ctrl Pts',(-4.4152611484038,1.47704417104799,39.2132688999111));
#32823=CARTESIAN_POINT('Ctrl Pts',(-3.6286209586944,-2.91707048796121,39.4122018382745));
#32824=CARTESIAN_POINT('Ctrl Pts',(0.493823895339948,-4.62950082687821,
39.6111347766379));
#32825=CARTESIAN_POINT('Ctrl Pts',(4.16230000860224,-2.08602580072547,39.8100677150015));
#32826=CARTESIAN_POINT('Ctrl Pts',(4.00434373250677,2.37517234857208,40.0090006533648));
#32827=CARTESIAN_POINT('Ctrl Pts',(0.16519745519922,4.6528059816321,40.2079335917283));
#32828=CARTESIAN_POINT('Ctrl Pts',(-3.82585650677666,2.65320484133016,40.4068665300917));
#32829=CARTESIAN_POINT('Ctrl Pts',(-4.29970479193952,-1.78571208206424,
40.6057994684551));
#32830=CARTESIAN_POINT('Ctrl Pts',(-0.820965403692237,-4.58260824249866,
40.8047324068186));
#32831=CARTESIAN_POINT('Ctrl Pts',(3.41277964200003,-3.16747340374845,41.003665345182));
#32832=CARTESIAN_POINT('Ctrl Pts',(4.50858774680517,1.16103327592888,41.2025982835454));
#32833=CARTESIAN_POINT('Ctrl Pts',(1.46069211445911,4.41931609540443,41.4015312219089));
#32834=CARTESIAN_POINT('Ctrl Pts',(-2.93206675809147,3.62048102032587,41.6004641602723));
#32835=CARTESIAN_POINT('Ctrl Pts',(-4.62538118106894,-0.517884424352666,
41.7993970986358));
#32836=CARTESIAN_POINT('Ctrl Pts',(-2.92506802252003,-2.94215747695014,
41.9320190575447));
#32837=CARTESIAN_POINT('Ctrl Pts',(-1.74998052418886,-3.52545282590189,
41.9983300369992));
#32838=CARTESIAN_POINT('Ctrl Pts',(-2.14454317821952,3.01050386677641,6.72649619915742));
#32839=CARTESIAN_POINT('Ctrl Pts',(-3.14871348584711,2.29525996140177,6.79285167650196));
#32840=CARTESIAN_POINT('Ctrl Pts',(-4.36647259874689,-0.206245684665433,
6.92551813330099));
#32841=CARTESIAN_POINT('Ctrl Pts',(-2.18089545508631,-3.7928747038927,7.12449556955447));
#32842=CARTESIAN_POINT('Ctrl Pts',(2.01112757824255,-3.88091212828921,7.32342850791792));
#32843=CARTESIAN_POINT('Ctrl Pts',(4.35324710193498,-0.406686609570857,
7.52236144628135));
#32844=CARTESIAN_POINT('Ctrl Pts',(2.69396302714936,3.44423669322017,7.7212943846448));
#32845=CARTESIAN_POINT('Ctrl Pts',(-1.44218363300452,4.12738523561646,7.92022732300823));
#32846=CARTESIAN_POINT('Ctrl Pts',(-4.25237300188823,1.01697737978396,8.11916026137167));
#32847=CARTESIAN_POINT('Ctrl Pts',(-3.15341553044576,-3.02874265855638,
8.31809319973511));
#32848=CARTESIAN_POINT('Ctrl Pts',(0.844532293999059,-4.28991709569067,
8.51702613809854));
#32849=CARTESIAN_POINT('Ctrl Pts',(4.06607628421319,-1.60746017549409,8.71595907646199));
#32850=CARTESIAN_POINT('Ctrl Pts',(3.54966911676128,2.55279894780965,8.91489201482541));
#32851=CARTESIAN_POINT('Ctrl Pts',(-0.229970795531832,4.36622881746894,
9.11382495318887));
#32852=CARTESIAN_POINT('Ctrl Pts',(-3.79819446779221,2.16578019232958,9.31275789155229));
#32853=CARTESIAN_POINT('Ctrl Pts',(-3.87472234165631,-2.02568803287688,
9.51169082991574));
#32854=CARTESIAN_POINT('Ctrl Pts',(-0.389199579151803,-4.35492786885263,
9.71062376827917));
#32855=CARTESIAN_POINT('Ctrl Pts',(3.45411568819898,-2.6806649703053,9.90955670664261));
#32856=CARTESIAN_POINT('Ctrl Pts',(4.12204697548566,1.45794652614552,10.1084896450061));
#32857=CARTESIAN_POINT('Ctrl Pts',(1.00056168057528,4.25626057815718,10.3074225833695));
#32858=CARTESIAN_POINT('Ctrl Pts',(-3.04074444030663,3.14177530310008,10.5063555217329));
#32859=CARTESIAN_POINT('Ctrl Pts',(-4.28668044925664,-0.860958407946073,
10.7052884600964));
#32860=CARTESIAN_POINT('Ctrl Pts',(-1.59185167833342,-4.07220906838072,
10.9042213984598));
#32861=CARTESIAN_POINT('Ctrl Pts',(2.56637354567592,-3.53985952206916,11.1031543368232));
#32862=CARTESIAN_POINT('Ctrl Pts',(4.36531994349343,0.246698947662476,11.3020872751867));
#32863=CARTESIAN_POINT('Ctrl Pts',(2.15120793231547,3.80646594483665,11.5010202135501));
#32864=CARTESIAN_POINT('Ctrl Pts',(-2.04051927856241,3.86693155519059,11.6999531519136));
#32865=CARTESIAN_POINT('Ctrl Pts',(-4.35638787015977,0.372509459594964,
11.898886090277));
#32866=CARTESIAN_POINT('Ctrl Pts',(-2.66740935028452,-3.46436226862834,
12.0978190286404));
#32867=CARTESIAN_POINT('Ctrl Pts',(1.47373067318826,-4.11643006453438,12.2967519670039));
#32868=CARTESIAN_POINT('Ctrl Pts',(4.2600634102983,-0.984245046982922,12.4956849053673));
#32869=CARTESIAN_POINT('Ctrl Pts',(3.13010054869347,3.05276090237982,12.6946178437308));
#32870=CARTESIAN_POINT('Ctrl Pts',(-0.877377932161288,4.28334991993443,
12.8935507820942));
#32871=CARTESIAN_POINT('Ctrl Pts',(-4.07827890392793,1.57623594491877,13.0924837204576));
#32872=CARTESIAN_POINT('Ctrl Pts',(-3.52999959753036,-2.57991887734767,
13.2914166588211));
#32873=CARTESIAN_POINT('Ctrl Pts',(0.263424335980266,-4.36434258411605,
13.4903495971845));
#32874=CARTESIAN_POINT('Ctrl Pts',(3.8146810836505,-2.1366063751491,13.6892825355479));
#32875=CARTESIAN_POINT('Ctrl Pts',(3.85908422390511,2.05532175707241,13.8882154739114));
#32876=CARTESIAN_POINT('Ctrl Pts',(0.355813748685168,4.35778328379722,14.0871484122748));
#32877=CARTESIAN_POINT('Ctrl Pts',(-3.47455791816341,2.65411488930297,14.2860813506383));
#32878=CARTESIAN_POINT('Ctrl Pts',(-4.11075274498564,-1.48949335073545,
14.4850142890017));
#32879=CARTESIAN_POINT('Ctrl Pts',(-0.967913944402505,-4.26380360341846,
14.6839472273652));
#32880=CARTESIAN_POINT('Ctrl Pts',(3.06473253162247,-3.11837988094897,14.8828801657286));
#32881=CARTESIAN_POINT('Ctrl Pts',(4.27995650269812,0.893784597822432,15.081813104092));
#32882=CARTESIAN_POINT('Ctrl Pts',(1.56059706511263,4.08428884539946,15.2807460424554));
#32883=CARTESIAN_POINT('Ctrl Pts',(-2.59342632668046,3.52008784838862,15.4796789808189));
#32884=CARTESIAN_POINT('Ctrl Pts',(-4.3633011435735,-0.280145859835127,
15.6786119191823));
#32885=CARTESIAN_POINT('Ctrl Pts',(-2.12197344575085,-3.82284020955897,
15.8775448575457));
#32886=CARTESIAN_POINT('Ctrl Pts',(2.0700940570225,-3.8511802304453,16.0764777959092));
#32887=CARTESIAN_POINT('Ctrl Pts',(4.35911471200799,-0.339112812863191,
16.2754107342726));
#32888=CARTESIAN_POINT('Ctrl Pts',(2.6407814577879,3.48470255036153,16.4743436726361));
#32889=CARTESIAN_POINT('Ctrl Pts',(-1.50523415796133,4.10501506720731,16.6732766109995));
#32890=CARTESIAN_POINT('Ctrl Pts',(-4.26748119093852,0.951568629831059,
16.8722095493629));
#32891=CARTESIAN_POINT('Ctrl Pts',(-3.10661342589027,-3.07665916122845,
17.0711424877264));
#32892=CARTESIAN_POINT('Ctrl Pts',(0.910178140001792,-4.27650024269325,
17.2700754260898));
#32893=CARTESIAN_POINT('Ctrl Pts',(4.09023881708235,-1.54493527098234,17.4690083644533));
#32894=CARTESIAN_POINT('Ctrl Pts',(3.51012441364316,2.60689569661673,17.6679413028167));
#32895=CARTESIAN_POINT('Ctrl Pts',(-0.296863270295577,4.36219563649339,
17.8668742411801));
#32896=CARTESIAN_POINT('Ctrl Pts',(-3.83094320453884,2.10730935932299,18.0658071795436));
#32897=CARTESIAN_POINT('Ctrl Pts',(-3.84321968993877,-2.08483596169087,
18.264740117907));
#32898=CARTESIAN_POINT('Ctrl Pts',(-0.322406897833154,-4.3603821351485,
18.4636730562704));
#32899=CARTESIAN_POINT('Ctrl Pts',(3.4947960165208,-2.62740925156378,18.6626059946339));
#32900=CARTESIAN_POINT('Ctrl Pts',(4.09921711531441,1.52095286376864,18.8615389329973));
#32901=CARTESIAN_POINT('Ctrl Pts',(0.935209343336036,4.27109611884696,19.0604718713608));
#32902=CARTESIAN_POINT('Ctrl Pts',(-3.08854061611436,3.09480135629163,19.2594048097242));
#32903=CARTESIAN_POINT('Ctrl Pts',(-4.27298119064957,-0.926558317996034,
19.4583377480876));
#32904=CARTESIAN_POINT('Ctrl Pts',(-1.52925079250028,-4.09612873161108,
19.6572706864511));
#32905=CARTESIAN_POINT('Ctrl Pts',(2.62032678939031,-3.50010943958843,19.8562036248145));
#32906=CARTESIAN_POINT('Ctrl Pts',(4.36102607910528,0.313576321899792,20.055136563178));
#32907=CARTESIAN_POINT('Ctrl Pts',(2.09261433118024,3.83898994961327,20.2540695015414));
#32908=CARTESIAN_POINT('Ctrl Pts',(-2.09954725462231,3.83520271927058,20.4530024399048));
#32909=CARTESIAN_POINT('Ctrl Pts',(-4.36158553460872,0.30569624888859,20.6519353782683));
#32910=CARTESIAN_POINT('Ctrl Pts',(-2.61399846697548,-3.50483816843836,
20.8508683166317));
#32911=CARTESIAN_POINT('Ctrl Pts',(1.53664923735901,-4.09335897443855,21.0498012549951));
#32912=CARTESIAN_POINT('Ctrl Pts',(4.27464833406557,-0.918836325121606,
21.2487341933586));
#32913=CARTESIAN_POINT('Ctrl Pts',(3.08294384559025,3.10037672182424,21.447667131722));
#32914=CARTESIAN_POINT('Ctrl Pts',(-0.942924891294206,4.26939939823746,
21.6466000700854));
#32915=CARTESIAN_POINT('Ctrl Pts',(-4.10195850250371,1.51354385996249,21.8455330084489));
#32916=CARTESIAN_POINT('Ctrl Pts',(-3.49004307327481,-2.63371940779178,
22.0444659468123));
#32917=CARTESIAN_POINT('Ctrl Pts',(0.330284769249194,-4.35979248858183,
22.2433988851758));
#32918=CARTESIAN_POINT('Ctrl Pts',(3.84698032663149,-2.07788857709042,22.4423318235392));
#32919=CARTESIAN_POINT('Ctrl Pts',(3.82712943615432,2.11422771981017,22.6412647619026));
#32920=CARTESIAN_POINT('Ctrl Pts',(0.288981111392786,4.36272489271909,22.8401977002661));
#32921=CARTESIAN_POINT('Ctrl Pts',(-3.51482885866484,2.6005493009342,23.0391306386295));
#32922=CARTESIAN_POINT('Ctrl Pts',(-4.08744073059509,-1.5523230482618,23.238063576993));
#32923=CARTESIAN_POINT('Ctrl Pts',(-0.902449815593572,-4.27813778443702,
23.4369965153564));
#32924=CARTESIAN_POINT('Ctrl Pts',(3.11216730456806,-3.07104106789052,23.6359294537198));
#32925=CARTESIAN_POINT('Ctrl Pts',(4.26575491804855,0.959277619585273,23.8348623920833));
#32926=CARTESIAN_POINT('Ctrl Pts',(1.4978147039944,4.10772804416148,24.0337953304467));
#32927=CARTESIAN_POINT('Ctrl Pts',(-2.64707335517684,3.47992546250712,24.2327282688101));
#32928=CARTESIAN_POINT('Ctrl Pts',(-4.35849488303591,-0.346988367013049,
24.4316612071736));
#32929=CARTESIAN_POINT('Ctrl Pts',(-2.06313231327231,-3.85491421827051,
24.630594145537));
#32930=CARTESIAN_POINT('Ctrl Pts',(2.12887714170064,-3.81899995913029,24.8295270839005));
#32931=CARTESIAN_POINT('Ctrl Pts',(4.36380019275037,-0.272261730774709,
25.0284600222639));
#32932=CARTESIAN_POINT('Ctrl Pts',(2.58706195091454,3.52476794050656,25.2273929606274));
#32933=CARTESIAN_POINT('Ctrl Pts',(-1.56797406633792,4.08146247068183,25.4263258989908));
#32934=CARTESIAN_POINT('Ctrl Pts',(-4.28156441872558,0.886050055355632,
25.6252588373542));
#32935=CARTESIAN_POINT('Ctrl Pts',(-3.05909319796137,-3.12391219122417,
25.8241917757177));
#32936=CARTESIAN_POINT('Ctrl Pts',(0.975616262761357,-4.2620478035949,26.0231247140811));
#32937=CARTESIAN_POINT('Ctrl Pts',(4.11343727186996,-1.48206355554802,26.2220576524445));
#32938=CARTESIAN_POINT('Ctrl Pts',(3.46975675584276,2.6603884354688,26.4209905908079));
#32939=CARTESIAN_POINT('Ctrl Pts',(-0.363686869931574,4.35713328152031,
26.6199235291714));
#32940=CARTESIAN_POINT('Ctrl Pts',(-3.86279150803662,2.0483457563929,26.8188564675348));
#32941=CARTESIAN_POINT('Ctrl Pts',(-3.810814407564,-2.14349530519553,27.0177894058983));
#32942=CARTESIAN_POINT('Ctrl Pts',(-0.255538352525876,-4.36481141891387,
27.2167223442617));
#32943=CARTESIAN_POINT('Ctrl Pts',(3.53465526802747,-2.57353661495193,27.4156552826252));
#32944=CARTESIAN_POINT('Ctrl Pts',(4.07542428247787,1.58360206178266,27.6145882209886));
#32945=CARTESIAN_POINT('Ctrl Pts',(0.869637285206309,4.28492818661779,27.813521159352));
#32946=CARTESIAN_POINT('Ctrl Pts',(-3.13561120934189,3.04710041123396,28.0124540977155));
#32947=CARTESIAN_POINT('Ctrl Pts',(-4.25827810930823,-0.99194058092151,
28.2113870360789));
#32948=CARTESIAN_POINT('Ctrl Pts',(-1.46629064589802,-4.11908610180032,
28.4103199744424));
#32949=CARTESIAN_POINT('Ctrl Pts',(2.67366445316185,-3.4595371025892,28.6092529128058));
#32950=CARTESIAN_POINT('Ctrl Pts',(4.35570770402749,0.380380032820054,28.8081858511692));
#32951=CARTESIAN_POINT('Ctrl Pts',(2.03352912356371,3.87061208026725,29.0071187895327));
#32952=CARTESIAN_POINT('Ctrl Pts',(-2.15808199565578,3.80257290164423,29.2060517278961));
#32953=CARTESIAN_POINT('Ctrl Pts',(-4.36575855636173,0.238811222196252,
29.4049846662595));
#32954=CARTESIAN_POINT('Ctrl Pts',(-2.55997349163937,-3.5444906960516,29.603917604623));
#32955=CARTESIAN_POINT('Ctrl Pts',(1.59920680512957,-4.06932625464213,29.8028505429864));
#32956=CARTESIAN_POINT('Ctrl Pts',(4.2882290387233,-0.853211746134946,30.0017834813498));
#32957=CARTESIAN_POINT('Ctrl Pts',(3.03506288379887,3.14726418714398,30.2007164197133));
#32958=CARTESIAN_POINT('Ctrl Pts',(-1.00825033437494,4.25444589053914,30.3996493580767));
#32959=CARTESIAN_POINT('Ctrl Pts',(-4.12467445101052,1.45049620663885,30.5985822964402));
#32960=CARTESIAN_POINT('Ctrl Pts',(-3.44926665280217,-2.68690121332354,
30.7975152348036));
#32961=CARTESIAN_POINT('Ctrl Pts',(0.397067610571902,-4.35421817148927,
30.996448173167));
#32962=CARTESIAN_POINT('Ctrl Pts',(3.87837582013254,-2.01868263233817,31.1953811115305));
#32963=CARTESIAN_POINT('Ctrl Pts',(3.7942755623814,2.17263699890429,31.3943140498939));
#32964=CARTESIAN_POINT('Ctrl Pts',(0.222080585391179,4.36664159118708,31.5932469882574));
#32965=CARTESIAN_POINT('Ctrl Pts',(-3.55427408016482,2.54637278012491,31.7921799266208));
#32966=CARTESIAN_POINT('Ctrl Pts',(-4.06316847671228,-1.61478806725346,
31.9911128649843));
#32967=CARTESIAN_POINT('Ctrl Pts',(-0.836773679318462,-4.2914669265756,
32.1900458033476));
#32968=CARTESIAN_POINT('Ctrl Pts',(3.15887095352933,-3.02298079240363,32.3889787417111));
#32969=CARTESIAN_POINT('Ctrl Pts',(4.25055120355625,1.02454528364496,32.5879116800745));
#32970=CARTESIAN_POINT('Ctrl Pts',(1.43468046968086,4.1302022374466,32.786844618438));
#32971=CARTESIAN_POINT('Ctrl Pts',(-2.70009852159804,3.43894555728302,32.9857775568014));
#32972=CARTESIAN_POINT('Ctrl Pts',(-4.3526647057765,-0.413749358162806,
33.1847104951649));
#32973=CARTESIAN_POINT('Ctrl Pts',(-2.00380650070783,-3.88608261363723,
33.3836434335282));
#32974=CARTESIAN_POINT('Ctrl Pts',(2.18716010122942,-3.7859225116057,33.5825763718918));
#32975=CARTESIAN_POINT('Ctrl Pts',(4.36746051042428,-0.205346687767176,
33.7815093102551));
#32976=CARTESIAN_POINT('Ctrl Pts',(2.53273468010832,3.56400527671735,33.9804422486186));
#32977=CARTESIAN_POINT('Ctrl Pts',(-1.63034561937406,4.05695103910325,34.179375186982));
#32978=CARTESIAN_POINT('Ctrl Pts',(-4.29464180263262,0.820323326117568,
34.3783081253455));
#32979=CARTESIAN_POINT('Ctrl Pts',(-3.01085431445013,-3.17043133807512,
34.5772410637089));
#32980=CARTESIAN_POINT('Ctrl Pts',(1.04082518947229,-4.24659410554575,34.7761740020724));
#32981=CARTESIAN_POINT('Ctrl Pts',(4.1356693799436,-1.41884366724649,34.9751069404358));
#32982=CARTESIAN_POINT('Ctrl Pts',(3.42857396757734,2.7132561842074,35.1740398787992));
#32983=CARTESIAN_POINT('Ctrl Pts',(-0.43042503065489,4.35104732970134,35.3729728171627));
#32984=CARTESIAN_POINT('Ctrl Pts',(-3.89373234762037,1.98890094709468,35.5719057555261));
#32985=CARTESIAN_POINT('Ctrl Pts',(-3.77751387196871,-2.2016510893785,35.7708386938896));
#32986=CARTESIAN_POINT('Ctrl Pts',(-0.188609775022207,-4.36821530206696,
35.969771632253));
#32987=CARTESIAN_POINT('Ctrl Pts',(3.57368414281305,-2.51905939180415,36.1687045706164));
#32988=CARTESIAN_POINT('Ctrl Pts',(4.05067403312995,1.64587923299354,36.3676375089799));
#32989=CARTESIAN_POINT('Ctrl Pts',(0.803860928027483,4.29775362040325,36.5665704473433));
#32990=CARTESIAN_POINT('Ctrl Pts',(-3.18194517095124,2.99868362775086,36.7655033857068));
#32991=CARTESIAN_POINT('Ctrl Pts',(-4.24257465477942,-1.05708981235569,
36.9644363240701));
#32992=CARTESIAN_POINT('Ctrl Pts',(-1.40298603154328,-4.14107579911404,
37.1633692624336));
#32993=CARTESIAN_POINT('Ctrl Pts',(2.72637400733384,-3.41815203427124,37.362302200797));
#32994=CARTESIAN_POINT('Ctrl Pts',(4.34936606820663,0.447094379937924,37.5612351391605));
#32995=CARTESIAN_POINT('Ctrl Pts',(1.97396618806673,3.90132491601227,37.7601680775239));
#32996=CARTESIAN_POINT('Ctrl Pts',(-2.21610974618682,3.76904975494763,37.9591010158874));
#32997=CARTESIAN_POINT('Ctrl Pts',(-4.3689059634554,0.17187011588989,38.1580339542508));
#32998=CARTESIAN_POINT('Ctrl Pts',(-2.50534709985704,-3.5833105804079,38.3569668926142));
#32999=CARTESIAN_POINT('Ctrl Pts',(1.66138864906423,-4.04433746645492,38.5558998309777));
#33000=CARTESIAN_POINT('Ctrl Pts',(4.30080239357324,-0.787386888794196,
38.7548327693411));
#33001=CARTESIAN_POINT('Ctrl Pts',(2.98646879715839,3.19341259377544,38.9537657077046));
#33002=CARTESIAN_POINT('Ctrl Pts',(-1.07333869518271,4.23849231457894,39.152698646068));
#33003=CARTESIAN_POINT('Ctrl Pts',(-4.14642183414512,1.38710893760937,39.3516315844314));
#33004=CARTESIAN_POINT('Ctrl Pts',(-3.40767910781596,-2.73945398844537,
39.5505645227949));
#33005=CARTESIAN_POINT('Ctrl Pts',(0.46375562238267,-4.34761674667882,39.7494974611583));
#33006=CARTESIAN_POINT('Ctrl Pts',(3.90886315799689,-1.9590104947349,39.9484303995218));
#33007=CARTESIAN_POINT('Ctrl Pts',(3.76052462715392,2.23055129808965,40.1473633378851));
#33008=CARTESIAN_POINT('Ctrl Pts',(0.155138804288171,4.36950288189749,40.3462962762487));
#33009=CARTESIAN_POINT('Ctrl Pts',(-3.59290524859212,2.49165476622559,40.545229214612));
#33010=CARTESIAN_POINT('Ctrl Pts',(-4.03790154884084,-1.67698247458014,
40.7441621529755));
#33011=CARTESIAN_POINT('Ctrl Pts',(-0.770977924188701,-4.3035793887071,
40.943095091339));
#33012=CARTESIAN_POINT('Ctrl Pts',(3.20498007865981,-2.97461020739956,41.1420280297023));
#33013=CARTESIAN_POINT('Ctrl Pts',(4.23406590146329,1.09033952096375,41.3409609680659));
#33014=CARTESIAN_POINT('Ctrl Pts',(1.37175253575807,4.15022988087543,41.5398939064291));
#33015=CARTESIAN_POINT('Ctrl Pts',(-2.75353715585242,3.40003479934917,41.7388268447928));
#33016=CARTESIAN_POINT('Ctrl Pts',(-4.34374794056332,-0.486351138137266,
41.9377597831561));
#33017=CARTESIAN_POINT('Ctrl Pts',(-2.74696456387898,-2.76301346440847,
42.0703817420651));
#33018=CARTESIAN_POINT('Ctrl Pts',(-1.64342656321671,-3.3107927439021,42.1366927215196));
#33019=CARTESIAN_POINT('Ctrl Pts',(-2.0054985897787,2.81531345260957,6.86485888367774));
#33020=CARTESIAN_POINT('Ctrl Pts',(-2.94456204921288,2.14644343024538,6.93121436102229));
#33021=CARTESIAN_POINT('Ctrl Pts',(-4.08336597184518,-0.19287344453834,
7.06388081782131));
#33022=CARTESIAN_POINT('Ctrl Pts',(-2.03949391369296,-3.54695813407657,
7.26285825407481));
#33023=CARTESIAN_POINT('Ctrl Pts',(1.88073318504086,-3.62928752350934,7.46179119243823));
#33024=CARTESIAN_POINT('Ctrl Pts',(4.07099796943106,-0.380318489391973,
7.66072413080168));
#33025=CARTESIAN_POINT('Ctrl Pts',(2.51929600053549,3.2209245779103,7.8596570691651));
#33026=CARTESIAN_POINT('Ctrl Pts',(-1.34867755126933,3.85978018702081,8.05859000752856));
#33027=CARTESIAN_POINT('Ctrl Pts',(-3.97666418895809,0.951040166366322,
8.25752294589198));
#33028=CARTESIAN_POINT('Ctrl Pts',(-2.94895922988404,-2.83236970569201,
8.45645588425543));
#33029=CARTESIAN_POINT('Ctrl Pts',(0.789775809524059,-4.01177405661665,
8.65538882261886));
#33030=CARTESIAN_POINT('Ctrl Pts',(3.80244629100563,-1.50323814778838,8.85432176098231));
#33031=CARTESIAN_POINT('Ctrl Pts',(3.31952113631781,2.38728450040875,9.05325469934573));
#33032=CARTESIAN_POINT('Ctrl Pts',(-0.2150603031981,4.08313799648236,9.25218763770918));
#33033=CARTESIAN_POINT('Ctrl Pts',(-3.5519329833157,2.02535867106851,9.45112057607261));
#33034=CARTESIAN_POINT('Ctrl Pts',(-3.62349906073116,-1.89434959133768,
9.65005351443604));
#33035=CARTESIAN_POINT('Ctrl Pts',(-0.363965256124856,-4.07256976137133,
9.84898645279951));
#33036=CARTESIAN_POINT('Ctrl Pts',(3.23016305382427,-2.50686014262486,10.0479193911629));
#33037=CARTESIAN_POINT('Ctrl Pts',(3.85478804078057,1.36341843421643,10.2468523295264));
#33038=CARTESIAN_POINT('Ctrl Pts',(0.93568880298618,3.98029970854296,10.4457852678898));
#33039=CARTESIAN_POINT('Ctrl Pts',(-2.84359333439737,2.9380737136755,10.6447182062533));
#33040=CARTESIAN_POINT('Ctrl Pts',(-4.00874726288035,-0.805136912387771,
10.8436511446167));
#33041=CARTESIAN_POINT('Ctrl Pts',(-1.48864165033278,-3.8081814471565,11.0425840829802));
#33042=CARTESIAN_POINT('Ctrl Pts',(2.39997896940062,-3.31034756102161,11.2415170213436));
#33043=CARTESIAN_POINT('Ctrl Pts',(4.0822880506782,0.23070386115876,11.440449959707));
#33044=CARTESIAN_POINT('Ctrl Pts',(2.01173122481096,3.55966816706786,11.6393828980705));
#33045=CARTESIAN_POINT('Ctrl Pts',(-1.90821923155247,3.61621340128212,11.8383158364339));
#33046=CARTESIAN_POINT('Ctrl Pts',(-4.07393510136182,0.34835726484055,12.0372487747973));
#33047=CARTESIAN_POINT('Ctrl Pts',(-2.49446397008411,-3.23974528224934,
12.2361817131608));
#33048=CARTESIAN_POINT('Ctrl Pts',(1.3781791930375,-3.84953531045267,12.4351146515242));
#33049=CARTESIAN_POINT('Ctrl Pts',(3.98385597850928,-0.920430082158486,
12.6340475898877));
#33050=CARTESIAN_POINT('Ctrl Pts',(2.92715590901843,2.8548306916055,12.8329805282511));
#33051=CARTESIAN_POINT('Ctrl Pts',(-0.820491852774556,4.00563267329001,
13.0319134666145));
#33052=CARTESIAN_POINT('Ctrl Pts',(-3.81385773605278,1.47403838579632,13.230846404978));
#33053=CARTESIAN_POINT('Ctrl Pts',(-3.30112691908783,-2.41264606971442,
13.4297793433414));
#33054=CARTESIAN_POINT('Ctrl Pts',(0.246344834502405,-4.0813740598232,13.6287122817048));
#33055=CARTESIAN_POINT('Ctrl Pts',(3.56735066536092,-1.99807638092479,13.8276452200683));
#33056=CARTESIAN_POINT('Ctrl Pts',(3.60887486317929,1.92206196975356,14.0265781584317));
#33057=CARTESIAN_POINT('Ctrl Pts',(0.332744044726809,4.07524004131849,14.2255110967952));
#33058=CARTESIAN_POINT('Ctrl Pts',(-3.24927988195903,2.48203147489298,14.4244440351586));
#33059=CARTESIAN_POINT('Ctrl Pts',(-3.84422608820695,-1.39291987436911,
14.623376973522));
#33060=CARTESIAN_POINT('Ctrl Pts',(-0.905157830460687,-3.98735367074704,
14.8223099118855));
#33061=CARTESIAN_POINT('Ctrl Pts',(2.86602612278512,-2.91619516788176,15.0212428502489));
#33062=CARTESIAN_POINT('Ctrl Pts',(4.00245927321531,0.835834768310396,15.2201757886123));
#33063=CARTESIAN_POINT('Ctrl Pts',(1.45941347559844,3.81947801419324,15.4191087269758));
#33064=CARTESIAN_POINT('Ctrl Pts',(-2.42527774384603,3.29185781267492,15.6180416653392));
#33065=CARTESIAN_POINT('Ctrl Pts',(-4.08040014259896,-0.261982193941216,
15.8169746037027));
#33066=CARTESIAN_POINT('Ctrl Pts',(-1.98439219887121,-3.57498078242707,
16.0159075420661));
#33067=CARTESIAN_POINT('Ctrl Pts',(1.93587648606574,-3.60148333667693,16.2148404804295));
#33068=CARTESIAN_POINT('Ctrl Pts',(4.07648514443705,-0.317125938465704,
16.413773418793));
#33069=CARTESIAN_POINT('Ctrl Pts',(2.46956253587978,3.25876677211529,16.6127063571564));
#33070=CARTESIAN_POINT('Ctrl Pts',(-1.40764010337363,3.8388604211456,16.8116392955199));
#33071=CARTESIAN_POINT('Ctrl Pts',(-3.99079281651019,0.889872288227052,
17.0105722338833));
#33072=CARTESIAN_POINT('Ctrl Pts',(-2.90519160811827,-2.87717947194522,
17.2095051722467));
#33073=CARTESIAN_POINT('Ctrl Pts',(0.851165411244564,-3.99922710487472,
17.4084381106102));
#33074=CARTESIAN_POINT('Ctrl Pts',(3.82504221077387,-1.44476713676006,17.6073710489736));
#33075=CARTESIAN_POINT('Ctrl Pts',(3.28254037176988,2.43787380751438,17.806303987337));
#33076=CARTESIAN_POINT('Ctrl Pts',(-0.277615706683554,4.07936631268466,
18.0052369257005));
#33077=CARTESIAN_POINT('Ctrl Pts',(-3.58255840789535,1.97067887989953,18.2041698640639));
#33078=CARTESIAN_POINT('Ctrl Pts',(-3.59403892943819,-1.94966257781868,
18.4031028024274));
#33079=CARTESIAN_POINT('Ctrl Pts',(-0.301503175830768,-4.07767039234755,
18.6020357407908));
#33080=CARTESIAN_POINT('Ctrl Pts',(3.26820581365757,-2.45705733617242,18.8009686791542));
#33081=CARTESIAN_POINT('Ctrl Pts',(3.83343838792988,1.42233966393734,18.9999016175177));
#33082=CARTESIAN_POINT('Ctrl Pts',(0.874573679959915,3.99417336528914,19.1988345558811));
#33083=CARTESIAN_POINT('Ctrl Pts',(-2.88829057535421,2.89414539130014,19.3977674942445));
#33084=CARTESIAN_POINT('Ctrl Pts',(-3.99593621570884,-0.866483556480068,
19.596700432608));
#33085=CARTESIAN_POINT('Ctrl Pts',(-1.43009958434302,-3.83055024409362,
19.7956333709714));
#33086=CARTESIAN_POINT('Ctrl Pts',(2.45043407577578,-3.27317473318194,19.9945663093349));
#33087=CARTESIAN_POINT('Ctrl Pts',(4.07827258525759,0.293245143182466,20.1934992476983));
#33088=CARTESIAN_POINT('Ctrl Pts',(1.95693662536422,3.59008343050296,20.3924321860618));
#33089=CARTESIAN_POINT('Ctrl Pts',(-1.96342004259136,3.58654175076973,20.5913651244252));
#33090=CARTESIAN_POINT('Ctrl Pts',(-4.07879576764655,0.285875986211559,
20.7902980627886));
#33091=CARTESIAN_POINT('Ctrl Pts',(-2.44451605938545,-3.27759686799192,
20.989231001152));
#33092=CARTESIAN_POINT('Ctrl Pts',(1.43701834022598,-3.82796006817182,21.1881639395155));
#33093=CARTESIAN_POINT('Ctrl Pts',(3.99749526744709,-0.85926223028944,21.3870968778789));
#33094=CARTESIAN_POINT('Ctrl Pts',(2.88305667961953,2.89935926986721,21.5860298162423));
#33095=CARTESIAN_POINT('Ctrl Pts',(-0.881788979099839,3.99258665403793,
21.7849627546059));
#33096=CARTESIAN_POINT('Ctrl Pts',(-3.83600203327774,1.41541103371171,21.9838956929692));
#33097=CARTESIAN_POINT('Ctrl Pts',(-3.26376103442727,-2.46295836420717,
22.1828286313327));
#33098=CARTESIAN_POINT('Ctrl Pts',(0.30887027395015,-4.07711897637704,22.3817615696961));
#33099=CARTESIAN_POINT('Ctrl Pts',(3.59755573975958,-1.94316563704349,22.5806945080596));
#33100=CARTESIAN_POINT('Ctrl Pts',(3.57899191075299,1.97714867838221,22.779627446423));
#33101=CARTESIAN_POINT('Ctrl Pts',(0.270244599062885,4.07986125381013,22.9785603847864));
#33102=CARTESIAN_POINT('Ctrl Pts',(-3.28693979722906,2.43193888966304,23.1774933231499));
#33103=CARTESIAN_POINT('Ctrl Pts',(-3.82242554230984,-1.45167591671186,
23.3764262615133));
#33104=CARTESIAN_POINT('Ctrl Pts',(-0.843938164034378,-4.00075847420837,
23.5753591998767));
#33105=CARTESIAN_POINT('Ctrl Pts',(2.91038539296211,-2.87192563589251,23.7742921382402));
#33106=CARTESIAN_POINT('Ctrl Pts',(3.98917846904379,0.897081454373756,23.9732250766036));
#33107=CARTESIAN_POINT('Ctrl Pts',(1.40070170053866,3.8413974982774,24.1721580149671));
#33108=CARTESIAN_POINT('Ctrl Pts',(-2.47544648891397,3.25429941372752,24.3710909533305));
#33109=CARTESIAN_POINT('Ctrl Pts',(-4.07590550298146,-0.324490869562239,
24.5700238916939));
#33110=CARTESIAN_POINT('Ctrl Pts',(-1.92936611713726,-3.60497522594906,
24.7689568300574));
#33111=CARTESIAN_POINT('Ctrl Pts',(1.9908482836132,-3.57138952024253,24.9678897684208));
#33112=CARTESIAN_POINT('Ctrl Pts',(4.08086683519371,-0.254609243900974,
25.1668227067842));
#33113=CARTESIAN_POINT('Ctrl Pts',(2.41932601167626,3.29623446418644,25.3657556451477));
#33114=CARTESIAN_POINT('Ctrl Pts',(-1.46631217817726,3.81683489160756,25.5646885835111));
#33115=CARTESIAN_POINT('Ctrl Pts',(-4.00396293765922,0.828601706198546,
25.7636215218746));
#33116=CARTESIAN_POINT('Ctrl Pts',(-2.86075242355659,-2.92136878274188,
25.962554460238));
#33117=CARTESIAN_POINT('Ctrl Pts',(0.912360757761685,-3.98571171076888,
26.1614873986014));
#33118=CARTESIAN_POINT('Ctrl Pts',(3.84673655987073,-1.38597180080177,26.3604203369649));
#33119=CARTESIAN_POINT('Ctrl Pts',(3.24479001000817,2.4878982665324,26.5593532753283));
#33120=CARTESIAN_POINT('Ctrl Pts',(-0.340106700660735,4.07463218288835,
26.7582862136918));
#33121=CARTESIAN_POINT('Ctrl Pts',(-3.61234178013069,1.91553826826458,26.9572191520552));
#33122=CARTESIAN_POINT('Ctrl Pts',(-3.56373469086466,-2.00451865713232,
27.1561520904186));
#33123=CARTESIAN_POINT('Ctrl Pts',(-0.238970150300533,-4.0818124970323,
27.355085028782));
#33124=CARTESIAN_POINT('Ctrl Pts',(3.30548073238998,-2.4066776106206,27.5540179671455));
#33125=CARTESIAN_POINT('Ctrl Pts',(3.81118819815281,1.4809269097172,27.7529509055089));
#33126=CARTESIAN_POINT('Ctrl Pts',(0.813253081967926,4.00710861074834,27.9518838438724));
#33127=CARTESIAN_POINT('Ctrl Pts',(-2.93230927793693,2.84953720666863,28.1508167822358));
#33128=CARTESIAN_POINT('Ctrl Pts',(-3.98218643011584,-0.927626664917013,
28.3497497205993));
#33129=CARTESIAN_POINT('Ctrl Pts',(-1.37122155078066,-3.85201913966408,
28.5486826589627));
#33130=CARTESIAN_POINT('Ctrl Pts',(2.50031351423257,-3.23523296289614,28.7476155973261));
#33131=CARTESIAN_POINT('Ctrl Pts',(4.07329903479392,0.355717537957839,28.9465485356896));
#33132=CARTESIAN_POINT('Ctrl Pts',(1.90168229346025,3.61965529414108,29.145481474053));
#33133=CARTESIAN_POINT('Ctrl Pts',(-2.01815959821697,3.55602753501551,29.3444144124164));
#33134=CARTESIAN_POINT('Ctrl Pts',(-4.08269822544072,0.223327547890934,
29.5433473507799));
#33135=CARTESIAN_POINT('Ctrl Pts',(-2.393993872213,-3.31467846607637,29.7422802891433));
#33136=CARTESIAN_POINT('Ctrl Pts',(1.49551989674303,-3.80548554485619,29.9412132275068));
#33137=CARTESIAN_POINT('Ctrl Pts',(4.01019544728766,-0.797892516706975,
30.1401461658702));
#33138=CARTESIAN_POINT('Ctrl Pts',(2.8382801499021,2.94320671790745,30.3390791042336));
#33139=CARTESIAN_POINT('Ctrl Pts',(-0.942878951689648,3.97860267884648,
30.5380120425971));
#33140=CARTESIAN_POINT('Ctrl Pts',(-3.85724516009308,1.35645116705405,30.7369449809605));
#33141=CARTESIAN_POINT('Ctrl Pts',(-3.22562841271805,-2.51269204972075,
30.935877919324));
#33142=CARTESIAN_POINT('Ctrl Pts',(0.371323152238799,-4.07190607827283,
31.1348108576874));
#33143=CARTESIAN_POINT('Ctrl Pts',(3.62691566059552,-1.88779839617231,31.3337437960508));
#33144=CARTESIAN_POINT('Ctrl Pts',(3.54826816585965,2.03177090657653,31.5326767344143));
#33145=CARTESIAN_POINT('Ctrl Pts',(0.207681666353341,4.08352400741375,31.7316096727777));
#33146=CARTESIAN_POINT('Ctrl Pts',(-3.32382753019483,2.38127498268946,31.9305426111411));
#33147=CARTESIAN_POINT('Ctrl Pts',(-3.79972701545007,-1.51009092498523,
32.1294755495046));
#33148=CARTESIAN_POINT('Ctrl Pts',(-0.782520235955546,-4.01322340195306,
32.328408487868));
#33149=CARTESIAN_POINT('Ctrl Pts',(2.9540609426459,-2.82698141854484,32.5273414262314));
#33150=CARTESIAN_POINT('Ctrl Pts',(3.97496050958118,0.958117394129718,32.7262743645949));
#33151=CARTESIAN_POINT('Ctrl Pts',(1.34166086649601,3.86241454442386,32.9252073029583));
#33152=CARTESIAN_POINT('Ctrl Pts',(-2.52503369124243,3.21597650049785,33.1241402413218));
#33153=CARTESIAN_POINT('Ctrl Pts',(-4.07045333377795,-0.38692331436581,
33.3230731796852));
#33154=CARTESIAN_POINT('Ctrl Pts',(-1.87388678025847,-3.63412277288981,
33.5220061180486));
#33155=CARTESIAN_POINT('Ctrl Pts',(2.04535238235562,-3.54045669732818,33.720939056412));
#33156=CARTESIAN_POINT('Ctrl Pts',(4.08428983082642,-0.192032735416775,
33.9198719947756));
#33157=CARTESIAN_POINT('Ctrl Pts',(2.36852112880191,3.3329277904093,34.1188049331389));
#33158=CARTESIAN_POINT('Ctrl Pts',(-1.5246397804968,3.79391269448716,34.3177378715024));
#33159=CARTESIAN_POINT('Ctrl Pts',(-4.01619243028494,0.767136465425386,
34.5166708098658));
#33160=CARTESIAN_POINT('Ctrl Pts',(-2.81564117849665,-2.96487179277909,
34.7156037482293));
#33161=CARTESIAN_POINT('Ctrl Pts',(0.973341768490662,-3.97125997579838,
34.9145366865927));
#33162=CARTESIAN_POINT('Ctrl Pts',(3.8675272167539,-1.32685086627251,35.1134696249562));
#33163=CARTESIAN_POINT('Ctrl Pts',(3.20627736795542,2.53733825758359,35.3124025633196));
#33164=CARTESIAN_POINT('Ctrl Pts',(-0.402517795281907,4.06894082264232,
35.511335501683));
#33165=CARTESIAN_POINT('Ctrl Pts',(-3.64127652519993,1.85994764997906,35.7102684400464));
#33166=CARTESIAN_POINT('Ctrl Pts',(-3.53259324412043,-2.0589038261282,35.9092013784099));
#33167=CARTESIAN_POINT('Ctrl Pts',(-0.176380984849015,-4.08499568445078,
36.1081343167733));
#33168=CARTESIAN_POINT('Ctrl Pts',(3.34197911308852,-2.35573249778373,36.3070672551368));
#33169=CARTESIAN_POINT('Ctrl Pts',(3.78804266736189,1.53916624959495,36.5060001935002));
#33170=CARTESIAN_POINT('Ctrl Pts',(0.751741430954012,4.0191024888065,36.7049331318636));
#33171=CARTESIAN_POINT('Ctrl Pts',(-2.97563910948809,2.80425959604127,36.9038660702271));
#33172=CARTESIAN_POINT('Ctrl Pts',(-3.96750113199172,-0.988551850799671,
37.1027990085905));
#33173=CARTESIAN_POINT('Ctrl Pts',(-1.31202138353558,-3.87258310284293,
37.301731946954));
#33174=CARTESIAN_POINT('Ctrl Pts',(2.54960556749285,-3.19653115591342,37.5006648853174));
#33175=CARTESIAN_POINT('Ctrl Pts',(4.06736856819161,0.418106362963447,37.6995978236809));
#33176=CARTESIAN_POINT('Ctrl Pts',(1.84598120786055,3.64837681833342,37.8985307620442));
#33177=CARTESIAN_POINT('Ctrl Pts',(-2.07242503480969,3.52467791048579,38.0974637004078));
#33178=CARTESIAN_POINT('Ctrl Pts',(-4.0856415657996,0.160726665959935,38.2963966387711));
#33179=CARTESIAN_POINT('Ctrl Pts',(-2.34290926230782,-3.3509814065453,38.4953295771346));
#33180=CARTESIAN_POINT('Ctrl Pts',(1.5536700900277,-3.78211694123996,38.694262515498));
#33181=CARTESIAN_POINT('Ctrl Pts',(4.02195359031618,-0.736335510109945,
38.8931954538615));
#33182=CARTESIAN_POINT('Ctrl Pts',(2.79283673182646,2.98636302520864,39.0921283922249));
#33183=CARTESIAN_POINT('Ctrl Pts',(-1.00374721358184,3.96368347627922,39.2910613305884));
#33184=CARTESIAN_POINT('Ctrl Pts',(-3.87758251988644,1.29717370417073,39.4899942689517));
#33185=CARTESIAN_POINT('Ctrl Pts',(-3.18673725693753,-2.56183748892951,
39.6889272073153));
#33186=CARTESIAN_POINT('Ctrl Pts',(0.433687349425391,-4.06573266647945,
39.8878601456786));
#33187=CARTESIAN_POINT('Ctrl Pts',(3.65542630739156,-1.83199518874432,40.0867930840421));
#33188=CARTESIAN_POINT('Ctrl Pts',(3.51670552180105,2.08593024760723,40.2857260224055));
#33189=CARTESIAN_POINT('Ctrl Pts',(0.145080153377126,4.08619978216286,40.484658960769));
#33190=CARTESIAN_POINT('Ctrl Pts',(-3.35995399040756,2.33010469112103,40.6835918991324));
#33191=CARTESIAN_POINT('Ctrl Pts',(-3.77609830574217,-1.56825286709605,
40.8825248374958));
#33192=CARTESIAN_POINT('Ctrl Pts',(-0.720990444685169,-4.02455053491554,
41.0814577758593));
#33193=CARTESIAN_POINT('Ctrl Pts',(2.99718051531959,-2.78174701105068,41.2803907142227));
#33194=CARTESIAN_POINT('Ctrl Pts',(3.9595440561214,1.01964576599861,41.4793236525862));
#33195=CARTESIAN_POINT('Ctrl Pts',(1.28281295705702,3.88114366634645,41.6782565909495));
#33196=CARTESIAN_POINT('Ctrl Pts',(-2.57500755361336,3.17958857837247,41.8771895293131));
#33197=CARTESIAN_POINT('Ctrl Pts',(-4.0621147000577,-0.454817851921865,
42.0761224676764));
#33198=CARTESIAN_POINT('Ctrl Pts',(-2.56886110523792,-2.5838694518668,42.2087444265854));
#33199=CARTESIAN_POINT('Ctrl Pts',(-1.53687260224456,-3.09613266190232,
42.2750554060399));
#33200=CARTESIAN_POINT('Ctrl Pts',(-1.86645400133787,2.62012303844274,7.00322156819806));
#33201=CARTESIAN_POINT('Ctrl Pts',(-2.74041061257865,1.997626899089,7.0695770455426));
#33202=CARTESIAN_POINT('Ctrl Pts',(-3.80025934494349,-0.179501204411249,
7.20224350234162));
#33203=CARTESIAN_POINT('Ctrl Pts',(-1.89809237229961,-3.30104156426044,
7.40122093859512));
#33204=CARTESIAN_POINT('Ctrl Pts',(1.75033879183918,-3.37766291872948,7.60015387695855));
#33205=CARTESIAN_POINT('Ctrl Pts',(3.78874883692714,-0.353950369213094,
7.79908681532199));
#33206=CARTESIAN_POINT('Ctrl Pts',(2.34462897392162,2.99761246260044,7.99801975368543));
#33207=CARTESIAN_POINT('Ctrl Pts',(-1.25517146953415,3.59217513842517,8.19695269204886));
#33208=CARTESIAN_POINT('Ctrl Pts',(-3.70095537602795,0.885102952948687,
8.39588563041231));
#33209=CARTESIAN_POINT('Ctrl Pts',(-2.74450292932235,-2.63599675282763,
8.59481856877575));
#33210=CARTESIAN_POINT('Ctrl Pts',(0.735019325049069,-3.73363101754262,
8.79375150713918));
#33211=CARTESIAN_POINT('Ctrl Pts',(3.53881629779805,-1.39901612008267,8.99268444550262));
#33212=CARTESIAN_POINT('Ctrl Pts',(3.08937315587434,2.22177005300786,9.19161738386606));
#33213=CARTESIAN_POINT('Ctrl Pts',(-0.200149810864368,3.80004717549578,
9.3905503222295));
#33214=CARTESIAN_POINT('Ctrl Pts',(-3.30567149883918,1.88493714980744,9.58948326059294));
#33215=CARTESIAN_POINT('Ctrl Pts',(-3.37227577980602,-1.76301114979847,
9.78841619895636));
#33216=CARTESIAN_POINT('Ctrl Pts',(-0.338730933097911,-3.79021165389004,
9.98734913731983));
#33217=CARTESIAN_POINT('Ctrl Pts',(3.00621041944956,-2.33305531494441,10.1862820756832));
#33218=CARTESIAN_POINT('Ctrl Pts',(3.58752910607548,1.26889034228732,10.3852150140467));
#33219=CARTESIAN_POINT('Ctrl Pts',(0.870815925397089,3.70433883892876,10.5841479524101));
#33220=CARTESIAN_POINT('Ctrl Pts',(-2.64644222848811,2.73437212425091,10.7830808907735));
#33221=CARTESIAN_POINT('Ctrl Pts',(-3.73081407650405,-0.749315416829459,
10.9820138291369));
#33222=CARTESIAN_POINT('Ctrl Pts',(-1.38543162233216,-3.54415382593228,
11.1809467675004));
#33223=CARTESIAN_POINT('Ctrl Pts',(2.23358439312533,-3.08083559997405,11.3798797058638));
#33224=CARTESIAN_POINT('Ctrl Pts',(3.79925615786297,0.214708774655039,11.5788126442273));
#33225=CARTESIAN_POINT('Ctrl Pts',(1.87225451730644,3.31287038929909,11.7777455825907));
#33226=CARTESIAN_POINT('Ctrl Pts',(-1.77591918454253,3.36549524737367,11.9766785209541));
#33227=CARTESIAN_POINT('Ctrl Pts',(-3.79148233256386,0.32420507008613,12.1756114593176));
#33228=CARTESIAN_POINT('Ctrl Pts',(-2.32151858988368,-3.01512829587034,
12.374544397681));
#33229=CARTESIAN_POINT('Ctrl Pts',(1.28262771288672,-3.58264055637097,12.5734773360444));
#33230=CARTESIAN_POINT('Ctrl Pts',(3.70764854672028,-0.85661511733405,12.7724102744079));
#33231=CARTESIAN_POINT('Ctrl Pts',(2.72421126934337,2.65690048083118,12.9713432127713));
#33232=CARTESIAN_POINT('Ctrl Pts',(-0.763605773387818,3.72791542664558,
13.1702761511348));
#33233=CARTESIAN_POINT('Ctrl Pts',(-3.54943656817764,1.37184082667385,13.3692090894982));
#33234=CARTESIAN_POINT('Ctrl Pts',(-3.0722542406453,-2.24537326208117,13.5681420278616));
#33235=CARTESIAN_POINT('Ctrl Pts',(0.229265333024543,-3.79840553553036,
13.7670749662251));
#33236=CARTESIAN_POINT('Ctrl Pts',(3.32002024707132,-1.85954638670049,13.9660079045885));
#33237=CARTESIAN_POINT('Ctrl Pts',(3.35866550245346,1.78880218243472,14.164940842952));
#33238=CARTESIAN_POINT('Ctrl Pts',(0.309674340768458,3.79269679883976,14.3638737813154));
#33239=CARTESIAN_POINT('Ctrl Pts',(-3.02400184575466,2.30994806048298,14.5628067196789));
#33240=CARTESIAN_POINT('Ctrl Pts',(-3.57769943142826,-1.29634639800277,
14.7617396580423));
#33241=CARTESIAN_POINT('Ctrl Pts',(-0.842401716518874,-3.71090373807563,
14.9606725964057));
#33242=CARTESIAN_POINT('Ctrl Pts',(2.66731971394778,-2.71401045481454,15.1596055347691));
#33243=CARTESIAN_POINT('Ctrl Pts',(3.72496204373251,0.777884938798361,15.3585384731326));
#33244=CARTESIAN_POINT('Ctrl Pts',(1.35822988608424,3.55466718298702,15.557471411496));
#33245=CARTESIAN_POINT('Ctrl Pts',(-2.25712916101158,3.06362777696122,15.7564043498595));
#33246=CARTESIAN_POINT('Ctrl Pts',(-3.7974991416244,-0.243818528047306,
15.9553372882229));
#33247=CARTESIAN_POINT('Ctrl Pts',(-1.84681095199157,-3.32712135529518,
16.1542702265864));
#33248=CARTESIAN_POINT('Ctrl Pts',(1.80165891510899,-3.35178644290854,16.3532031649498));
#33249=CARTESIAN_POINT('Ctrl Pts',(3.79385557686611,-0.295139064068223,
16.5521361033133));
#33250=CARTESIAN_POINT('Ctrl Pts',(2.29834361397166,3.03283099386907,16.7510690416766));
#33251=CARTESIAN_POINT('Ctrl Pts',(-1.31004604878593,3.57270577508387,16.9500019800401));
#33252=CARTESIAN_POINT('Ctrl Pts',(-3.71410444208186,0.828175946623051,
17.1489349184035));
#33253=CARTESIAN_POINT('Ctrl Pts',(-2.70376979034626,-2.677699782662,17.347867856767));
#33254=CARTESIAN_POINT('Ctrl Pts',(0.792152682487336,-3.7219539670562,17.5468007951304));
#33255=CARTESIAN_POINT('Ctrl Pts',(3.55984560446539,-1.3445990025378,17.7457337334939));
#33256=CARTESIAN_POINT('Ctrl Pts',(3.05495632989659,2.26885191841203,17.9446666718573));
#33257=CARTESIAN_POINT('Ctrl Pts',(-0.25836814307153,3.79653698887591,18.1435996102207));
#33258=CARTESIAN_POINT('Ctrl Pts',(-3.33417361125188,1.83404840047608,18.3425325485842));
#33259=CARTESIAN_POINT('Ctrl Pts',(-3.34485816893761,-1.8144891939465,18.5414654869476));
#33260=CARTESIAN_POINT('Ctrl Pts',(-0.280599453828384,-3.79495864954658,
18.740398425311));
#33261=CARTESIAN_POINT('Ctrl Pts',(3.04161561079433,-2.28670542078106,18.9393313636745));
#33262=CARTESIAN_POINT('Ctrl Pts',(3.56765966054535,1.32372646410603,19.1382643020379));
#33263=CARTESIAN_POINT('Ctrl Pts',(0.813938016583792,3.71725061173132,19.3371972404014));
#33264=CARTESIAN_POINT('Ctrl Pts',(-2.68804053459405,2.69348942630865,19.5361301787648));
#33265=CARTESIAN_POINT('Ctrl Pts',(-3.71889124076811,-0.8064087949641,19.7350631171283));
#33266=CARTESIAN_POINT('Ctrl Pts',(-1.33094837618574,-3.56497175657617,
19.9339960554916));
#33267=CARTESIAN_POINT('Ctrl Pts',(2.28054136216125,-3.04624002677545,20.1329289938551));
#33268=CARTESIAN_POINT('Ctrl Pts',(3.79551909140992,0.272913964465135,20.3318619322185));
#33269=CARTESIAN_POINT('Ctrl Pts',(1.8212589195482,3.34117691139266,20.530794870582));
#33270=CARTESIAN_POINT('Ctrl Pts',(-1.8272928305604,3.33788078226886,20.7297278089454));
#33271=CARTESIAN_POINT('Ctrl Pts',(-3.79600600068437,0.266055723534535,
20.9286607473089));
#33272=CARTESIAN_POINT('Ctrl Pts',(-2.27503365179541,-3.05035556754547,
21.1275936856723));
#33273=CARTESIAN_POINT('Ctrl Pts',(1.33738744309295,-3.56256116190508,21.3265266240357));
#33274=CARTESIAN_POINT('Ctrl Pts',(3.72034220082859,-0.799688135457281,
21.5254595623992));
#33275=CARTESIAN_POINT('Ctrl Pts',(2.6831695136488,2.69834181791016,21.7243925007626));
#33276=CARTESIAN_POINT('Ctrl Pts',(-0.820653066905469,3.7157739098384,21.923325439126));
#33277=CARTESIAN_POINT('Ctrl Pts',(-3.57004556405178,1.31727820746093,22.1222583774895));
#33278=CARTESIAN_POINT('Ctrl Pts',(-3.03747899557971,-2.29219732062257,
22.3211913158529));
#33279=CARTESIAN_POINT('Ctrl Pts',(0.287455778651096,-3.79444546417224,
22.5201242542163));
#33280=CARTESIAN_POINT('Ctrl Pts',(3.34813115288769,-1.80844269699657,22.7190571925798));
#33281=CARTESIAN_POINT('Ctrl Pts',(3.33085438535164,1.84006963695426,22.9179901309432));
#33282=CARTESIAN_POINT('Ctrl Pts',(0.251508086732996,3.79699761490117,23.1169230693067));
#33283=CARTESIAN_POINT('Ctrl Pts',(-3.0590507357933,2.26332847839188,23.3158560076701));
#33284=CARTESIAN_POINT('Ctrl Pts',(-3.55741035402456,-1.35102878516191,
23.5147889460336));
#33285=CARTESIAN_POINT('Ctrl Pts',(-0.785426512475196,-3.72337916397971,
23.7137218843969));
#33286=CARTESIAN_POINT('Ctrl Pts',(2.70860348135616,-2.67281020389449,23.9126548227604));
#33287=CARTESIAN_POINT('Ctrl Pts',(3.71260202003901,0.83488528916224,24.1115877611238));
#33288=CARTESIAN_POINT('Ctrl Pts',(1.30358869708293,3.57506695239331,24.3105206994873));
#33289=CARTESIAN_POINT('Ctrl Pts',(-2.3038196226511,3.02867336494793,24.5094536378507));
#33290=CARTESIAN_POINT('Ctrl Pts',(-3.79331612292701,-0.301993372111428,
24.7083865762142));
#33291=CARTESIAN_POINT('Ctrl Pts',(-1.7955999210022,-3.35503623362761,24.9073195145776));
#33292=CARTESIAN_POINT('Ctrl Pts',(1.85281942552575,-3.32377908135478,25.1062524529411));
#33293=CARTESIAN_POINT('Ctrl Pts',(3.79793347763706,-0.23695675702724,25.3051853913045));
#33294=CARTESIAN_POINT('Ctrl Pts',(2.25159007243797,3.06770098786632,25.5041183296679));
#33295=CARTESIAN_POINT('Ctrl Pts',(-1.36465029001659,3.55220731253327,25.7030512680313));
#33296=CARTESIAN_POINT('Ctrl Pts',(-3.72636145659287,0.771153357041461,
25.9019842063948));
#33297=CARTESIAN_POINT('Ctrl Pts',(-2.66241164915182,-2.7188253742596,26.1009171447582));
#33298=CARTESIAN_POINT('Ctrl Pts',(0.849105252762015,-3.70937561794287,
26.2998500831217));
#33299=CARTESIAN_POINT('Ctrl Pts',(3.58003584787151,-1.28988004605551,26.4987830214851));
#33300=CARTESIAN_POINT('Ctrl Pts',(3.01982326417359,2.31540809759601,26.6977159598485));
#33301=CARTESIAN_POINT('Ctrl Pts',(-0.316526531389901,3.79213108425639,
26.896648898212));
#33302=CARTESIAN_POINT('Ctrl Pts',(-3.36189205222476,1.78273078013626,27.0955818365754));
#33303=CARTESIAN_POINT('Ctrl Pts',(-3.31665497416533,-1.86554200906911,
27.294514774939));
#33304=CARTESIAN_POINT('Ctrl Pts',(-0.222401948075185,-3.79881357515075,
27.4934477133024));
#33305=CARTESIAN_POINT('Ctrl Pts',(3.07630619675248,-2.23981860628926,27.6923806516658));
#33306=CARTESIAN_POINT('Ctrl Pts',(3.54695211382774,1.37825175765173,27.8913135900291));
#33307=CARTESIAN_POINT('Ctrl Pts',(0.756868878729541,3.72928903487889,28.0902465283926));
#33308=CARTESIAN_POINT('Ctrl Pts',(-2.72900734653197,2.65197400210329,28.2891794667561));
#33309=CARTESIAN_POINT('Ctrl Pts',(-3.70609475092345,-0.863312748912513,
28.4881124051195));
#33310=CARTESIAN_POINT('Ctrl Pts',(-1.27615245566332,-3.58495217752786,
28.6870453434829));
#33311=CARTESIAN_POINT('Ctrl Pts',(2.32696257530329,-3.01092882320308,28.8859782818464));
#33312=CARTESIAN_POINT('Ctrl Pts',(3.79089036556033,0.331055043095624,29.0849112202098));
#33313=CARTESIAN_POINT('Ctrl Pts',(1.7698354633568,3.36869850801491,29.2838441585732));
#33314=CARTESIAN_POINT('Ctrl Pts',(-1.87823720077816,3.3094821683868,29.4827770969367));
#33315=CARTESIAN_POINT('Ctrl Pts',(-3.79963789451971,0.207843873585611,
29.6817100353001));
#33316=CARTESIAN_POINT('Ctrl Pts',(-2.22801425278663,-3.08486623610115,
29.8806429736635));
#33317=CARTESIAN_POINT('Ctrl Pts',(1.39183298835648,-3.54164483507025,30.079575912027));
#33318=CARTESIAN_POINT('Ctrl Pts',(3.73216185585201,-0.742573287279,30.2785088503904));
#33319=CARTESIAN_POINT('Ctrl Pts',(2.64149741600532,2.73914924867091,30.4774417887539));
#33320=CARTESIAN_POINT('Ctrl Pts',(-0.877507569004345,3.70275946715383,
30.6763747271173));
#33321=CARTESIAN_POINT('Ctrl Pts',(-3.58981586917566,1.26240612746925,30.8753076654808));
#33322=CARTESIAN_POINT('Ctrl Pts',(-3.00199017263393,-2.33848288611794,
31.0742406038442));
#33323=CARTESIAN_POINT('Ctrl Pts',(0.345578693905692,-3.78959398505641,
31.2731735422076));
#33324=CARTESIAN_POINT('Ctrl Pts',(3.37545550105851,-1.75691416000643,31.4721064805712));
#33325=CARTESIAN_POINT('Ctrl Pts',(3.3022607693379,1.89090481424875,31.6710394189345));
#33326=CARTESIAN_POINT('Ctrl Pts',(0.193282747315501,3.80040642364043,31.8699723572979));
#33327=CARTESIAN_POINT('Ctrl Pts',(-3.09338098022485,2.216177185254,32.0689052956615));
#33328=CARTESIAN_POINT('Ctrl Pts',(-3.53628555418785,-1.40539378271698,
32.2678382340249));
#33329=CARTESIAN_POINT('Ctrl Pts',(-0.728266792592632,-3.73497987733052,
32.4667711723883));
#33330=CARTESIAN_POINT('Ctrl Pts',(2.74925093176247,-2.63098204468606,32.6657041107517));
#33331=CARTESIAN_POINT('Ctrl Pts',(3.69936981560612,0.891689504614469,32.8646370491151));
#33332=CARTESIAN_POINT('Ctrl Pts',(1.24864126331116,3.59462685140112,33.0635699874787));
#33333=CARTESIAN_POINT('Ctrl Pts',(-2.34996886088683,2.99300744371268,33.262502925842));
#33334=CARTESIAN_POINT('Ctrl Pts',(-3.78824196177939,-0.360097270568816,
33.4614358642054));
#33335=CARTESIAN_POINT('Ctrl Pts',(-1.74396705980911,-3.38216293214238,
33.660368802569));
#33336=CARTESIAN_POINT('Ctrl Pts',(1.90354466348184,-3.29499088305067,33.8593017409324));
#33337=CARTESIAN_POINT('Ctrl Pts',(3.80111915122855,-0.17871878306637,34.0582346792959));
#33338=CARTESIAN_POINT('Ctrl Pts',(2.20430757749551,3.10185030410124,34.2571676176593));
#33339=CARTESIAN_POINT('Ctrl Pts',(-1.41893394161954,3.5308743498711,34.4561005560226));
#33340=CARTESIAN_POINT('Ctrl Pts',(-3.73774305793726,0.713949604733199,
34.6550334943861));
#33341=CARTESIAN_POINT('Ctrl Pts',(-2.62042804254318,-2.75931224748304,
34.8539664327496));
#33342=CARTESIAN_POINT('Ctrl Pts',(0.90585834750904,-3.69592584605102,35.052899371113));
#33343=CARTESIAN_POINT('Ctrl Pts',(3.59938505356419,-1.23485806529853,35.2518323094765));
#33344=CARTESIAN_POINT('Ctrl Pts',(2.98398076833351,2.36142033095977,35.4507652478398));
#33345=CARTESIAN_POINT('Ctrl Pts',(-0.374610559908926,3.7868343155833,35.6496981862033));
#33346=CARTESIAN_POINT('Ctrl Pts',(-3.3888207027795,1.73099435286343,35.8486311245668));
#33347=CARTESIAN_POINT('Ctrl Pts',(-3.28767261627215,-1.91615656287791,
36.0475640629301));
#33348=CARTESIAN_POINT('Ctrl Pts',(-0.164152194675816,-3.80177606683461,
36.2464970012937));
#33349=CARTESIAN_POINT('Ctrl Pts',(3.11027408336399,-2.1924056037633,36.445429939657));
#33350=CARTESIAN_POINT('Ctrl Pts',(3.52541130159383,1.43245326619635,36.6443628780206));
#33351=CARTESIAN_POINT('Ctrl Pts',(0.699621933880535,3.74045135720976,36.843295816384));
#33352=CARTESIAN_POINT('Ctrl Pts',(-2.76933304802493,2.60983556433168,37.0422287547475));
#33353=CARTESIAN_POINT('Ctrl Pts',(-3.69242760920404,-0.920013889243654,
37.2411616931107));
#33354=CARTESIAN_POINT('Ctrl Pts',(-1.22105673552787,-3.60409040657181,
37.4400946314743));
#33355=CARTESIAN_POINT('Ctrl Pts',(2.37283712765188,-2.9749102775556,37.6390275698377));
#33356=CARTESIAN_POINT('Ctrl Pts',(3.7853710681766,0.389118345988962,37.8379605082012));
#33357=CARTESIAN_POINT('Ctrl Pts',(1.71799622765437,3.39542872065456,38.0368934465646));
#33358=CARTESIAN_POINT('Ctrl Pts',(-1.92874032343257,3.28030606602396,38.235826384928));
#33359=CARTESIAN_POINT('Ctrl Pts',(-3.80237716814379,0.149583216029986,
38.4347593232914));
#33360=CARTESIAN_POINT('Ctrl Pts',(-2.1804714247586,-3.1186522326827,38.633692261655));
#33361=CARTESIAN_POINT('Ctrl Pts',(1.44595153099118,-3.51989641602498,38.8326252000182));
#33362=CARTESIAN_POINT('Ctrl Pts',(3.74310478705912,-0.685284131425703,
39.0315581383817));
#33363=CARTESIAN_POINT('Ctrl Pts',(2.59920466649454,2.77931345664184,39.2304910767451));
#33364=CARTESIAN_POINT('Ctrl Pts',(-0.934155731980976,3.68887463797949,
39.4294240151087));
#33365=CARTESIAN_POINT('Ctrl Pts',(-3.60874320562774,1.20723847073212,39.628356953472));
#33366=CARTESIAN_POINT('Ctrl Pts',(-2.9657954060591,-2.38422098941366,39.8272898918356));
#33367=CARTESIAN_POINT('Ctrl Pts',(0.403619076468115,-3.78384858628005,
40.0262228301989));
#33368=CARTESIAN_POINT('Ctrl Pts',(3.40198945678621,-1.70497988275374,40.2251557685625));
#33369=CARTESIAN_POINT('Ctrl Pts',(3.27288641644818,1.9413091971248,40.4240887069258));
#33370=CARTESIAN_POINT('Ctrl Pts',(0.135021502466078,3.80289668242824,40.6230216452892));
#33371=CARTESIAN_POINT('Ctrl Pts',(-3.12700273222302,2.16855461601647,40.8219545836528));
#33372=CARTESIAN_POINT('Ctrl Pts',(-3.51429506264349,-1.45952325961196,
41.020887522016));
#33373=CARTESIAN_POINT('Ctrl Pts',(-0.671002965181634,-3.74552168112398,
41.2198204603797));
#33374=CARTESIAN_POINT('Ctrl Pts',(2.78938095197937,-2.58888381470178,41.418753398743));
#33375=CARTESIAN_POINT('Ctrl Pts',(3.68502221077952,0.948952011033468,41.6176863371064));
#33376=CARTESIAN_POINT('Ctrl Pts',(1.19387337835599,3.61205745181745,41.8166192754698));
#33377=CARTESIAN_POINT('Ctrl Pts',(-2.39647795137431,2.95914235739577,42.0155522138333));
#33378=CARTESIAN_POINT('Ctrl Pts',(-3.78048145955207,-0.423284565706465,
42.2144851521968));
#33379=CARTESIAN_POINT('Ctrl Pts',(-2.39075764659687,-2.40472543932513,
42.3471071111058));
#33380=CARTESIAN_POINT('Ctrl Pts',(-1.43031864127241,-2.88147257990253,
42.4134180905602));
#33381=CARTESIAN_POINT('',(-1.87386922097,2.62532148205406,42.0016066797527));
#33382=CARTESIAN_POINT('Ctrl Pts',(-1.87561919562493,2.62751776731827,42.));
#33383=CARTESIAN_POINT('Ctrl Pts',(-1.93354241972396,2.5952533695629,42.));
#33384=CARTESIAN_POINT('Ctrl Pts',(-1.99028258208655,2.56113722808904,42.));
#33385=CARTESIAN_POINT('Ctrl Pts',(-2.04574119823645,2.52519298213882,42.));
#33386=CARTESIAN_POINT('Ctrl Pts',(-2.13151874516022,2.46959820791473,42.));
#33387=CARTESIAN_POINT('Ctrl Pts',(-2.21423174799282,2.40963304771824,42.));
#33388=CARTESIAN_POINT('Ctrl Pts',(-2.29379848781349,2.34570550738362,42.));
#33389=CARTESIAN_POINT('Ctrl Pts',(-2.37493421037037,2.28051737490485,42.));
#33390=CARTESIAN_POINT('Ctrl Pts',(-2.45279884777719,2.21120864124839,42.));
#33391=CARTESIAN_POINT('Ctrl Pts',(-2.52728671613257,2.13816044108625,42.));
#33392=CARTESIAN_POINT('Ctrl Pts',(-2.60344111362154,2.06347792172002,42.));
#33393=CARTESIAN_POINT('Ctrl Pts',(-2.67606653870818,1.98488624906051,42.));
#33394=CARTESIAN_POINT('Ctrl Pts',(-2.7450221352932,1.90274628377322,42.));
#33395=CARTESIAN_POINT('Ctrl Pts',(-2.7679416471307,1.87544454178317,42.));
#33396=CARTESIAN_POINT('Ctrl Pts',(-2.79045546383387,1.84775045492808,42.));
#33397=CARTESIAN_POINT('Ctrl Pts',(-2.81255757521727,1.81967632547802,42.));
#33398=CARTESIAN_POINT('Ctrl Pts',(-2.82452315241262,1.80447763439825,42.));
#33399=CARTESIAN_POINT('Ctrl Pts',(-2.83636967025138,1.78916527706112,42.));
#33400=CARTESIAN_POINT('Ctrl Pts',(-2.84808157918788,1.77376072408085,42.));
#33401=CARTESIAN_POINT('Ctrl Pts',(-2.91426840109589,1.68670588014324,42.));
#33402=CARTESIAN_POINT('Ctrl Pts',(-2.9762581387323,1.59658638019521,42.));
#33403=CARTESIAN_POINT('Ctrl Pts',(-3.03395163488204,1.50383670327667,42.));
#33404=CARTESIAN_POINT('Ctrl Pts',(-3.09256319399938,1.40961112267194,42.));
#33405=CARTESIAN_POINT('Ctrl Pts',(-3.14674125704714,1.31267038210085,42.));
#33406=CARTESIAN_POINT('Ctrl Pts',(-3.19635290330767,1.21342331376483,42.));
#33407=CARTESIAN_POINT('Ctrl Pts',(-3.246323219868,1.11345873294058,42.));
#33408=CARTESIAN_POINT('Ctrl Pts',(-3.29166142466647,1.01115361908758,42.));
#33409=CARTESIAN_POINT('Ctrl Pts',(-3.3321940140089,0.906889032325619,42.));
#33410=CARTESIAN_POINT('Ctrl Pts',(-3.36732123477664,0.816529022840346,
42.));
#33411=CARTESIAN_POINT('Ctrl Pts',(-3.39883874146856,0.724696427496403,
42.));
#33412=CARTESIAN_POINT('Ctrl Pts',(-3.42660590875194,0.631623878310208,
42.));
#33413=CARTESIAN_POINT('Ctrl Pts',(-3.43064581025193,0.618082564310531,
42.));
#33414=CARTESIAN_POINT('Ctrl Pts',(-3.43460572040773,0.604516718988522,
42.));
#33415=CARTESIAN_POINT('Ctrl Pts',(-3.43848278257111,0.590935988110032,
42.));
#33416=CARTESIAN_POINT('Ctrl Pts',(-3.47005193987078,0.480354261204366,
42.));
#33417=CARTESIAN_POINT('Ctrl Pts',(-3.49618062575215,0.368624547072095,
42.));
#33418=CARTESIAN_POINT('Ctrl Pts',(-3.51673450065987,0.256176968912335,
42.));
#33419=CARTESIAN_POINT('Ctrl Pts',(-3.53722326495676,0.144085602441787,
42.));
#33420=CARTESIAN_POINT('Ctrl Pts',(-3.55217297423634,0.0312800672726983,
42.));
#33421=CARTESIAN_POINT('Ctrl Pts',(-3.56140895218783,-0.0818433222640444,
42.));
#33422=CARTESIAN_POINT('Ctrl Pts',(-3.56994174233481,-0.186353981417057,
42.));
#33423=CARTESIAN_POINT('Ctrl Pts',(-3.57359760697331,-0.291136756602193,
42.));
#33424=CARTESIAN_POINT('Ctrl Pts',(-3.5722015224377,-0.395892400984094,
42.));
#33425=CARTESIAN_POINT('Ctrl Pts',(-3.57116204802633,-0.473889691980635,
42.));
#33426=CARTESIAN_POINT('Ctrl Pts',(-3.56732114613858,-0.551872243847325,
42.));
#33427=CARTESIAN_POINT('Ctrl Pts',(-3.56075455121097,-0.629742381860636,
42.));
#33428=CARTESIAN_POINT('Ctrl Pts',(-3.55856422692781,-0.655716399765561,
42.));
#33429=CARTESIAN_POINT('Ctrl Pts',(-3.55607053983388,-0.681677912787002,
42.));
#33430=CARTESIAN_POINT('Ctrl Pts',(-3.55327599217611,-0.707623291232608,
42.));
#33431=CARTESIAN_POINT('Ctrl Pts',(-3.55103199554422,-0.728457196742502,
42.));
#33432=CARTESIAN_POINT('Ctrl Pts',(-3.54859343660888,-0.749284406114006,
42.));
#33433=CARTESIAN_POINT('Ctrl Pts',(-3.54596521901003,-0.770076248997231,
42.));
#33434=CARTESIAN_POINT('Ctrl Pts',(-3.53185443093333,-0.881706765731404,
42.));
#33435=CARTESIAN_POINT('Ctrl Pts',(-3.51226715074755,-0.992463613106634,
42.));
#33436=CARTESIAN_POINT('Ctrl Pts',(-3.48751798321568,-1.10205172963754,
42.));
#33437=CARTESIAN_POINT('Ctrl Pts',(-3.46230882163008,-1.2136766775851,42.));
#33438=CARTESIAN_POINT('Ctrl Pts',(-3.43174398907026,-1.32408968730896,
42.));
#33439=CARTESIAN_POINT('Ctrl Pts',(-3.39610122197234,-1.43298776326768,
42.));
#33440=CARTESIAN_POINT('Ctrl Pts',(-3.35972906008411,-1.5441143331326,42.));
#33441=CARTESIAN_POINT('Ctrl Pts',(-3.31806887336794,-1.65366408568259,
42.));
#33442=CARTESIAN_POINT('Ctrl Pts',(-3.27136124123191,-1.7613134609039,42.));
#33443=CARTESIAN_POINT('Ctrl Pts',(-3.23281667986467,-1.85014900575188,
42.));
#33444=CARTESIAN_POINT('Ctrl Pts',(-3.19083369759702,-1.93769056532194,
42.));
#33445=CARTESIAN_POINT('Ctrl Pts',(-3.14552159514942,-2.02374982253641,
42.));
#33446=CARTESIAN_POINT('Ctrl Pts',(-3.1353496479755,-2.04306894857399,42.));
#33447=CARTESIAN_POINT('Ctrl Pts',(-3.12500984414154,-2.06231334028129,
42.));
#33448=CARTESIAN_POINT('Ctrl Pts',(-3.11450326876925,-2.081480800172,42.));
#33449=CARTESIAN_POINT('Ctrl Pts',(-3.10547118925435,-2.09795829314162,
42.));
#33450=CARTESIAN_POINT('Ctrl Pts',(-3.09632042674677,-2.11437056920114,
42.));
#33451=CARTESIAN_POINT('Ctrl Pts',(-3.08705381289204,-2.13071331918172,
42.));
#33452=CARTESIAN_POINT('Ctrl Pts',(-3.02769650863937,-2.23539682041853,
42.));
#33453=CARTESIAN_POINT('Ctrl Pts',(-2.9635677965333,-2.33726880643937,42.));
#33454=CARTESIAN_POINT('Ctrl Pts',(-2.89494192545328,-2.43599574081051,
42.));
#33455=CARTESIAN_POINT('Ctrl Pts',(-2.82581314326201,-2.53544617597652,
42.));
#33456=CARTESIAN_POINT('Ctrl Pts',(-2.75212073730953,-2.63170612789041,
42.));
#33457=CARTESIAN_POINT('Ctrl Pts',(-2.67409458472159,-2.72442029741163,
42.));
#33458=CARTESIAN_POINT('Ctrl Pts',(-2.63882178662635,-2.76633301607867,
42.));
#33459=CARTESIAN_POINT('Ctrl Pts',(-2.60266268502766,-2.80752084211434,
42.));
#33460=CARTESIAN_POINT('Ctrl Pts',(-2.56563543615746,-2.84794928527981,
42.));
#33461=CARTESIAN_POINT('Ctrl Pts',(-2.54453127685218,-2.87099199925564,
42.));
#33462=CARTESIAN_POINT('Ctrl Pts',(-2.52314012955761,-2.89379293748534,
42.));
#33463=CARTESIAN_POINT('Ctrl Pts',(-2.50149137216201,-2.91631875583217,
42.));
#33464=CARTESIAN_POINT('Ctrl Pts',(-2.41601150820879,-3.00526168463577,
42.));
#33465=CARTESIAN_POINT('Ctrl Pts',(-2.32646440639479,-3.08998053490754,
42.));
#33466=CARTESIAN_POINT('Ctrl Pts',(-2.23310493987845,-3.17012015379869,
42.));
#33467=CARTESIAN_POINT('Ctrl Pts',(-2.14095799804003,-3.24921894341766,
42.));
#33468=CARTESIAN_POINT('Ctrl Pts',(-2.04509659589572,-3.32385743023979,
42.));
#33469=CARTESIAN_POINT('Ctrl Pts',(-1.94572314910561,-3.39366789682963,
42.));
#33470=CARTESIAN_POINT('Ctrl Pts',(-1.88149925545439,-3.43878558296039,
42.));
#33471=CARTESIAN_POINT('Ctrl Pts',(-1.81580757706967,-3.48188610285196,
42.));
#33472=CARTESIAN_POINT('Ctrl Pts',(-1.7486944753309,-3.52286199445098,42.));
#33473=CARTESIAN_POINT('Ctrl Pts',(-1.83231942908391,2.65117390457541,42.));
#33474=CARTESIAN_POINT('Ctrl Pts',(-1.84571201009948,2.64191782131431,42.0005355599176));
#33475=CARTESIAN_POINT('Ctrl Pts',(-1.85903445318218,2.6325602558508,42.0010711198351));
#33476=CARTESIAN_POINT('Ctrl Pts',(-1.8722852285359,2.62310228270006,42.0016066797527));
#33477=CARTESIAN_POINT('Ctrl Pts',(-1.75279757044496,-3.52836060600329,
7.));
#33478=CARTESIAN_POINT('Ctrl Pts',(-1.82143513113133,-3.4868125032314,6.99999999999999));
#33479=CARTESIAN_POINT('Ctrl Pts',(-1.88858118174007,-3.44308259126114,
6.99999999999999));
#33480=CARTESIAN_POINT('Ctrl Pts',(-1.95412266298839,-3.39717065740713,
6.99999999999999));
#33481=CARTESIAN_POINT('Ctrl Pts',(-2.05256253282086,-3.32821333898428,
6.99999999999999));
#33482=CARTESIAN_POINT('Ctrl Pts',(-2.14738467987841,-3.25433542296032,
7.));
#33483=CARTESIAN_POINT('Ctrl Pts',(-2.23843373886498,-3.17595281845062,
7.));
#33484=CARTESIAN_POINT('Ctrl Pts',(-2.33061677527292,-3.09659399183901,
7.));
#33485=CARTESIAN_POINT('Ctrl Pts',(-2.41893259169034,-3.01261674070712,
6.99999999999999));
#33486=CARTESIAN_POINT('Ctrl Pts',(-2.50317815019085,-2.9244189608764,6.99999999999999));
#33487=CARTESIAN_POINT('Ctrl Pts',(-2.5873331199782,-2.8363160195573,7.));
#33488=CARTESIAN_POINT('Ctrl Pts',(-2.66742692977287,-2.74400072916138,
6.99999999999999));
#33489=CARTESIAN_POINT('Ctrl Pts',(-2.74320996257998,-2.64784930966859,
6.99999999999999));
#33490=CARTESIAN_POINT('Ctrl Pts',(-2.77126696959633,-2.61225135388067,
6.99999999999999));
#33491=CARTESIAN_POINT('Ctrl Pts',(-2.79873261100939,-2.57612745058929,
7.));
#33492=CARTESIAN_POINT('Ctrl Pts',(-2.82559242679685,-2.53949635630442,
7.));
#33493=CARTESIAN_POINT('Ctrl Pts',(-2.83828837203979,-2.52218177861299,
7.));
#33494=CARTESIAN_POINT('Ctrl Pts',(-2.85085104477547,-2.5047507777665,7.));
#33495=CARTESIAN_POINT('Ctrl Pts',(-2.86326365819409,-2.48722719727718,
7.));
#33496=CARTESIAN_POINT('Ctrl Pts',(-2.93259158933157,-2.38935308000032,
7.));
#33497=CARTESIAN_POINT('Ctrl Pts',(-2.99733701215284,-2.28846693884865,
7.));
#33498=CARTESIAN_POINT('Ctrl Pts',(-3.05733419775333,-2.18496288465553,
7.));
#33499=CARTESIAN_POINT('Ctrl Pts',(-3.11720514852066,-2.08167660429433,
7.));
#33500=CARTESIAN_POINT('Ctrl Pts',(-3.17234812152713,-1.97578252307709,
7.));
#33501=CARTESIAN_POINT('Ctrl Pts',(-3.22255056777115,-1.86765274479227,
7.));
#33502=CARTESIAN_POINT('Ctrl Pts',(-3.27167565899372,-1.76184345421906,
7.));
#33503=CARTESIAN_POINT('Ctrl Pts',(-3.31607011161638,-1.65389257738756,
7.));
#33504=CARTESIAN_POINT('Ctrl Pts',(-3.35548609359103,-1.54414270697495,
7.));
#33505=CARTESIAN_POINT('Ctrl Pts',(-3.38624690686046,-1.45849229054546,
7.));
#33506=CARTESIAN_POINT('Ctrl Pts',(-3.41397468395636,-1.37174597137287,
7.00000000000001));
#33507=CARTESIAN_POINT('Ctrl Pts',(-3.43852956617388,-1.28406860130853,
7.00000000000001));
#33508=CARTESIAN_POINT('Ctrl Pts',(-3.44534001315227,-1.25975074570902,
7.00000000000001));
#33509=CARTESIAN_POINT('Ctrl Pts',(-3.45190626155755,-1.23536129061186,
7.));
#33510=CARTESIAN_POINT('Ctrl Pts',(-3.45822504922081,-1.21090381613226,
7.));
#33511=CARTESIAN_POINT('Ctrl Pts',(-3.46235658517791,-1.19491230943548,
7.00000000000001));
#33512=CARTESIAN_POINT('Ctrl Pts',(-3.46638018579831,-1.17889993609237,
7.));
#33513=CARTESIAN_POINT('Ctrl Pts',(-3.4702944287354,-1.16287131443645,7.));
#33514=CARTESIAN_POINT('Ctrl Pts',(-3.49751037118451,-1.0514234427693,7.00000000000001));
#33515=CARTESIAN_POINT('Ctrl Pts',(-3.51945812556307,-0.939134270268195,
7.00000000000001));
#33516=CARTESIAN_POINT('Ctrl Pts',(-3.53594432284242,-0.826340673701463,
7.00000000000001));
#33517=CARTESIAN_POINT('Ctrl Pts',(-3.55198795134533,-0.716574999412837,
7.00000000000001));
#33518=CARTESIAN_POINT('Ctrl Pts',(-3.56285932263424,-0.60633091546549,
7.00000000000001));
#33519=CARTESIAN_POINT('Ctrl Pts',(-3.56833195426463,-0.495920182767021,
7.00000000000001));
#33520=CARTESIAN_POINT('Ctrl Pts',(-3.57365992657054,-0.388427962237084,
7.));
#33521=CARTESIAN_POINT('Ctrl Pts',(-3.57387078895861,-0.280777228268469,
7.00000000000001));
#33522=CARTESIAN_POINT('Ctrl Pts',(-3.56870919579919,-0.173266018235025,
7.00000000000001));
#33523=CARTESIAN_POINT('Ctrl Pts',(-3.56545218869441,-0.105425573607107,
7.00000000000001));
#33524=CARTESIAN_POINT('Ctrl Pts',(-3.56005490071492,-0.0376409163409465,
7.00000000000001));
#33525=CARTESIAN_POINT('Ctrl Pts',(-3.55255422030096,0.0300081250946052,
7.00000000000001));
#33526=CARTESIAN_POINT('Ctrl Pts',(-3.54883684376604,0.0635353446751962,
7.00000000000001));
#33527=CARTESIAN_POINT('Ctrl Pts',(-3.54460273875139,0.0970292015076146,
7.00000000000001));
#33528=CARTESIAN_POINT('Ctrl Pts',(-3.53985592740968,0.130479635249894,
7.00000000000001));
#33529=CARTESIAN_POINT('Ctrl Pts',(-3.53595669558841,0.157957237853769,
7.00000000000001));
#33530=CARTESIAN_POINT('Ctrl Pts',(-3.53171002969387,0.185413044431481,
7.00000000000001));
#33531=CARTESIAN_POINT('Ctrl Pts',(-3.52712663472941,0.212793679985835,
7.00000000000001));
#33532=CARTESIAN_POINT('Ctrl Pts',(-3.50874228151889,0.322619535942592,
7.00000000000001));
#33533=CARTESIAN_POINT('Ctrl Pts',(-3.48492824893386,0.431373726643265,
7.00000000000001));
#33534=CARTESIAN_POINT('Ctrl Pts',(-3.45593528714537,0.538732382687488,
7.00000000000001));
#33535=CARTESIAN_POINT('Ctrl Pts',(-3.42668728127143,0.647035446910703,
7.00000000000001));
#33536=CARTESIAN_POINT('Ctrl Pts',(-3.3921683075505,0.753919111921691,7.00000000000001));
#33537=CARTESIAN_POINT('Ctrl Pts',(-3.35258661736185,0.859029856172523,
7.00000000000001));
#33538=CARTESIAN_POINT('Ctrl Pts',(-3.31330346367511,0.96334782493164,7.00000000000001));
#33539=CARTESIAN_POINT('Ctrl Pts',(-3.26903306106834,1.06592021272638,7.00000000000001));
#33540=CARTESIAN_POINT('Ctrl Pts',(-3.21993945256717,1.16636974039666,7.00000000000001));
#33541=CARTESIAN_POINT('Ctrl Pts',(-3.18444216307314,1.23900009029579,7.00000000000001));
#33542=CARTESIAN_POINT('Ctrl Pts',(-3.14642243000112,1.31051997303733,7.00000000000001));
#33543=CARTESIAN_POINT('Ctrl Pts',(-3.10593191142431,1.38077323634485,7.00000000000001));
#33544=CARTESIAN_POINT('Ctrl Pts',(-3.09665163218864,1.39687502816246,7.00000000000001));
#33545=CARTESIAN_POINT('Ctrl Pts',(-3.087240740324,1.41291154782213,7.00000000000001));
#33546=CARTESIAN_POINT('Ctrl Pts',(-3.07770226318236,1.42887670683733,7.00000000000001));
#33547=CARTESIAN_POINT('Ctrl Pts',(-3.02120417669121,1.52344116628832,7.00000000000001));
#33548=CARTESIAN_POINT('Ctrl Pts',(-2.96039292042869,1.61523884970404,7.00000000000001));
#33549=CARTESIAN_POINT('Ctrl Pts',(-2.89545383187046,1.70392058416469,7.00000000000001));
#33550=CARTESIAN_POINT('Ctrl Pts',(-2.83177573858355,1.7908802857128,7.00000000000001));
#33551=CARTESIAN_POINT('Ctrl Pts',(-2.76412793568667,1.8748443953877,7.00000000000001));
#33552=CARTESIAN_POINT('Ctrl Pts',(-2.69265479824662,1.95544467162499,7.00000000000001));
#33553=CARTESIAN_POINT('Ctrl Pts',(-2.64648561361655,2.00750967350008,7.00000000000001));
#33554=CARTESIAN_POINT('Ctrl Pts',(-2.5987196386097,2.05817023396695,7.));
#33555=CARTESIAN_POINT('Ctrl Pts',(-2.54939063956779,2.10731665555531,7.00000000000001));
#33556=CARTESIAN_POINT('Ctrl Pts',(-2.5348701644819,2.12178338717555,7.00000000000001));
#33557=CARTESIAN_POINT('Ctrl Pts',(-2.52021953276182,2.13611352242801,7.));
#33558=CARTESIAN_POINT('Ctrl Pts',(-2.50544499954275,2.15029964147411,7.));
#33559=CARTESIAN_POINT('Ctrl Pts',(-2.42926702549359,2.22344373290008,7.));
#33560=CARTESIAN_POINT('Ctrl Pts',(-2.34975484372937,2.29280507614037,7.));
#33561=CARTESIAN_POINT('Ctrl Pts',(-2.26705259277626,2.35803725076561,7.));
#33562=CARTESIAN_POINT('Ctrl Pts',(-2.18660206795646,2.42149335532451,7.));
#33563=CARTESIAN_POINT('Ctrl Pts',(-2.10313227547012,2.48104239546345,7.));
#33564=CARTESIAN_POINT('Ctrl Pts',(-2.01675688329826,2.5363204381136,7.));
#33565=CARTESIAN_POINT('Ctrl Pts',(-1.96924061746609,2.56672963340872,7.));
#33566=CARTESIAN_POINT('Ctrl Pts',(-1.92084475461694,2.59584549215854,7.));
#33567=CARTESIAN_POINT('Ctrl Pts',(-1.87158653173904,2.62360084935059,7.));
#33568=CARTESIAN_POINT('Origin',(0.,0.,42.));
#33569=CARTESIAN_POINT('Origin',(0.,0.,7.));
#33570=CARTESIAN_POINT('',(0.,0.,0.));
#33571=CARTESIAN_POINT('Origin',(0.,-4.0019382647053,0.));
#33572=CARTESIAN_POINT('',(0.,-4.0019382647053,9.1643052178268));
#33573=CARTESIAN_POINT('Origin',(0.,-4.0019382647053,0.));
#33574=CARTESIAN_POINT('Origin',(0.,0.,0.));
#33575=CARTESIAN_POINT('',(0.,0.,0.));
#33576=CARTESIAN_POINT('Origin',(0.,0.,32.));
#33577=CARTESIAN_POINT('',(4.,4.89858719658941E-16,29.));
#33578=CARTESIAN_POINT('Origin',(0.,0.,29.));
#33579=CARTESIAN_POINT('',(4.,-4.89858719658941E-16,35.));
#33580=CARTESIAN_POINT('',(4.,4.89858719658941E-16,32.));
#33581=CARTESIAN_POINT('Origin',(0.,0.,35.));
#33582=CARTESIAN_POINT('Origin',(0.,0.,35.));
#33583=CARTESIAN_POINT('',(-3.46410161513776,-6.,35.));
#33584=CARTESIAN_POINT('',(3.46410161513775,-6.,35.));
#33585=CARTESIAN_POINT('',(-3.46410161513776,-6.,35.));
#33586=CARTESIAN_POINT('',(6.92820323027551,-2.22044604925031E-15,35.));
#33587=CARTESIAN_POINT('',(3.46410161513775,-6.,35.));
#33588=CARTESIAN_POINT('',(3.46410161513776,6.,35.));
#33589=CARTESIAN_POINT('',(6.92820323027551,-2.22044604925031E-15,35.));
#33590=CARTESIAN_POINT('',(-3.46410161513775,6.,35.));
#33591=CARTESIAN_POINT('',(3.46410161513776,6.,35.));
#33592=CARTESIAN_POINT('',(-6.92820323027551,4.44089209850063E-15,35.));
#33593=CARTESIAN_POINT('',(-3.46410161513775,6.,35.));
#33594=CARTESIAN_POINT('',(-6.92820323027551,3.88578058618805E-15,35.));
#33595=CARTESIAN_POINT('Origin',(6.92820323027551,-2.22044604925031E-15,
32.));
#33596=CARTESIAN_POINT('',(3.46410161513775,-6.,29.));
#33597=CARTESIAN_POINT('',(3.46410161513775,-6.,32.));
#33598=CARTESIAN_POINT('',(6.92820323027551,-2.22044604925031E-15,29.));
#33599=CARTESIAN_POINT('',(3.46410161513775,-6.,29.));
#33600=CARTESIAN_POINT('',(6.92820323027551,-2.22044604925031E-15,32.));
#33601=CARTESIAN_POINT('Origin',(3.46410161513776,6.,32.));
#33602=CARTESIAN_POINT('',(3.46410161513776,6.,29.));
#33603=CARTESIAN_POINT('',(6.92820323027551,-2.22044604925031E-15,29.));
#33604=CARTESIAN_POINT('',(3.46410161513776,6.,32.));
#33605=CARTESIAN_POINT('Origin',(-3.46410161513775,6.,32.));
#33606=CARTESIAN_POINT('',(-3.46410161513775,6.,29.));
#33607=CARTESIAN_POINT('',(3.46410161513776,6.,29.));
#33608=CARTESIAN_POINT('',(-3.46410161513775,6.,32.));
#33609=CARTESIAN_POINT('Origin',(-6.92820323027551,4.44089209850063E-15,
32.));
#33610=CARTESIAN_POINT('',(-6.92820323027551,4.44089209850063E-15,29.));
#33611=CARTESIAN_POINT('',(-3.46410161513775,6.,29.));
#33612=CARTESIAN_POINT('',(-6.92820323027551,3.88578058618805E-15,32.));
#33613=CARTESIAN_POINT('Origin',(-3.46410161513776,-6.,32.));
#33614=CARTESIAN_POINT('',(-3.46410161513776,-6.,29.));
#33615=CARTESIAN_POINT('',(-6.92820323027551,3.88578058618805E-15,29.));
#33616=CARTESIAN_POINT('',(-3.46410161513776,-6.,32.));
#33617=CARTESIAN_POINT('Origin',(3.46410161513775,-6.,32.));
#33618=CARTESIAN_POINT('',(-3.46410161513776,-6.,29.));
#33619=CARTESIAN_POINT('Origin',(0.,0.,29.));
#33620=CARTESIAN_POINT('',(0.,0.,0.));
#33621=CARTESIAN_POINT('Origin',(0.,0.,32.));
#33622=CARTESIAN_POINT('',(3.93496388660084,0.00195648875352047,37.2208358380349));
#33623=CARTESIAN_POINT('',(3.93463686453598,0.00228919349351085,37.4041629160656));
#33624=CARTESIAN_POINT('',(3.933,4.81653586104654E-16,32.));
#33625=CARTESIAN_POINT('',(-3.88542223618671,0.609904128979188,37.9980892280756));
#33626=CARTESIAN_POINT('Ctrl Pts',(-3.88542223618671,0.609904128979188,
37.9980892280756));
#33627=CARTESIAN_POINT('Ctrl Pts',(-3.86749256473595,0.724125923573192,
37.9922268209659));
#33628=CARTESIAN_POINT('Ctrl Pts',(-3.84449896610055,0.837702284267991,
37.9863644138562));
#33629=CARTESIAN_POINT('Ctrl Pts',(-3.81650392804124,0.950150918141841,
37.9805020067465));
#33630=CARTESIAN_POINT('Ctrl Pts',(-3.78853529915897,1.06249347336439,37.9746451299506));
#33631=CARTESIAN_POINT('Ctrl Pts',(-3.75557471545758,1.17371001885672,37.9687882531547));
#33632=CARTESIAN_POINT('Ctrl Pts',(-3.71773598028384,1.28332699687297,37.9629313763589));
#33633=CARTESIAN_POINT('Ctrl Pts',(-3.67990854063047,1.39291125231526,37.9570762479426));
#33634=CARTESIAN_POINT('Ctrl Pts',(-3.6372059613303,1.5008964937652,37.9512211195263));
#33635=CARTESIAN_POINT('Ctrl Pts',(-3.58979229255919,1.60682304448332,37.94536599111));
#33636=CARTESIAN_POINT('Ctrl Pts',(-3.54240969388923,1.71268018170253,37.93951469955));
#33637=CARTESIAN_POINT('Ctrl Pts',(-3.49032233155603,1.81648094151968,37.9336634079899));
#33638=CARTESIAN_POINT('Ctrl Pts',(-3.43374231814287,1.91778588288548,37.9278121164299));
#33639=CARTESIAN_POINT('Ctrl Pts',(-3.37716709289371,2.01908225117672,37.9219613200437));
#33640=CARTESIAN_POINT('Ctrl Pts',(-3.31610017418119,2.11788286012534,37.9161105236576));
#33641=CARTESIAN_POINT('Ctrl Pts',(-3.25079938729001,2.21377332705832,37.9102597272714));
#33642=CARTESIAN_POINT('Ctrl Pts',(-3.18548831005988,2.3096789047649,37.9044080088952));
#33643=CARTESIAN_POINT('Ctrl Pts',(-3.11594227087696,2.40267308700958,37.8985562905189));
#33644=CARTESIAN_POINT('Ctrl Pts',(-3.04246171385679,2.4923715051564,37.8927045721426));
#33645=CARTESIAN_POINT('Ctrl Pts',(-2.9689019872486,2.58216656637588,37.8868465489947));
#33646=CARTESIAN_POINT('Ctrl Pts',(-2.89139953671942,2.66865844926548,37.8809885258468));
#33647=CARTESIAN_POINT('Ctrl Pts',(-2.81029448477806,2.75149666705704,37.8751305026989));
#33648=CARTESIAN_POINT('Ctrl Pts',(-2.72914963764217,2.83437553044236,37.8692696052397));
#33649=CARTESIAN_POINT('Ctrl Pts',(-2.6443989705447,2.91359687583261,37.8634087077804));
#33650=CARTESIAN_POINT('Ctrl Pts',(-2.55641735766959,2.98884915869062,37.8575478103212));
#33651=CARTESIAN_POINT('Ctrl Pts',(-2.46828756305929,3.06422818409729,37.8516770417317));
#33652=CARTESIAN_POINT('Ctrl Pts',(-2.37691627453245,3.13562453343064,37.8458062731423));
#33653=CARTESIAN_POINT('Ctrl Pts',(-2.28270965334754,3.20276843348281,37.8399355045529));
#33654=CARTESIAN_POINT('Ctrl Pts',(-2.18895820069543,3.26958792119445,37.8340931011578));
#33655=CARTESIAN_POINT('Ctrl Pts',(-2.0923991372675,3.33219581956083,37.8282506977628));
#33656=CARTESIAN_POINT('Ctrl Pts',(-1.99345630322199,3.39037180367353,37.8224082943678));
#33657=CARTESIAN_POINT('Ctrl Pts',(-1.89401014270797,3.44884373152909,37.8165361704145));
#33658=CARTESIAN_POINT('Ctrl Pts',(-1.79182243863938,3.5030345546936,37.8106640464611));
#33659=CARTESIAN_POINT('Ctrl Pts',(-1.68729798416966,3.55267709095789,37.8047919225078));
#33660=CARTESIAN_POINT('Ctrl Pts',(-1.58290904772492,3.60225526469091,37.7989274118794));
#33661=CARTESIAN_POINT('Ctrl Pts',(-1.47618975572388,3.64729670268684,37.7930629012511));
#33662=CARTESIAN_POINT('Ctrl Pts',(-1.36757205913616,3.68757856364716,37.7871983906227));
#33663=CARTESIAN_POINT('Ctrl Pts',(-1.25906612907142,3.72781897497561,37.7813399145171));
#33664=CARTESIAN_POINT('Ctrl Pts',(-1.14866606518523,3.76330940785714,37.7754814384116));
#33665=CARTESIAN_POINT('Ctrl Pts',(-1.03682588890287,3.79387415132616,37.769622962306));
#33666=CARTESIAN_POINT('Ctrl Pts',(-0.920575705995505,3.82564410320659,
37.7635334787101));
#33667=CARTESIAN_POINT('Ctrl Pts',(-0.802769914156219,3.85209172586888,
37.7574439951142));
#33668=CARTESIAN_POINT('Ctrl Pts',(-0.683938671629199,3.87307589564807,
37.7513545115183));
#33669=CARTESIAN_POINT('Ctrl Pts',(-0.569747881856857,3.89324061722167,
37.7455028270089));
#33670=CARTESIAN_POINT('Ctrl Pts',(-0.454610673238864,3.90836050408855,
37.7396511424996));
#33671=CARTESIAN_POINT('Ctrl Pts',(-0.339009367189833,3.91836211304641,
37.7337994579902));
#33672=CARTESIAN_POINT('Ctrl Pts',(-0.223425692845461,3.92836219654214,
37.7279486659896));
#33673=CARTESIAN_POINT('Ctrl Pts',(-0.107378473573039,3.93324551867752,
37.722097873989));
#33674=CARTESIAN_POINT('Ctrl Pts',(0.00864472130136986,3.93299049945377,
37.7162470819884));
#33675=CARTESIAN_POINT('Ctrl Pts',(0.124678322130959,3.93273545735771,37.7103957652385));
#33676=CARTESIAN_POINT('Ctrl Pts',(0.240687480842907,3.92734115868281,37.7045444484887));
#33677=CARTESIAN_POINT('Ctrl Pts',(0.356185216416442,3.91683814978439,37.6986931317389));
#33678=CARTESIAN_POINT('Ctrl Pts',(0.471721285545492,3.90633165495031,37.6928398729442));
#33679=CARTESIAN_POINT('Ctrl Pts',(0.586745182521605,3.89071311577341,37.6869866141496));
#33680=CARTESIAN_POINT('Ctrl Pts',(0.700776341940978,3.8700647951392,37.681133355355));
#33681=CARTESIAN_POINT('Ctrl Pts',(0.814937234059428,3.84939298301038,37.6752734373361));
#33682=CARTESIAN_POINT('Ctrl Pts',(0.928102727263295,3.82368004145438,37.6694135193173));
#33683=CARTESIAN_POINT('Ctrl Pts',(1.03980362436862,3.79305911142311,37.6635536012984));
#33684=CARTESIAN_POINT('Ctrl Pts',(1.15157973289195,3.76241756344134,37.6576897376286));
#33685=CARTESIAN_POINT('Ctrl Pts',(1.2618888891731,3.72686157322117,37.6518258739589));
#33686=CARTESIAN_POINT('Ctrl Pts',(1.37027986241766,3.68657321894637,37.6459620102891));
#33687=CARTESIAN_POINT('Ctrl Pts',(1.47883073841939,3.64622542965834,37.64008949601));
#33688=CARTESIAN_POINT('Ctrl Pts',(1.5854574043302,3.6011315032136,37.6342169817309));
#33689=CARTESIAN_POINT('Ctrl Pts',(1.68973121106261,3.55152043980615,37.6283444674517));
#33690=CARTESIAN_POINT('Ctrl Pts',(1.7185502575496,3.53780900462016,37.6267214303026));
#33691=CARTESIAN_POINT('Ctrl Pts',(1.74718974257687,3.52375278791357,37.6250983931535));
#33692=CARTESIAN_POINT('Ctrl Pts',(1.7756410032213,3.50935721004278,37.6234753560044));
#33693=CARTESIAN_POINT('Ctrl Pts',(1.87857723493968,3.45727422651714,37.6176032320885));
#33694=CARTESIAN_POINT('Ctrl Pts',(1.97939255308003,3.40057110844653,37.6117311081726));
#33695=CARTESIAN_POINT('Ctrl Pts',(2.07764341029815,3.33944409440324,37.6058589842567));
#33696=CARTESIAN_POINT('Ctrl Pts',(2.17576688331402,3.27839633275672,37.5999944736669));
#33697=CARTESIAN_POINT('Ctrl Pts',(2.27133215960027,3.21293629767389,37.5941299630771));
#33698=CARTESIAN_POINT('Ctrl Pts',(2.36391832744339,3.14330703896028,37.5882654524874));
#33699=CARTESIAN_POINT('Ctrl Pts',(2.45640922502803,3.07374942807084,37.5824069764215));
#33700=CARTESIAN_POINT('Ctrl Pts',(2.54592678312613,3.00003137372826,37.5765485003556));
#33701=CARTESIAN_POINT('Ctrl Pts',(2.63207782173528,2.92243996351152,37.5706900242897));
#33702=CARTESIAN_POINT('Ctrl Pts',(2.72162591098664,2.84178902024491,37.5646005406793));
#33703=CARTESIAN_POINT('Ctrl Pts',(2.8075361396623,2.75695321399475,37.5585110570689));
#33704=CARTESIAN_POINT('Ctrl Pts',(2.88940329059112,2.66830238622259,37.5524215734586));
#33705=CARTESIAN_POINT('Ctrl Pts',(2.96807346463353,2.583113443274,37.5465698889915));
#33706=CARTESIAN_POINT('Ctrl Pts',(3.0430100991615,2.49440217895448,37.5407182045244));
#33707=CARTESIAN_POINT('Ctrl Pts',(3.11389077470868,2.4025347537932,37.5348665200573));
#33708=CARTESIAN_POINT('Ctrl Pts',(3.18476063940591,2.31068134041921,37.5290157280998));
#33709=CARTESIAN_POINT('Ctrl Pts',(3.25157552266725,2.21567305056715,37.5231649361423));
#33710=CARTESIAN_POINT('Ctrl Pts',(3.31405380919675,2.11790848474349,37.5173141441848));
#33711=CARTESIAN_POINT('Ctrl Pts',(3.3765376993061,2.02013515056877,37.5114628274789));
#33712=CARTESIAN_POINT('Ctrl Pts',(3.43468399686684,1.91960539737308,37.505611510773));
#33713=CARTESIAN_POINT('Ctrl Pts',(3.48825526576596,1.81674549699621,37.4997601940671));
#33714=CARTESIAN_POINT('Ctrl Pts',(3.54184431489582,1.71385145755939,37.4939069353172));
#33715=CARTESIAN_POINT('Ctrl Pts',(3.59085512516964,1.60862609961033,37.4880536765674));
#33716=CARTESIAN_POINT('Ctrl Pts',(3.63509724358918,1.501518241531,37.4822004178175));
#33717=CARTESIAN_POINT('Ctrl Pts',(3.67938969604625,1.39428852737559,37.4763404998443));
#33718=CARTESIAN_POINT('Ctrl Pts',(3.71890246993564,1.28517242061843,37.4704805818711));
#33719=CARTESIAN_POINT('Ctrl Pts',(3.75349406598325,1.17463666579437,37.464620663898));
#33720=CARTESIAN_POINT('Ctrl Pts',(3.78810895354121,1.06402648408717,37.4587568002745));
#33721=CARTESIAN_POINT('Ctrl Pts',(3.81779595965542,0.951995149594837,37.4528929366511));
#33722=CARTESIAN_POINT('Ctrl Pts',(3.84246447098273,0.839020732303683,37.4470290730277));
#33723=CARTESIAN_POINT('Ctrl Pts',(3.86716937429586,0.725879650581997,37.4411565587954));
#33724=CARTESIAN_POINT('Ctrl Pts',(3.88684093685391,0.611793115212634,37.4352840445631));
#33725=CARTESIAN_POINT('Ctrl Pts',(3.90144022942924,0.497245549191858,37.4294115303309));
#33726=CARTESIAN_POINT('Ctrl Pts',(3.9054751622212,0.465587047384892,37.4277884927676));
#33727=CARTESIAN_POINT('Ctrl Pts',(3.90912295559818,0.433893334164532,37.4261654552043));
#33728=CARTESIAN_POINT('Ctrl Pts',(3.9123834894837,0.402174627761775,37.424542417641));
#33729=CARTESIAN_POINT('Ctrl Pts',(3.92602993472042,0.269421034300653,37.417749452439));
#33730=CARTESIAN_POINT('Ctrl Pts',(3.93292115709448,0.135961246390276,37.410956487237));
#33731=CARTESIAN_POINT('Ctrl Pts',(3.93299932738369,0.00230017378215415,
37.404163522035));
#33732=CARTESIAN_POINT('',(-2.80846544028688,-2.75336355585568,38.));
#33733=CARTESIAN_POINT('Origin',(0.,0.,38.));
#33734=CARTESIAN_POINT('Ctrl Pts',(3.93299950757024,0.00196810879246953,
37.220836477965));
#33735=CARTESIAN_POINT('Ctrl Pts',(3.93294383452817,0.113223161314397,37.2264931957242));
#33736=CARTESIAN_POINT('Ctrl Pts',(3.92816790717577,0.22435667800964,37.2321499134834));
#33737=CARTESIAN_POINT('Ctrl Pts',(3.91869980905131,0.335083282992792,37.2378066312426));
#33738=CARTESIAN_POINT('Ctrl Pts',(3.90887116844884,0.450026325534738,37.2436787552018));
#33739=CARTESIAN_POINT('Ctrl Pts',(3.89396450975248,0.564729262387047,37.249550879161));
#33740=CARTESIAN_POINT('Ctrl Pts',(3.87399604281211,0.678707345087798,37.2554230031202));
#33741=CARTESIAN_POINT('Ctrl Pts',(3.85405346538562,0.79253765294116,37.261287513754));
#33742=CARTESIAN_POINT('Ctrl Pts',(3.82906220129585,0.905644572093272,37.2671520243879));
#33743=CARTESIAN_POINT('Ctrl Pts',(3.79909033948502,1.01754685023913,37.2730165350218));
#33744=CARTESIAN_POINT('Ctrl Pts',(3.76914931842163,1.12933398205476,37.2788750111326));
#33745=CARTESIAN_POINT('Ctrl Pts',(3.73423799979103,1.23991854148262,37.2847334872434));
#33746=CARTESIAN_POINT('Ctrl Pts',(3.69447568419538,1.34882853576318,37.2905919633542));
#33747=CARTESIAN_POINT('Ctrl Pts',(3.65314548775988,1.46203299556326,37.296681446948));
#33748=CARTESIAN_POINT('Ctrl Pts',(3.6065739399445,1.57342766445927,37.3027709305419));
#33749=CARTESIAN_POINT('Ctrl Pts',(3.55495259639291,1.6824984509352,37.3088604141357));
#33750=CARTESIAN_POINT('Ctrl Pts',(3.50534710653775,1.78730993819564,37.3147120986494));
#33751=CARTESIAN_POINT('Ctrl Pts',(3.45107901028721,1.88997522706534,37.3205637831631));
#33752=CARTESIAN_POINT('Ctrl Pts',(3.392367399822,1.99005839729012,37.3264154676768));
#33753=CARTESIAN_POINT('Ctrl Pts',(3.33366474415319,2.09012630265662,37.3322662596814));
#33754=CARTESIAN_POINT('Ctrl Pts',(3.27052013093913,2.1876125159477,37.338117051686));
#33755=CARTESIAN_POINT('Ctrl Pts',(3.20319799362034,2.28210683660223,37.3439678436907));
#33756=CARTESIAN_POINT('Ctrl Pts',(3.13586981827867,2.37660963231256,37.3498191604442));
#33757=CARTESIAN_POINT('Ctrl Pts',(3.06436361390616,2.46811966523383,37.3556704771977));
#33758=CARTESIAN_POINT('Ctrl Pts',(2.98898599387445,2.55625736740696,37.3615217939512));
#33759=CARTESIAN_POINT('Ctrl Pts',(2.91358335610828,2.64442432236928,37.3673750527492));
#33760=CARTESIAN_POINT('Ctrl Pts',(2.83430701626353,2.72921640696602,37.3732283115471));
#33761=CARTESIAN_POINT('Ctrl Pts',(2.75150206251009,2.81028920220014,37.3790815703451));
#33762=CARTESIAN_POINT('Ctrl Pts',(2.66860290196837,2.89145423355433,37.3849414883668));
#33763=CARTESIAN_POINT('Ctrl Pts',(2.58216741028541,2.96889124035578,37.3908014063884));
#33764=CARTESIAN_POINT('Ctrl Pts',(2.49257560162771,3.04229450746805,37.3966613244101));
#33765=CARTESIAN_POINT('Ctrl Pts',(2.4029234682402,3.11574719910163,37.4025251880824));
#33766=CARTESIAN_POINT('Ctrl Pts',(2.31011111636953,3.18516049589827,37.4083890517546));
#33767=CARTESIAN_POINT('Ctrl Pts',(2.21454808627185,3.25027164612278,37.4142529154269));
#33768=CARTESIAN_POINT('Ctrl Pts',(2.11884407772622,3.31547885095014,37.4201254297081));
#33769=CARTESIAN_POINT('Ctrl Pts',(2.02038164240613,3.37637102573865,37.4259979439892));
#33770=CARTESIAN_POINT('Ctrl Pts',(1.91959553306117,3.4327309812235,37.4318704582704));
#33771=CARTESIAN_POINT('Ctrl Pts',(1.89174041207018,3.44830766524553,37.4334934953822));
#33772=CARTESIAN_POINT('Ctrl Pts',(1.86370791579227,3.46353843799419,37.4351165324941));
#33773=CARTESIAN_POINT('Ctrl Pts',(1.83550747679674,3.47841936842343,37.4367395696059));
#33774=CARTESIAN_POINT('Ctrl Pts',(1.73347871087051,3.53225835184389,37.4426116935682));
#33775=CARTESIAN_POINT('Ctrl Pts',(1.62890808433844,3.5816947379408,37.4484838175304));
#33776=CARTESIAN_POINT('Ctrl Pts',(1.52221224378136,3.62648023362628,37.4543559414927));
#33777=CARTESIAN_POINT('Ctrl Pts',(1.41565473650146,3.67120766402677,37.4602204521296));
#33778=CARTESIAN_POINT('Ctrl Pts',(1.30697787232185,3.71129603691539,37.4660849627664));
#33779=CARTESIAN_POINT('Ctrl Pts',(1.19662338876077,3.74654260158225,37.4719494734033));
#33780=CARTESIAN_POINT('Ctrl Pts',(1.0863824588669,3.78175289788424,37.477807949517));
#33781=CARTESIAN_POINT('Ctrl Pts',(0.974467734634347,3.81213117071812,37.4836664256307));
#33782=CARTESIAN_POINT('Ctrl Pts',(0.861340834317039,3.83752276438043,37.4895249017444));
#33783=CARTESIAN_POINT('Ctrl Pts',(0.743753190362223,3.86391558223926,37.4956143853371));
#33784=CARTESIAN_POINT('Ctrl Pts',(0.624856227806823,3.88492019147547,37.5017038689298));
#33785=CARTESIAN_POINT('Ctrl Pts',(0.505186031405749,3.90041998683123,37.5077933525225));
#33786=CARTESIAN_POINT('Ctrl Pts',(0.390189049364761,3.91531450310821,37.5136450370389));
#33787=CARTESIAN_POINT('Ctrl Pts',(0.274478539588281,3.92512601396187,37.5194967215552));
#33788=CARTESIAN_POINT('Ctrl Pts',(0.158539689569357,3.9298033241921,37.5253484060716));
#33789=CARTESIAN_POINT('Ctrl Pts',(0.0426185227462051,3.9344799210308,37.5311991980788));
#33790=CARTESIAN_POINT('Ctrl Pts',(-0.0735305021100036,3.93402385758884,
37.537049990086));
#33791=CARTESIAN_POINT('Ctrl Pts',(-0.189419339084341,3.92843598827585,
37.5429007820933));
#33792=CARTESIAN_POINT('Ctrl Pts',(-0.305318569954967,3.92284761779523,
37.5487520988493));
#33793=CARTESIAN_POINT('Ctrl Pts',(-0.420957153596696,3.91212654639289,
37.5546034156052));
#33794=CARTESIAN_POINT('Ctrl Pts',(-0.535850027816559,3.89632567269331,
37.5604547323612));
#33795=CARTESIAN_POINT('Ctrl Pts',(-0.650781034830726,3.88051955470447,
37.5663079911616));
#33796=CARTESIAN_POINT('Ctrl Pts',(-0.76496543094427,3.85963033825317,37.572161249962));
#33797=CARTESIAN_POINT('Ctrl Pts',(-0.877926940000475,3.83376228892995,
37.5780145087623));
#33798=CARTESIAN_POINT('Ctrl Pts',(-0.991016964806267,3.80786480965508,
37.5838744267862));
#33799=CARTESIAN_POINT('Ctrl Pts',(-1.10288092238968,3.77697728386623,37.5897343448101));
#33800=CARTESIAN_POINT('Ctrl Pts',(-1.21305623145749,3.74125427889126,37.595594262834));
#33801=CARTESIAN_POINT('Ctrl Pts',(-1.3233057247134,3.70550722059488,37.6014581265084));
#33802=CARTESIAN_POINT('Ctrl Pts',(-1.43186391914719,3.66491834447394,37.6073219901828));
#33803=CARTESIAN_POINT('Ctrl Pts',(-1.53828843031218,3.61969027751929,37.6131858538572));
#33804=CARTESIAN_POINT('Ctrl Pts',(-1.64486994321869,3.57439548829174,37.6190583681404));
#33805=CARTESIAN_POINT('Ctrl Pts',(-1.74931111907896,3.52444802672684,37.6249308824235));
#33806=CARTESIAN_POINT('Ctrl Pts',(-1.85119428810024,3.47009635423932,37.6308033967067));
#33807=CARTESIAN_POINT('Ctrl Pts',(-1.87935261244782,3.45507471683406,37.6324264337942));
#33808=CARTESIAN_POINT('Ctrl Pts',(-1.90731571692631,3.43971691608275,37.6340494708818));
#33809=CARTESIAN_POINT('Ctrl Pts',(-1.93507519692215,3.42402876481152,37.6356725079694));
#33810=CARTESIAN_POINT('Ctrl Pts',(-2.03550858192254,3.36726926727036,37.6415446319685));
#33811=CARTESIAN_POINT('Ctrl Pts',(-2.13361092601821,3.30599200839285,37.6474167559676));
#33812=CARTESIAN_POINT('Ctrl Pts',(-2.22894817098408,3.24041340743226,37.6532888799667));
#33813=CARTESIAN_POINT('Ctrl Pts',(-2.32416180932104,3.17491983042843,37.6591533906405));
#33814=CARTESIAN_POINT('Ctrl Pts',(-2.41661714034022,3.10513623365194,37.6650179013144));
#33815=CARTESIAN_POINT('Ctrl Pts',(-2.50590486924698,3.03132475764051,37.6708824119883));
#33816=CARTESIAN_POINT('Ctrl Pts',(-2.59510072197035,2.95758923290243,37.6767408881391));
#33817=CARTESIAN_POINT('Ctrl Pts',(-2.6811351390289,2.87983433464965,37.6825993642899));
#33818=CARTESIAN_POINT('Ctrl Pts',(-2.76362855226727,2.79836491992969,37.6884578404407));
#33819=CARTESIAN_POINT('Ctrl Pts',(-2.84937478940238,2.71368305892279,37.6945473240195));
#33820=CARTESIAN_POINT('Ctrl Pts',(-2.93129464984765,2.62498797621149,37.7006368075984));
#33821=CARTESIAN_POINT('Ctrl Pts',(-3.00900034488857,2.53266774853325,37.7067262911772));
#33822=CARTESIAN_POINT('Ctrl Pts',(-3.08367157267096,2.44395269687256,37.7125779757308));
#33823=CARTESIAN_POINT('Ctrl Pts',(-3.15445130019248,2.3518906626465,37.7184296602843));
#33824=CARTESIAN_POINT('Ctrl Pts',(-3.22103427970653,2.25686223969374,37.7242813448378));
#33825=CARTESIAN_POINT('Ctrl Pts',(-3.28760710386799,2.16184831064238,37.7301321368822));
#33826=CARTESIAN_POINT('Ctrl Pts',(-3.3499842155701,2.06386923093621,37.7359829289266));
#33827=CARTESIAN_POINT('Ctrl Pts',(-3.40790261924258,1.96333612449819,37.741833720971));
#33828=CARTESIAN_POINT('Ctrl Pts',(-3.46582621752925,1.86279400139762,37.747685037764));
#33829=CARTESIAN_POINT('Ctrl Pts',(-3.51929010644619,1.75969775444043,37.7535363545571));
#33830=CARTESIAN_POINT('Ctrl Pts',(-3.5680766948491,1.65448411889468,37.7593876713502));
#33831=CARTESIAN_POINT('Ctrl Pts',(-3.61687947545567,1.54923556308354,37.7652409301875));
#33832=CARTESIAN_POINT('Ctrl Pts',(-3.66100169490512,1.44186859615042,37.7710941890248));
#33833=CARTESIAN_POINT('Ctrl Pts',(-3.700273731881,1.33284031644884,37.7769474478621));
#33834=CARTESIAN_POINT('Ctrl Pts',(-3.73959044845629,1.22368799582054,37.7828073659227));
#33835=CARTESIAN_POINT('Ctrl Pts',(-3.77404582853623,1.11287097908174,37.7886672839832));
#33836=CARTESIAN_POINT('Ctrl Pts',(-3.80351997677793,1.00086202158501,37.7945272020437));
#33837=CARTESIAN_POINT('Ctrl Pts',(-3.83301397080609,0.888777645255649,
37.8003910657546));
#33838=CARTESIAN_POINT('Ctrl Pts',(-3.85751996731369,0.775500133178225,
37.8062549294654));
#33839=CARTESIAN_POINT('Ctrl Pts',(-3.87696942368802,0.661511215164319,
37.8121187931763));
#33840=CARTESIAN_POINT('Ctrl Pts',(-3.89644757268481,0.547354136101277,
37.8179913074954));
#33841=CARTESIAN_POINT('Ctrl Pts',(-3.91085424229471,0.432483965168503,
37.8238638218144));
#33842=CARTESIAN_POINT('Ctrl Pts',(-3.92017281141304,0.317386402761613,
37.8297363361335));
#33843=CARTESIAN_POINT('Ctrl Pts',(-3.92274826362267,0.285575910436055,
37.8313593728667));
#33844=CARTESIAN_POINT('Ctrl Pts',(-3.92493536749216,0.253748039177028,
37.8329824095998));
#33845=CARTESIAN_POINT('Ctrl Pts',(-3.92673447276226,0.221913001918477,
37.8346054463329));
#33846=CARTESIAN_POINT('Ctrl Pts',(-3.93324439359981,0.106720424887167,
37.8404782770253));
#33847=CARTESIAN_POINT('Ctrl Pts',(-3.93469208920761,-0.00895199463281238,
37.8463511077176));
#33848=CARTESIAN_POINT('Ctrl Pts',(-3.93102510557173,-0.124621905637643,
37.85222393841));
#33849=CARTESIAN_POINT('Ctrl Pts',(-3.92718047745846,-0.245895365207376,
37.8583812743096));
#33850=CARTESIAN_POINT('Ctrl Pts',(-3.91771306451741,-0.36716563417689,
37.8645386102092));
#33851=CARTESIAN_POINT('Ctrl Pts',(-3.90262370181262,-0.487870107764704,
37.8706959461088));
#33852=CARTESIAN_POINT('Ctrl Pts',(-3.88826876487249,-0.602699682786761,
37.876553593664));
#33853=CARTESIAN_POINT('Ctrl Pts',(-3.86882626391864,-0.717016759625243,
37.8824112412192));
#33854=CARTESIAN_POINT('Ctrl Pts',(-3.84435019811851,-0.830337614603938,
37.8882688887744));
#33855=CARTESIAN_POINT('Ctrl Pts',(-3.81989064215858,-0.943582031268476,
37.8941225851708));
#33856=CARTESIAN_POINT('Ctrl Pts',(-3.79040435949656,-1.05583115968554,
37.8999762815671));
#33857=CARTESIAN_POINT('Ctrl Pts',(-3.75599681193477,-1.16660916708889,
37.9058299779635));
#33858=CARTESIAN_POINT('Ctrl Pts',(-3.72160413907796,-1.27733928412237,
37.911681143752));
#33859=CARTESIAN_POINT('Ctrl Pts',(-3.68229455560271,-1.38659915110984,
37.9175323095406));
#33860=CARTESIAN_POINT('Ctrl Pts',(-3.63822380843997,-1.49392654427871,
37.9233834753292));
#33861=CARTESIAN_POINT('Ctrl Pts',(-3.59416143914316,-1.60123353446901,
37.9292335288089));
#33862=CARTESIAN_POINT('Ctrl Pts',(-3.54533986516638,-1.70660840017188,
37.9350835822886));
#33863=CARTESIAN_POINT('Ctrl Pts',(-3.49196329098949,-1.80960807203711,
37.9409336357683));
#33864=CARTESIAN_POINT('Ctrl Pts',(-3.43856616530903,-1.91264740171395,
37.9467859416855));
#33865=CARTESIAN_POINT('Ctrl Pts',(-3.38061072430561,-2.01330934241119,
37.9526382476027));
#33866=CARTESIAN_POINT('Ctrl Pts',(-3.31834743433787,-2.1111748636774,37.9584905535198));
#33867=CARTESIAN_POINT('Ctrl Pts',(-3.25607013218143,-2.20906240932026,
37.964344176483));
#33868=CARTESIAN_POINT('Ctrl Pts',(-3.18948328170545,-2.30415193962538,
37.9701977994461));
#33869=CARTESIAN_POINT('Ctrl Pts',(-3.1188803022657,-2.39605397688346,37.9760514224093));
#33870=CARTESIAN_POINT('Ctrl Pts',(-3.04821565354052,-2.48803628742478,
37.9819101583116));
#33871=CARTESIAN_POINT('Ctrl Pts',(-2.97352813414324,-2.57682522667805,
37.987768894214));
#33872=CARTESIAN_POINT('Ctrl Pts',(-2.89515090838893,-2.66206502881781,
37.9936276301164));
#33873=CARTESIAN_POINT('Ctrl Pts',(-2.86673472889935,-2.69296928058161,
37.995751753411));
#33874=CARTESIAN_POINT('Ctrl Pts',(-2.83783389725777,-2.72340736054617,
37.9978758767055));
#33875=CARTESIAN_POINT('Ctrl Pts',(-2.80846544028688,-2.75336355585568,
38.));
#33876=CARTESIAN_POINT('Origin',(0.,0.,32.));
#33877=CARTESIAN_POINT('',(3.93133412486678,0.00259602383233126,35.9708370172092));
#33878=CARTESIAN_POINT('',(3.93121085245411,0.00231623353798856,36.1541640353064));
#33879=CARTESIAN_POINT('',(3.933,4.81653586104654E-16,32.));
#33880=CARTESIAN_POINT('',(0.65368646409381,3.87829640520945,35.));
#33881=CARTESIAN_POINT('Ctrl Pts',(0.65368646409381,3.87829640520945,35.));
#33882=CARTESIAN_POINT('Ctrl Pts',(0.539330922767402,3.89757102005291,35.0058615808379));
#33883=CARTESIAN_POINT('Ctrl Pts',(0.424217848923065,3.91176742009041,35.0117231616759));
#33884=CARTESIAN_POINT('Ctrl Pts',(0.308833568652951,3.92085587938056,35.0175847425138));
#33885=CARTESIAN_POINT('Ctrl Pts',(0.193261297999275,3.92995914608592,35.02345587336));
#33886=CARTESIAN_POINT('Ctrl Pts',(0.0774173514306077,3.9339378322415,35.0293270042062));
#33887=CARTESIAN_POINT('Ctrl Pts',(-0.0382115899189808,3.93281437070145,
35.0351981350524));
#33888=CARTESIAN_POINT('Ctrl Pts',(-0.132391795727835,3.93189930706924,
35.0399801931165));
#33889=CARTESIAN_POINT('Ctrl Pts',(-0.226429308324548,3.92760039491556,
35.0447622511807));
#33890=CARTESIAN_POINT('Ctrl Pts',(-0.320064996648115,3.91995502498698,
35.0495443092448));
#33891=CARTESIAN_POINT('Ctrl Pts',(-0.435044857224395,3.91056689975203,
35.0554164332108));
#33892=CARTESIAN_POINT('Ctrl Pts',(-0.549804072018368,3.89609987364649,
35.0612885571768));
#33893=CARTESIAN_POINT('Ctrl Pts',(-0.663857834012495,3.87656829892371,
35.0671606811429));
#33894=CARTESIAN_POINT('Ctrl Pts',(-0.777763723039442,3.85706204727539,
35.0730251917836));
#33895=CARTESIAN_POINT('Ctrl Pts',(-0.890965574426317,3.83250437410963,
35.0788897024243));
#33896=CARTESIAN_POINT('Ctrl Pts',(-1.00298187849455,3.80296152378795,35.084754213065));
#33897=CARTESIAN_POINT('Ctrl Pts',(-1.11488291890037,3.77344907276532,35.0906126891826));
#33898=CARTESIAN_POINT('Ctrl Pts',(-1.22560044112233,3.73896175259171,35.0964711653002));
#33899=CARTESIAN_POINT('Ctrl Pts',(-1.33466199872459,3.69961705439367,35.1023296414178));
#33900=CARTESIAN_POINT('Ctrl Pts',(-1.44802399800991,3.65872094262829,35.108419125009));
#33901=CARTESIAN_POINT('Ctrl Pts',(-1.55959630369201,3.61257658314203,35.1145086086003));
#33902=CARTESIAN_POINT('Ctrl Pts',(-1.66886409402027,3.56137356025592,35.1205980921916));
#33903=CARTESIAN_POINT('Ctrl Pts',(-1.77386489214357,3.51217005524117,35.126449776712));
#33904=CARTESIAN_POINT('Ctrl Pts',(-1.87673737398393,3.45829575416629,35.1323014612324));
#33905=CARTESIAN_POINT('Ctrl Pts',(-1.97704478296076,3.39996807722773,35.1381531457528));
#33906=CARTESIAN_POINT('Ctrl Pts',(-2.07733689287734,3.34164929652778,35.1440039377641));
#33907=CARTESIAN_POINT('Ctrl Pts',(-2.17506435053188,3.27887869825674,35.1498547297754));
#33908=CARTESIAN_POINT('Ctrl Pts',(-2.26981594510763,3.21191914209171,35.1557055217867));
#33909=CARTESIAN_POINT('Ctrl Pts',(-2.36457603781286,3.14495358042376,35.1615568385468));
#33910=CARTESIAN_POINT('Ctrl Pts',(-2.45635939922802,3.07379855260523,35.167408155307));
#33911=CARTESIAN_POINT('Ctrl Pts',(-2.54478528928676,2.99875921531384,35.1732594720671));
#33912=CARTESIAN_POINT('Ctrl Pts',(-2.63324052778291,2.92369497256443,35.1791127308716));
#33913=CARTESIAN_POINT('Ctrl Pts',(-2.71833576408511,2.84474412420826,35.1849659896761));
#33914=CARTESIAN_POINT('Ctrl Pts',(-2.79972525940178,2.76225043612407,35.1908192484807));
#33915=CARTESIAN_POINT('Ctrl Pts',(-2.88120735114467,2.67966289537901,35.1966791665088));
#33916=CARTESIAN_POINT('Ctrl Pts',(-2.95897499634738,2.59352476425835,35.2025390845369));
#33917=CARTESIAN_POINT('Ctrl Pts',(-3.03272102596396,2.50421488268801,35.208399002565));
#33918=CARTESIAN_POINT('Ctrl Pts',(-3.10651671089285,2.4148448662184,35.2142628662436));
#33919=CARTESIAN_POINT('Ctrl Pts',(-3.1762851400794,2.32229917614978,35.2201267299223));
#33920=CARTESIAN_POINT('Ctrl Pts',(-3.24176199442419,2.22698634290983,35.2259905936009));
#33921=CARTESIAN_POINT('Ctrl Pts',(-3.3073354428715,2.13153290032515,35.2318631078883));
#33922=CARTESIAN_POINT('Ctrl Pts',(-3.36860446279633,2.03330451671135,35.2377356221756));
#33923=CARTESIAN_POINT('Ctrl Pts',(-3.42535020062493,1.93273510939258,35.243608136463));
#33924=CARTESIAN_POINT('Ctrl Pts',(-3.44103350599065,1.90493988131405,35.2452311735114));
#33925=CARTESIAN_POINT('Ctrl Pts',(-3.45637158232295,1.8769659537885,35.2468542105598));
#33926=CARTESIAN_POINT('Ctrl Pts',(-3.47136046246102,1.8488227442517,35.2484772476082));
#33927=CARTESIAN_POINT('Ctrl Pts',(-3.52559000846581,1.74700102960462,35.2543493715742));
#33928=CARTESIAN_POINT('Ctrl Pts',(-3.57542672946076,1.6426206029676,35.2602214955402));
#33929=CARTESIAN_POINT('Ctrl Pts',(-3.62062073765856,1.53609715644447,35.2660936195063));
#33930=CARTESIAN_POINT('Ctrl Pts',(-3.66575615092748,1.4297118196846,35.271958130147));
#33931=CARTESIAN_POINT('Ctrl Pts',(-3.70626066176825,1.32118936546262,35.2778226407877));
#33932=CARTESIAN_POINT('Ctrl Pts',(-3.74192982829283,1.21097075114654,35.2836871514284));
#33933=CARTESIAN_POINT('Ctrl Pts',(-3.77756229159994,1.10086555068798,35.289545627546));
#33934=CARTESIAN_POINT('Ctrl Pts',(-3.80836918061562,0.989068052643565,
35.2954041036637));
#33935=CARTESIAN_POINT('Ctrl Pts',(-3.8341940719254,0.876039279263296,35.3012625797813));
#33936=CARTESIAN_POINT('Ctrl Pts',(-3.86103727290798,0.758553631627159,
35.3073520633725));
#33937=CARTESIAN_POINT('Ctrl Pts',(-3.88249732192508,0.639738028258825,
35.3134415469638));
#33938=CARTESIAN_POINT('Ctrl Pts',(-3.89845556038526,0.52012810316428,35.3195310305551));
#33939=CARTESIAN_POINT('Ctrl Pts',(-3.91379061722067,0.405189038681629,
35.3253827150755));
#33940=CARTESIAN_POINT('Ctrl Pts',(-3.92404544006576,0.289516974445092,
35.3312343995959));
#33941=CARTESIAN_POINT('Ctrl Pts',(-3.92916697493633,0.173596898214589,
35.3370860841163));
#33942=CARTESIAN_POINT('Ctrl Pts',(-3.9342877286615,0.0576945023155024,
35.3429368761276));
#33943=CARTESIAN_POINT('Ctrl Pts',(-3.93427673289576,-0.0584554174693667,
35.3487876681389));
#33944=CARTESIAN_POINT('Ctrl Pts',(-3.92913297192955,-0.174364815533547,
35.3546384601502));
#33945=CARTESIAN_POINT('Ctrl Pts',(-3.92398874962709,-0.290284609338774,
35.3604897769103));
#33946=CARTESIAN_POINT('Ctrl Pts',(-3.91371086531983,-0.405963425509345,
35.3663410936704));
#33947=CARTESIAN_POINT('Ctrl Pts',(-3.89835035856407,-0.520916002713838,
35.3721924104306));
#33948=CARTESIAN_POINT('Ctrl Pts',(-3.88298475367618,-0.635906732528653,
35.3780456692351));
#33949=CARTESIAN_POINT('Ctrl Pts',(-3.86253322674438,-0.750170334535612,
35.3838989280396));
#33950=CARTESIAN_POINT('Ctrl Pts',(-3.8370982175806,-0.863230136545143,
35.3897521868441));
#33951=CARTESIAN_POINT('Ctrl Pts',(-3.81163427113265,-0.976418566132486,
35.3956121048722));
#33952=CARTESIAN_POINT('Ctrl Pts',(-3.78117561670702,-1.08840005854956,
35.4014720229003));
#33953=CARTESIAN_POINT('Ctrl Pts',(-3.74587504796018,-1.19871144362158,
35.4073319409285));
#33954=CARTESIAN_POINT('Ctrl Pts',(-3.71055071033013,-1.3090971045062,35.4131958046071));
#33955=CARTESIAN_POINT('Ctrl Pts',(-3.67037810963136,-1.41781003204734,
35.4190596682857));
#33956=CARTESIAN_POINT('Ctrl Pts',(-3.62555817622155,-1.52440706861163,
35.4249235319644));
#33957=CARTESIAN_POINT('Ctrl Pts',(-3.58067212263409,-1.6311613614335,35.4307960462517));
#33958=CARTESIAN_POINT('Ctrl Pts',(-3.53112522943475,-1.73579316120889,
35.4366685605391));
#33959=CARTESIAN_POINT('Ctrl Pts',(-3.47716435577114,-1.8378838491468,35.4425410748265));
#33960=CARTESIAN_POINT('Ctrl Pts',(-3.46225072715634,-1.86609952657313,
35.4441641118749));
#33961=CARTESIAN_POINT('Ctrl Pts',(-3.44700018962873,-1.89412127369666,
35.4457871489232));
#33962=CARTESIAN_POINT('Ctrl Pts',(-3.43141852376622,-1.92194066369231,
35.4474101859715));
#33963=CARTESIAN_POINT('Ctrl Pts',(-3.37504428780202,-2.0225908040453,35.4532823099376));
#33964=CARTESIAN_POINT('Ctrl Pts',(-3.31414339153919,-2.12092723197976,
35.4591544339036));
#33965=CARTESIAN_POINT('Ctrl Pts',(-3.24893058939597,-2.21651506317623,
35.4650265578697));
#33966=CARTESIAN_POINT('Ctrl Pts',(-3.18380233694565,-2.31197896285149,
35.4708910685104));
#33967=CARTESIAN_POINT('Ctrl Pts',(-3.11437352686747,-2.40470101416566,
35.4767555791511));
#33968=CARTESIAN_POINT('Ctrl Pts',(-3.04090472941805,-2.49427092085101,
35.4826200897918));
#33969=CARTESIAN_POINT('Ctrl Pts',(-2.96751153063028,-2.58374866099349,
35.4884785659094));
#33970=CARTESIAN_POINT('Ctrl Pts',(-2.89008687375796,-2.67008039031691,
35.494337042027));
#33971=CARTESIAN_POINT('Ctrl Pts',(-2.80893415916184,-2.75288537529149,
35.5001955181447));
#33972=CARTESIAN_POINT('Ctrl Pts',(-2.72458148553147,-2.83895547051,35.5062850017359));
#33973=CARTESIAN_POINT('Ctrl Pts',(-2.63620095757036,-2.92121459514035,
35.5123744853272));
#33974=CARTESIAN_POINT('Ctrl Pts',(-2.54417916322711,-2.99927347626071,
35.5184639689185));
#33975=CARTESIAN_POINT('Ctrl Pts',(-2.45575089153084,-3.0742840973563,35.5243156534389));
#33976=CARTESIAN_POINT('Ctrl Pts',(-2.36396075026656,-3.14541607190399,
35.5301673379593));
#33977=CARTESIAN_POINT('Ctrl Pts',(-2.26918816081457,-3.21236269602593,
35.5360190224797));
#33978=CARTESIAN_POINT('Ctrl Pts',(-2.17443002624266,-3.27929910933239,
35.541869814491));
#33979=CARTESIAN_POINT('Ctrl Pts',(-2.07669068551382,-3.34205120300941,
35.5477206065023));
#33980=CARTESIAN_POINT('Ctrl Pts',(-1.97638025177208,-3.40035440805886,
35.5535713985136));
#33981=CARTESIAN_POINT('Ctrl Pts',(-1.87606082133687,-3.45866284223598,
35.5594227152738));
#33982=CARTESIAN_POINT('Ctrl Pts',(-1.77317019692764,-3.51252138682477,
35.5652740320339));
#33983=CARTESIAN_POINT('Ctrl Pts',(-1.66814427682793,-3.5617107787812,35.5711253487941));
#33984=CARTESIAN_POINT('Ctrl Pts',(-1.56308349876298,-3.61091649663237,
35.5769786075986));
#33985=CARTESIAN_POINT('Ctrl Pts',(-1.45588638998729,-3.65544980515002,
35.5828318664031));
#33986=CARTESIAN_POINT('Ctrl Pts',(-1.34700939553298,-3.69513933273779,
35.5886851252076));
#33987=CARTESIAN_POINT('Ctrl Pts',(-1.23800853226013,-3.73487401490496,
35.5945450432357));
#33988=CARTESIAN_POINT('Ctrl Pts',(-1.12732435725081,-3.76975377516615,
35.6004049612638));
#33989=CARTESIAN_POINT('Ctrl Pts',(-1.01542916296309,-3.79965690753837,
35.6062648792919));
#33990=CARTESIAN_POINT('Ctrl Pts',(-0.903458626439311,-3.82958017454527,
35.6121287429706));
#33991=CARTESIAN_POINT('Ctrl Pts',(-0.790275849730697,-3.85452005260933,
35.6179926066492));
#33992=CARTESIAN_POINT('Ctrl Pts',(-0.676362296463616,-3.87440615371214,
35.6238564703278));
#33993=CARTESIAN_POINT('Ctrl Pts',(-0.562280693316787,-3.89432159159536,
35.6297289846152));
#33994=CARTESIAN_POINT('Ctrl Pts',(-0.447466570445664,-3.90916831983273,
35.6356014989026));
#33995=CARTESIAN_POINT('Ctrl Pts',(-0.33240556098613,-3.91892785631804,
35.64147401319));
#33996=CARTESIAN_POINT('Ctrl Pts',(-0.300605164761025,-3.92162518296817,
35.6430970502384));
#33997=CARTESIAN_POINT('Ctrl Pts',(-0.268785901634046,-3.92393423057186,
35.6447200872867));
#33998=CARTESIAN_POINT('Ctrl Pts',(-0.236957985810335,-3.92585530973324,
35.6463431243351));
#33999=CARTESIAN_POINT('Ctrl Pts',(-0.12180505847427,-3.93280574564311,
35.6522152483011));
#34000=CARTESIAN_POINT('Ctrl Pts',(-0.00615301487706181,-3.93469705103759,
35.6580873722671));
#34001=CARTESIAN_POINT('Ctrl Pts',(0.109516173067406,-3.93147494050727,
35.6639594962331));
#34002=CARTESIAN_POINT('Ctrl Pts',(0.225035393613353,-3.92825700750722,
35.6698240068738));
#34003=CARTESIAN_POINT('Ctrl Pts',(0.340571304870519,-3.9199388539467,35.6756885175145));
#34004=CARTESIAN_POINT('Ctrl Pts',(0.455637867855379,-3.90651803187649,
35.6815530281552));
#34005=CARTESIAN_POINT('Ctrl Pts',(0.570586028491408,-3.89311101969871,
35.6874115042727));
#34006=CARTESIAN_POINT('Ctrl Pts',(0.685065393318412,-3.87461183029995,
35.6932699803903));
#34007=CARTESIAN_POINT('Ctrl Pts',(0.798591655527019,-3.85107002892996,
35.6991284565079));
#34008=CARTESIAN_POINT('Ctrl Pts',(0.91659440863619,-3.8265999431475,35.7052179400992));
#34009=CARTESIAN_POINT('Ctrl Pts',(1.03356689370182,-3.79668140298861,35.7113074236904));
#34010=CARTESIAN_POINT('Ctrl Pts',(1.14897266828838,-3.76142935697672,35.7173969072817));
#34011=CARTESIAN_POINT('Ctrl Pts',(1.25987175760961,-3.7275539307822,35.7232485918021));
#34012=CARTESIAN_POINT('Ctrl Pts',(1.36932377014749,-3.68875386908664,35.7291002763224));
#34013=CARTESIAN_POINT('Ctrl Pts',(1.47686561295159,-3.64518270615906,35.7349519608428));
#34014=CARTESIAN_POINT('Ctrl Pts',(1.58439105328696,-3.60161818878097,35.7408027528541));
#34015=CARTESIAN_POINT('Ctrl Pts',(1.69000652011514,-3.55328417225595,35.7466535448653));
#34016=CARTESIAN_POINT('Ctrl Pts',(1.79326779031035,-3.50038278367315,35.7525043368766));
#34017=CARTESIAN_POINT('Ctrl Pts',(1.89653832185472,-3.4474766504438,35.7583556536367));
#34018=CARTESIAN_POINT('Ctrl Pts',(1.99745386907001,-3.39000251933694,35.7642069703967));
#34019=CARTESIAN_POINT('Ctrl Pts',(2.09559439821291,-3.32820869510592,35.7700582871568));
#34020=CARTESIAN_POINT('Ctrl Pts',(2.19376750006895,-3.26639436158554,35.7759115459613));
#34021=CARTESIAN_POINT('Ctrl Pts',(2.28916340279892,-3.2002577042806,35.7817648047657));
#34022=CARTESIAN_POINT('Ctrl Pts',(2.38139126813706,-3.13009019487308,35.7876180635702));
#34023=CARTESIAN_POINT('Ctrl Pts',(2.4737240606623,-3.05984285623649,35.7934779815983));
#34024=CARTESIAN_POINT('Ctrl Pts',(2.56288129257514,-2.98555576266775,35.7993378996263));
#34025=CARTESIAN_POINT('Ctrl Pts',(2.64850535321294,-2.90756055723736,35.8051978176544));
#34026=CARTESIAN_POINT('Ctrl Pts',(2.73418706698117,-2.82951283540307,35.811061681333));
#34027=CARTESIAN_POINT('Ctrl Pts',(2.81633058015491,-2.74775232106522,35.8169255450116));
#34028=CARTESIAN_POINT('Ctrl Pts',(2.89461650753271,-2.66264610384466,35.8227894086902));
#34029=CARTESIAN_POINT('Ctrl Pts',(2.9730179254756,-2.57741433449169,35.8286619229776));
#34030=CARTESIAN_POINT('Ctrl Pts',(3.04755013455306,-2.48882732664115,35.834534437265));
#34031=CARTESIAN_POINT('Ctrl Pts',(3.11793517238354,-2.39728372555558,35.8404069515523));
#34032=CARTESIAN_POINT('Ctrl Pts',(3.13738808786115,-2.37198303681087,35.842029988601));
#34033=CARTESIAN_POINT('Ctrl Pts',(3.15652448380116,-2.34645666696298,35.8436530256498));
#34034=CARTESIAN_POINT('Ctrl Pts',(3.17533910233628,-2.32071337850546,35.8452760626985));
#34035=CARTESIAN_POINT('Ctrl Pts',(3.24386965336691,-2.22694577221349,35.8511878287586));
#34036=CARTESIAN_POINT('Ctrl Pts',(3.30835742877721,-2.12998392340895,35.8570995948188));
#34037=CARTESIAN_POINT('Ctrl Pts',(3.36849264223259,-2.03020844230953,35.8630113608789));
#34038=CARTESIAN_POINT('Ctrl Pts',(3.42854818206181,-1.9305651545445,35.8689152943929));
#34039=CARTESIAN_POINT('Ctrl Pts',(3.48426242031965,-1.82811599172916,35.8748192279068));
#34040=CARTESIAN_POINT('Ctrl Pts',(3.53536685330977,-1.72327311025228,35.8807231614208));
#34041=CARTESIAN_POINT('Ctrl Pts',(3.58641539569186,-1.61854489069514,35.8866206380695));
#34042=CARTESIAN_POINT('Ctrl Pts',(3.63286398405451,-1.51142852206661,35.8925181147183));
#34043=CARTESIAN_POINT('Ctrl Pts',(3.67448867569264,-1.40236299587752,35.898415591367));
#34044=CARTESIAN_POINT('Ctrl Pts',(3.71708453564452,-1.29075280259325,35.9044506652502));
#34045=CARTESIAN_POINT('Ctrl Pts',(3.75462837515732,-1.17710173246275,35.9104857391334));
#34046=CARTESIAN_POINT('Ctrl Pts',(3.78693102001708,-1.06190510387342,35.9165208130165));
#34047=CARTESIAN_POINT('Ctrl Pts',(3.81844890924432,-0.949507044984043,
35.9224092717156));
#34048=CARTESIAN_POINT('Ctrl Pts',(3.84497722627513,-0.835638076692662,
35.9282977304147));
#34049=CARTESIAN_POINT('Ctrl Pts',(3.8663899645524,-0.720775722405051,35.9341861891138));
#34050=CARTESIAN_POINT('Ctrl Pts',(3.88860242803569,-0.601623476803267,
35.940294570589));
#34051=CARTESIAN_POINT('Ctrl Pts',(3.90530960984758,-0.481402630182505,
35.9464029520642));
#34052=CARTESIAN_POINT('Ctrl Pts',(3.91642873442305,-0.360659074730551,
35.9525113335394));
#34053=CARTESIAN_POINT('Ctrl Pts',(3.92754785899851,-0.239915519278558,
35.9586197150147));
#34054=CARTESIAN_POINT('Ctrl Pts',(3.93307887719384,-0.118649740920967,
35.9647280964899));
#34055=CARTESIAN_POINT('Ctrl Pts',(3.93299914955306,0.00258642898096291,
35.9708364779651));
#34056=CARTESIAN_POINT('',(3.48437472100057,1.8241770209199,35.));
#34057=CARTESIAN_POINT('Origin',(0.,0.,35.));
#34058=CARTESIAN_POINT('Ctrl Pts',(3.93299932332396,0.0023071049629667,
36.154163522035));
#34059=CARTESIAN_POINT('Ctrl Pts',(3.93306815257745,-0.11502843536642,36.1482539137099));
#34060=CARTESIAN_POINT('Ctrl Pts',(3.92788182847184,-0.232374625365518,
36.1423443053847));
#34061=CARTESIAN_POINT('Ctrl Pts',(3.91746406086123,-0.349233921406056,
36.1364346970596));
#34062=CARTESIAN_POINT('Ctrl Pts',(3.90704445346722,-0.466113854861418,
36.1305240450945));
#34063=CARTESIAN_POINT('Ctrl Pts',(3.89139159917373,-0.582506322944185,
36.1246133931293));
#34064=CARTESIAN_POINT('Ctrl Pts',(3.87058107839869,-0.697919132523272,
36.1187027411642));
#34065=CARTESIAN_POINT('Ctrl Pts',(3.84976222824505,-0.813378135899996,
36.1127897234698));
#34066=CARTESIAN_POINT('Ctrl Pts',(3.82378167424935,-0.927856305137044,
36.1068767057753));
#34067=CARTESIAN_POINT('Ctrl Pts',(3.79276595892408,-1.04087241332774,36.1009636880809));
#34068=CARTESIAN_POINT('Ctrl Pts',(3.76170851327563,-1.15404057987561,36.0950427146732));
#34069=CARTESIAN_POINT('Ctrl Pts',(3.72560248091587,-1.26574236800933,36.0891217412655));
#34070=CARTESIAN_POINT('Ctrl Pts',(3.68462423432077,-1.37551199626033,36.0832007678578));
#34071=CARTESIAN_POINT('Ctrl Pts',(3.64361753378841,-1.48535784490568,36.0772756831222));
#34072=CARTESIAN_POINT('Ctrl Pts',(3.59773203505403,-1.59326849094606,36.0713505983866));
#34073=CARTESIAN_POINT('Ctrl Pts',(3.54719143757431,-1.69880013692002,36.0654255136511));
#34074=CARTESIAN_POINT('Ctrl Pts',(3.49655766018267,-1.80452634785695,36.0594895050464));
#34075=CARTESIAN_POINT('Ctrl Pts',(3.4412518234525,-1.90786443959993,36.0535534964416));
#34076=CARTESIAN_POINT('Ctrl Pts',(3.38154295267334,-2.00839643975617,36.0476174878369));
#34077=CARTESIAN_POINT('Ctrl Pts',(3.32921850769105,-2.09649526062636,36.0424156082569));
#34078=CARTESIAN_POINT('Ctrl Pts',(3.27351353645545,-2.18243944889097,36.0372137286769));
#34079=CARTESIAN_POINT('Ctrl Pts',(3.21463464360123,-2.26596847024816,36.0320118490969));
#34080=CARTESIAN_POINT('Ctrl Pts',(3.14816940685497,-2.36025992021537,36.026139725131));
#34081=CARTESIAN_POINT('Ctrl Pts',(3.07744059861696,-2.45178263820824,36.0202676011652));
#34082=CARTESIAN_POINT('Ctrl Pts',(3.00270672808036,-2.54012623803246,36.0143954771994));
#34083=CARTESIAN_POINT('Ctrl Pts',(2.92806975149084,-2.62835529862533,36.0085309665588));
#34084=CARTESIAN_POINT('Ctrl Pts',(2.84943830341971,-2.71341312508545,36.0026664559183));
#34085=CARTESIAN_POINT('Ctrl Pts',(2.7671139252641,-2.79491851842044,35.9968019452778));
#34086=CARTESIAN_POINT('Ctrl Pts',(2.68487425807463,-2.87634004351652,35.9909434691604));
#34087=CARTESIAN_POINT('Ctrl Pts',(2.59894951117365,-2.95421611717767,35.985084993043));
#34088=CARTESIAN_POINT('Ctrl Pts',(2.50968077474067,-3.02819936742894,35.9792265169256));
#34089=CARTESIAN_POINT('Ctrl Pts',(2.41689205377746,-3.1050998752419,35.9731370333342));
#34090=CARTESIAN_POINT('Ctrl Pts',(2.32049049587995,-3.17779389798758,35.9670475497429));
#34091=CARTESIAN_POINT('Ctrl Pts',(2.22090081590631,-3.24593415920698,35.9609580661516));
#34092=CARTESIAN_POINT('Ctrl Pts',(2.12520019040444,-3.31141349022082,35.9551063816313));
#34093=CARTESIAN_POINT('Ctrl Pts',(2.02655614087375,-3.37268778603635,35.9492546971111));
#34094=CARTESIAN_POINT('Ctrl Pts',(1.92537772850614,-3.42949115796681,35.9434030125909));
#34095=CARTESIAN_POINT('Ctrl Pts',(1.8242147480458,-3.48628586614828,35.9375522205798));
#34096=CARTESIAN_POINT('Ctrl Pts',(1.72051853370941,-3.53861080397351,35.9317014285687));
#34097=CARTESIAN_POINT('Ctrl Pts',(1.61472432391119,-3.58624516141459,35.9258506365576));
#34098=CARTESIAN_POINT('Ctrl Pts',(1.50892062558798,-3.63388379111019,35.9199993197976));
#34099=CARTESIAN_POINT('Ctrl Pts',(1.40101893473241,-3.67683083438635,35.9141480030377));
#34100=CARTESIAN_POINT('Ctrl Pts',(1.29147545916237,-3.71491320738202,35.9082966862778));
#34101=CARTESIAN_POINT('Ctrl Pts',(1.18189562625586,-3.75300821986755,35.9024434274734));
#34102=CARTESIAN_POINT('Ctrl Pts',(1.07067331540675,-3.78623521590995,35.8965901686691));
#34103=CARTESIAN_POINT('Ctrl Pts',(0.958280226486698,-3.81447086861659,
35.8907369098648));
#34104=CARTESIAN_POINT('Ctrl Pts',(0.845759268505086,-3.84273864488571,
35.8848769918369));
#34105=CARTESIAN_POINT('Ctrl Pts',(0.732065275031789,-3.86600364264212,
35.8790170738089));
#34106=CARTESIAN_POINT('Ctrl Pts',(0.617680580600549,-3.88419357143139,
35.873157155781));
#34107=CARTESIAN_POINT('Ctrl Pts',(0.503218867680946,-3.90239574802031,
35.8672932921026));
#34108=CARTESIAN_POINT('Ctrl Pts',(0.388065937513293,-3.91551600466352,
35.8614294284241));
#34109=CARTESIAN_POINT('Ctrl Pts',(0.272707948110416,-3.92353404152907,
35.8555655647457));
#34110=CARTESIAN_POINT('Ctrl Pts',(0.1571797779379,-3.93156390692675,35.8496930504585));
#34111=CARTESIAN_POINT('Ctrl Pts',(0.0414463565074991,-3.93447651968868,
35.8438205361713));
#34112=CARTESIAN_POINT('Ctrl Pts',(-0.0740073703216252,-3.93230363898035,
35.8379480218841));
#34113=CARTESIAN_POINT('Ctrl Pts',(-0.105916305245342,-3.93170310133619,
35.8363249848339));
#34114=CARTESIAN_POINT('Ctrl Pts',(-0.137803915726344,-3.93071441185742,
35.8347019477837));
#34115=CARTESIAN_POINT('Ctrl Pts',(-0.169660074222265,-3.929338934123,35.8330789107334));
#34116=CARTESIAN_POINT('Ctrl Pts',(-0.284915182996696,-3.92436247608846,
35.8272067867675));
#34117=CARTESIAN_POINT('Ctrl Pts',(-0.400144376111135,-3.91430239267515,
35.8213346628015));
#34118=CARTESIAN_POINT('Ctrl Pts',(-0.514862652605059,-3.89915445307729,
35.8154625388356));
#34119=CARTESIAN_POINT('Ctrl Pts',(-0.62943219457563,-3.8840261530839,35.8095980281949));
#34120=CARTESIAN_POINT('Ctrl Pts',(-0.743491731159177,-3.86382316858314,
35.8037335175543));
#34121=CARTESIAN_POINT('Ctrl Pts',(-0.856557568373406,-3.83859324910341,
35.7978690069137));
#34122=CARTESIAN_POINT('Ctrl Pts',(-0.969507061966085,-3.81338929095979,
35.7920105307961));
#34123=CARTESIAN_POINT('Ctrl Pts',(-1.08146448894426,-3.78316877600975,
35.7861520546786));
#34124=CARTESIAN_POINT('Ctrl Pts',(-1.19195324869756,-3.7480310101331,35.7802935785611));
#34125=CARTESIAN_POINT('Ctrl Pts',(-1.30679872660717,-3.71150771560258,
35.7742040949698));
#34126=CARTESIAN_POINT('Ctrl Pts',(-1.4200568803427,-3.66967146433403,35.7681146113785));
#34127=CARTESIAN_POINT('Ctrl Pts',(-1.5312060032593,-3.62269197912032,35.7620251277872));
#34128=CARTESIAN_POINT('Ctrl Pts',(-1.63801466646809,-3.57754707934744,
35.7561734432669));
#34129=CARTESIAN_POINT('Ctrl Pts',(-1.74287550973644,-3.52765327827911,
35.7503217587465));
#34130=CARTESIAN_POINT('Ctrl Pts',(-1.84534376791724,-3.47321110475724,
35.7444700742262));
#34131=CARTESIAN_POINT('Ctrl Pts',(-1.94779639746115,-3.41877723485033,
35.738619282215));
#34132=CARTESIAN_POINT('Ctrl Pts',(-2.0478568025135,-3.35979656575146,35.7327684902038));
#34133=CARTESIAN_POINT('Ctrl Pts',(-2.14510400419289,-3.29651601106314,
35.7269176981926));
#34134=CARTESIAN_POINT('Ctrl Pts',(-2.24235992782914,-3.233229780836,35.7210663814325));
#34135=CARTESIAN_POINT('Ctrl Pts',(-2.33680179998934,-3.16564312387548,
35.7152150646724));
#34136=CARTESIAN_POINT('Ctrl Pts',(-2.42803746981478,-3.09404638704326,
35.7093637479124));
#34137=CARTESIAN_POINT('Ctrl Pts',(-2.51930342063967,-3.02242588734775,
35.703510489108));
#34138=CARTESIAN_POINT('Ctrl Pts',(-2.60736072811292,-2.94679291637804,
35.6976572303035));
#34139=CARTESIAN_POINT('Ctrl Pts',(-2.69185073787341,-2.86747774272276,
35.6918039714991));
#34140=CARTESIAN_POINT('Ctrl Pts',(-2.77643687150012,-2.78807233258669,
35.6859440534711));
#34141=CARTESIAN_POINT('Ctrl Pts',(-2.85744730517025,-2.70497664130493,
35.680084135443));
#34142=CARTESIAN_POINT('Ctrl Pts',(-2.93456058230027,-2.61855746333921,
35.674224217415));
#34143=CARTESIAN_POINT('Ctrl Pts',(-3.01172578200672,-2.53208009686771,
35.6683603537365));
#34144=CARTESIAN_POINT('Ctrl Pts',(-3.08498833944942,-2.44227510737343,
35.6624964900579));
#34145=CARTESIAN_POINT('Ctrl Pts',(-3.15406847912027,-2.34954059956834,
35.6566326263794));
#34146=CARTESIAN_POINT('Ctrl Pts',(-3.22325052860603,-2.25666928606813,
35.6507601120921));
#34147=CARTESIAN_POINT('Ctrl Pts',(-3.28823761480356,-2.16086016971041,
35.6448875978048));
#34148=CARTESIAN_POINT('Ctrl Pts',(-3.34879442180649,-2.06253846521167,
35.6390150835175));
#34149=CARTESIAN_POINT('Ctrl Pts',(-3.36553102499484,-2.0353644539908,35.6373920464683));
#34150=CARTESIAN_POINT('Ctrl Pts',(-3.38192949838553,-2.00799864908361,
35.6357690094191));
#34151=CARTESIAN_POINT('Ctrl Pts',(-3.39798551695636,-1.9804503090345,35.63414597237));
#34152=CARTESIAN_POINT('Ctrl Pts',(-3.45607595395473,-1.88078082341616,
35.6282738484039));
#34153=CARTESIAN_POINT('Ctrl Pts',(-3.50987481252454,-1.77838621886318,
35.6224017244377));
#34154=CARTESIAN_POINT('Ctrl Pts',(-3.55911646351883,-1.67367230935725,
35.6165296004716));
#34155=CARTESIAN_POINT('Ctrl Pts',(-3.60829427173484,-1.56909416351423,
35.6106650898308));
#34156=CARTESIAN_POINT('Ctrl Pts',(-3.65292644795823,-1.46220306325422,
35.60480057919));
#34157=CARTESIAN_POINT('Ctrl Pts',(-3.69279180769145,-1.35343181026859,
35.5989360685492));
#34158=CARTESIAN_POINT('Ctrl Pts',(-3.73261614636621,-1.24477248181989,
35.5930775924314));
#34159=CARTESIAN_POINT('Ctrl Pts',(-3.76768328343449,-1.13423723459942,
35.5872191163137));
#34160=CARTESIAN_POINT('Ctrl Pts',(-3.79781924895605,-1.02228075999645,
35.581360640196));
#34161=CARTESIAN_POINT('Ctrl Pts',(-3.82914351551647,-0.905909693301426,
35.5752711566048));
#34162=CARTESIAN_POINT('Ctrl Pts',(-3.8551395311012,-0.788003423404034,
35.5691816730135));
#34163=CARTESIAN_POINT('Ctrl Pts',(-3.87566820456159,-0.669092645416404,
35.5630921894223));
#34164=CARTESIAN_POINT('Ctrl Pts',(-3.89539521735587,-0.554825425799626,
35.5572405049018));
#34165=CARTESIAN_POINT('Ctrl Pts',(-3.91007380593832,-0.439631125272265,
35.5513888203813));
#34166=CARTESIAN_POINT('Ctrl Pts',(-3.91963237582199,-0.323992343131811,
35.5455371358608));
#34167=CARTESIAN_POINT('Ctrl Pts',(-3.92918948781598,-0.208371198419347,
35.5396863438494));
#34168=CARTESIAN_POINT('Ctrl Pts',(-3.93362809976647,-0.0923061187816158,
35.533835551838));
#34169=CARTESIAN_POINT('Ctrl Pts',(-3.93292850011839,0.0237152473421576,
35.5279847598265));
#34170=CARTESIAN_POINT('Ctrl Pts',(-3.93222883772426,0.139747019249488,
35.5221334430663));
#34171=CARTESIAN_POINT('Ctrl Pts',(-3.92639005011987,0.255734656419345,
35.5162821263061));
#34172=CARTESIAN_POINT('Ctrl Pts',(-3.91544454946725,0.371191298452989,
35.5104308095458));
#34173=CARTESIAN_POINT('Ctrl Pts',(-3.90449541601719,0.486686260396046,
35.5045775507412));
#34174=CARTESIAN_POINT('Ctrl Pts',(-3.88843623829481,0.601649465418135,
35.4987242919365));
#34175=CARTESIAN_POINT('Ctrl Pts',(-3.86735112002908,0.715600666859522,
35.4928710331318));
#34176=CARTESIAN_POINT('Ctrl Pts',(-3.84624201332869,0.829681510018675,
35.4870111151036));
#34177=CARTESIAN_POINT('Ctrl Pts',(-3.82009562839742,0.942747644775464,
35.4811511970754));
#34178=CARTESIAN_POINT('Ctrl Pts',(-3.78904690309602,1.05433038756286,35.4752912790471));
#34179=CARTESIAN_POINT('Ctrl Pts',(-3.75797727179921,1.16598826220463,35.4694274153684));
#34180=CARTESIAN_POINT('Ctrl Pts',(-3.72199885544546,1.27616036402106,35.4635635516896));
#34181=CARTESIAN_POINT('Ctrl Pts',(-3.68129545992388,1.38439616322202,35.4576996880109));
#34182=CARTESIAN_POINT('Ctrl Pts',(-3.64053201710782,1.49279163624931,35.4518271737234));
#34183=CARTESIAN_POINT('Ctrl Pts',(-3.59502984521864,1.59924472687513,35.4459546594359));
#34184=CARTESIAN_POINT('Ctrl Pts',(-3.54501958528189,1.7033276666478,35.4400821451484));
#34185=CARTESIAN_POINT('Ctrl Pts',(-3.53119782161342,1.73209395974999,35.4384591081011));
#34186=CARTESIAN_POINT('Ctrl Pts',(-3.51703196704843,1.76067937158613,35.4368360710538));
#34187=CARTESIAN_POINT('Ctrl Pts',(-3.50252747509735,1.78907526006822,35.4352130340065));
#34188=CARTESIAN_POINT('Ctrl Pts',(-3.45005043833285,1.89181116346021,35.4293409100405));
#34189=CARTESIAN_POINT('Ctrl Pts',(-3.39296142786934,1.99240846515638,35.4234687860746));
#34190=CARTESIAN_POINT('Ctrl Pts',(-3.331458380452,2.09042437302002,35.4175966621086));
#34191=CARTESIAN_POINT('Ctrl Pts',(-3.27003507295682,2.18831320131295,35.4117321514679));
#34192=CARTESIAN_POINT('Ctrl Pts',(-3.20420932695427,2.28362694445509,35.4058676408272));
#34193=CARTESIAN_POINT('Ctrl Pts',(-3.13422580334255,2.37594562514839,35.4000031301866));
#34194=CARTESIAN_POINT('Ctrl Pts',(-3.06431429208025,2.46816931083786,35.394144654069));
#34195=CARTESIAN_POINT('Ctrl Pts',(-2.99025376121517,2.5574037366363,35.3882861779514));
#34196=CARTESIAN_POINT('Ctrl Pts',(-2.91233280283166,2.64325682549969,35.3824277018339));
#34197=CARTESIAN_POINT('Ctrl Pts',(-2.83133931784156,2.73249521538173,35.3763382182426));
#34198=CARTESIAN_POINT('Ctrl Pts',(-2.74617494034244,2.81807973566952,35.3702487346513));
#34199=CARTESIAN_POINT('Ctrl Pts',(-2.65721106180506,2.89960658935326,35.36415925106));
#34200=CARTESIAN_POINT('Ctrl Pts',(-2.57172129192485,2.97794975598523,35.3583075665397));
#34201=CARTESIAN_POINT('Ctrl Pts',(-2.48272353281795,3.05254591346051,35.3524558820193));
#34202=CARTESIAN_POINT('Ctrl Pts',(-2.39058517779383,3.12307404774726,35.346604197499));
#34203=CARTESIAN_POINT('Ctrl Pts',(-2.29846087587175,3.19359142496039,35.3407534054877));
#34204=CARTESIAN_POINT('Ctrl Pts',(-2.20319725864039,3.26004176144352,35.3349026134764));
#34205=CARTESIAN_POINT('Ctrl Pts',(-2.10519400279285,3.32214497134081,35.3290518214652));
#34206=CARTESIAN_POINT('Ctrl Pts',(-2.00718195717924,3.38425375118251,35.3232005047051));
#34207=CARTESIAN_POINT('Ctrl Pts',(-1.90643013371653,3.44201440808012,35.317349187945));
#34208=CARTESIAN_POINT('Ctrl Pts',(-1.80336571094006,3.49519114106877,35.3114978711849));
#34209=CARTESIAN_POINT('Ctrl Pts',(-1.70026708121687,3.54838552334535,35.3056446123805));
#34210=CARTESIAN_POINT('Ctrl Pts',(-1.59485469315812,3.59699276705317,35.2997913535761));
#34211=CARTESIAN_POINT('Ctrl Pts',(-1.48757809164367,3.64082414039209,35.2939380947716));
#34212=CARTESIAN_POINT('Ctrl Pts',(-1.38017944206958,3.68470538046795,35.2880781767436));
#34213=CARTESIAN_POINT('Ctrl Pts',(-1.27091272869601,3.72379974862621,35.2822182587155));
#34214=CARTESIAN_POINT('Ctrl Pts',(-1.16024523484106,3.75796753512169,35.2763583406874));
#34215=CARTESIAN_POINT('Ctrl Pts',(-1.04950322539493,3.79215832776579,35.2704944770088));
#34216=CARTESIAN_POINT('Ctrl Pts',(-0.937358956447254,3.82141582942803,
35.2646306133302));
#34217=CARTESIAN_POINT('Ctrl Pts',(-0.824290841697528,3.84565125931793,
35.2587667496516));
#34218=CARTESIAN_POINT('Ctrl Pts',(-0.711055924294302,3.86992244229369,
35.2528942353643));
#34219=CARTESIAN_POINT('Ctrl Pts',(-0.596894847145015,3.88915669855326,
35.2470217210769));
#34220=CARTESIAN_POINT('Ctrl Pts',(-0.482292178867151,3.90331695538597,
35.2411492067896));
#34221=CARTESIAN_POINT('Ctrl Pts',(-0.450618458309539,3.90723054679429,
35.2395261697408));
#34222=CARTESIAN_POINT('Ctrl Pts',(-0.418911010076204,3.9107568669515,35.237903132692));
#34223=CARTESIAN_POINT('Ctrl Pts',(-0.387180052773377,3.91389583493664,
35.2362800956432));
#34224=CARTESIAN_POINT('Ctrl Pts',(-0.272377919957184,3.92525257454261,
35.2304079716771));
#34225=CARTESIAN_POINT('Ctrl Pts',(-0.156883226493117,3.93157301805287,
35.2245358477111));
#34226=CARTESIAN_POINT('Ctrl Pts',(-0.0411755108716569,3.93278445599355,
35.2186637237451));
#34227=CARTESIAN_POINT('Ctrl Pts',(0.0743821873989408,3.93399432328088,
35.2127992131043));
#34228=CARTESIAN_POINT('Ctrl Pts',(0.190151949021274,3.93010835329838,35.2069347024636));
#34229=CARTESIAN_POINT('Ctrl Pts',(0.305648185573892,3.92110548017461,35.2010701918229));
#34230=CARTESIAN_POINT('Ctrl Pts',(0.421025577648185,3.91211187091772,35.1952117157053));
#34231=CARTESIAN_POINT('Ctrl Pts',(0.536129594798608,3.89801186327134,35.1893532395877));
#34232=CARTESIAN_POINT('Ctrl Pts',(0.650474386927192,3.87883643274007,35.18349476347));
#34233=CARTESIAN_POINT('Ctrl Pts',(0.769327945674279,3.85890488958255,35.1774052798788));
#34234=CARTESIAN_POINT('Ctrl Pts',(0.887360718078619,3.83348942291053,35.1713157962875));
#34235=CARTESIAN_POINT('Ctrl Pts',(1.00403225191212,3.80268434623757,35.1652263126963));
#34236=CARTESIAN_POINT('Ctrl Pts',(1.11614767159814,3.77308223176998,35.1593746281758));
#34237=CARTESIAN_POINT('Ctrl Pts',(1.22700573513248,3.73850366057662,35.1535229436554));
#34238=CARTESIAN_POINT('Ctrl Pts',(1.33613780774355,3.69908431354548,35.147671259135));
#34239=CARTESIAN_POINT('Ctrl Pts',(1.44525323534139,3.65967097882162,35.1418204671237));
#34240=CARTESIAN_POINT('Ctrl Pts',(1.55264280672405,3.61541847668629,35.1359696751124));
#34241=CARTESIAN_POINT('Ctrl Pts',(1.65785488154545,3.56651176806357,35.1301188831011));
#34242=CARTESIAN_POINT('Ctrl Pts',(1.76307639268116,3.51760067307098,35.1242675663409));
#34243=CARTESIAN_POINT('Ctrl Pts',(1.86611964411228,3.46403471605469,35.1184162495808));
#34244=CARTESIAN_POINT('Ctrl Pts',(1.9665553980936,3.40604592837926,35.1125649328206));
#34245=CARTESIAN_POINT('Ctrl Pts',(2.06702448656943,3.34803789430154,35.1067116740162));
#34246=CARTESIAN_POINT('Ctrl Pts',(2.16488399892109,3.2856043172812,35.1008584152117));
#34247=CARTESIAN_POINT('Ctrl Pts',(2.25973221776311,3.21902148237682,35.0950051564072));
#34248=CARTESIAN_POINT('Ctrl Pts',(2.3546883449552,3.15236289651005,35.0891452383791));
#34249=CARTESIAN_POINT('Ctrl Pts',(2.44662600199909,3.08154586825707,35.083285320351));
#34250=CARTESIAN_POINT('Ctrl Pts',(2.53517513579125,3.00688809749645,35.0774254023229));
#34251=CARTESIAN_POINT('Ctrl Pts',(2.62378389224925,2.93218005752225,35.0715615386443));
#34252=CARTESIAN_POINT('Ctrl Pts',(2.70899927913914,2.85362640516566,35.0656976749657));
#34253=CARTESIAN_POINT('Ctrl Pts',(2.79048808283301,2.77158172521883,35.0598338112871));
#34254=CARTESIAN_POINT('Ctrl Pts',(2.87209710210487,2.68941600964288,35.0539612969997));
#34255=CARTESIAN_POINT('Ctrl Pts',(2.94996828894416,2.60374929259215,35.0480887827123));
#34256=CARTESIAN_POINT('Ctrl Pts',(3.02380861326748,2.51496927820786,35.0422162684249));
#34257=CARTESIAN_POINT('Ctrl Pts',(3.04421649585024,2.49043238558377,35.0405932313765));
#34258=CARTESIAN_POINT('Ctrl Pts',(3.06431673688228,2.46565785194012,35.0389701943281));
#34259=CARTESIAN_POINT('Ctrl Pts',(3.08410374667262,2.44065423191403,35.0373471572797));
#34260=CARTESIAN_POINT('Ctrl Pts',(3.15563766634446,2.35026124351392,35.0314795601503));
#34261=CARTESIAN_POINT('Ctrl Pts',(3.2233192179815,2.25656266143007,35.0256119630209));
#34262=CARTESIAN_POINT('Ctrl Pts',(3.2868267905791,2.15992098205734,35.0197443658915));
#34263=CARTESIAN_POINT('Ctrl Pts',(3.35024046023304,2.06342219805599,35.013885444651));
#34264=CARTESIAN_POINT('Ctrl Pts',(3.40949220357858,1.96398931682529,35.0080265234105));
#34265=CARTESIAN_POINT('Ctrl Pts',(3.46430055068524,1.86201790929141,35.00216760217));
#34266=CARTESIAN_POINT('Ctrl Pts',(3.47105962727098,1.84944258838753,35.0014450681133));
#34267=CARTESIAN_POINT('Ctrl Pts',(3.47775117867621,1.83682870064933,35.0007225340567));
#34268=CARTESIAN_POINT('Ctrl Pts',(3.48437472100057,1.8241770209199,35.));
#34269=CARTESIAN_POINT('Origin',(0.,0.,4.68922655072688));
#34270=CARTESIAN_POINT('',(-1.47525540431025,-2.86526422072265,37.4085260041042));
#34271=CARTESIAN_POINT('',(-1.47642197926485,-2.86757701908443,37.6538374878572));
#34272=CARTESIAN_POINT('',(-1.47525540501186,-2.86526422036142,4.68922655072688));
#34273=CARTESIAN_POINT('',(3.0778063018882,-0.968536646922758,38.0000000000001));
#34274=CARTESIAN_POINT('Ctrl Pts',(-1.47642197926477,-2.86757701908447,
37.6538374878573));
#34275=CARTESIAN_POINT('Ctrl Pts',(-0.665155101486716,-3.27567489825073,
37.7100277566941));
#34276=CARTESIAN_POINT('Ctrl Pts',(1.38130508422518,-3.40042127156339,37.8254152607417));
#34277=CARTESIAN_POINT('Ctrl Pts',(2.78385737807687,-1.87794914020384,37.9408027647893));
#34278=CARTESIAN_POINT('Ctrl Pts',(3.0778063018882,-0.968536646922758,38.0000000000001));
#34279=CARTESIAN_POINT('',(1.92911062273198,2.58159829713351,37.9999969413403));
#34280=CARTESIAN_POINT('Origin',(0.,0.,38.));
#34281=CARTESIAN_POINT('',(3.22274953375635,0.00173354353987881,37.8165056021994));
#34282=CARTESIAN_POINT('Ctrl Pts',(3.222749531205,0.00173828016955539,37.8165059165414));
#34283=CARTESIAN_POINT('Ctrl Pts',(3.22270305071438,0.0879125241068303,
37.8222247873387));
#34284=CARTESIAN_POINT('Ctrl Pts',(3.21920019789002,0.174060452734954,37.8278510718186));
#34285=CARTESIAN_POINT('Ctrl Pts',(3.2114797988416,0.269454144514142,37.8339081349421));
#34286=CARTESIAN_POINT('Ctrl Pts',(3.21067053001022,0.278931510071132,37.8345079924864));
#34287=CARTESIAN_POINT('Ctrl Pts',(3.2092464328258,0.294781062059853,37.8355078136478));
#34288=CARTESIAN_POINT('Ctrl Pts',(3.20865456251314,0.301155178058178,37.835908996707));
#34289=CARTESIAN_POINT('Ctrl Pts',(3.20754096814088,0.312771891365883,37.8366384362922));
#34290=CARTESIAN_POINT('Ctrl Pts',(3.2070253751692,0.318015034703768,37.836967029785));
#34291=CARTESIAN_POINT('Ctrl Pts',(3.20593683907471,0.328812599313765,37.8376423829336));
#34292=CARTESIAN_POINT('Ctrl Pts',(3.20536232519363,0.334366724584944,37.8379890372753));
#34293=CARTESIAN_POINT('Ctrl Pts',(3.20402360875131,0.346988193085497,37.8387751375784));
#34294=CARTESIAN_POINT('Ctrl Pts',(3.20325045895787,0.354054502934622,37.8392140737816));
#34295=CARTESIAN_POINT('Ctrl Pts',(3.20118373404302,0.372382545982474,37.8403496410081));
#34296=CARTESIAN_POINT('Ctrl Pts',(3.19985409722441,0.383640228532662,37.8410442892656));
#34297=CARTESIAN_POINT('Ctrl Pts',(3.19108503739539,0.454666263385874,37.8454102006503));
#34298=CARTESIAN_POINT('Ctrl Pts',(3.1820302095878,0.514227520546008,37.8489966822654));
#34299=CARTESIAN_POINT('Ctrl Pts',(3.16366679900411,0.615771813209107,37.8550362213012));
#34300=CARTESIAN_POINT('Ctrl Pts',(3.1551785212053,0.657883962557299,37.8575185671406));
#34301=CARTESIAN_POINT('Ctrl Pts',(3.09705571057058,0.919161018413947,37.8728485623131));
#34302=CARTESIAN_POINT('Ctrl Pts',(3.02545318345635,1.13280770928991,37.8851126266627));
#34303=CARTESIAN_POINT('Ctrl Pts',(2.89150874849534,1.42650354757404,37.9034389615986));
#34304=CARTESIAN_POINT('Ctrl Pts',(2.84676610907895,1.51382154709284,37.9090837800931));
#34305=CARTESIAN_POINT('Ctrl Pts',(2.76897445235689,1.64995383043231,37.9183162286303));
#34306=CARTESIAN_POINT('Ctrl Pts',(2.73844702740723,1.70013951790317,37.9218187002717));
#34307=CARTESIAN_POINT('Ctrl Pts',(2.69709104329107,1.76412079276401,37.9264275422393));
#34308=CARTESIAN_POINT('Ctrl Pts',(2.68749641232533,1.7787032586588,37.927487903642));
#34309=CARTESIAN_POINT('Ctrl Pts',(2.67171291233598,1.80227265496957,37.9292182942922));
#34310=CARTESIAN_POINT('Ctrl Pts',(2.66559595145052,1.81130749122718,37.9298856027177));
#34311=CARTESIAN_POINT('Ctrl Pts',(2.65375232712182,1.82861075903095,37.9311714103812));
#34312=CARTESIAN_POINT('Ctrl Pts',(2.64803259611736,1.83688379817252,37.9317896403862));
#34313=CARTESIAN_POINT('Ctrl Pts',(2.63485785912359,1.85575036666307,37.9332075188928));
#34314=CARTESIAN_POINT('Ctrl Pts',(2.62737755804495,1.86632594172695,37.9340081330577));
#34315=CARTESIAN_POINT('Ctrl Pts',(2.60735435208714,1.89427559330572,37.9361397271336));
#34316=CARTESIAN_POINT('Ctrl Pts',(2.59470173952829,1.91156992752261,37.9374749398502));
#34317=CARTESIAN_POINT('Ctrl Pts',(2.49592050226965,2.04380213864549,37.9478116764587));
#34318=CARTESIAN_POINT('Ctrl Pts',(2.402379485937,2.15297679446978,37.9571075650017));
#34319=CARTESIAN_POINT('Ctrl Pts',(2.18612439940587,2.3736751443618,37.9775951997114));
#34320=CARTESIAN_POINT('Ctrl Pts',(2.06149009590583,2.48267715660793,37.988830446671));
#34321=CARTESIAN_POINT('Ctrl Pts',(1.92911062273198,2.58159829713351,37.9999969413403));
#34322=CARTESIAN_POINT('Ctrl Pts',(-1.47525540431025,-2.86526422072265,
37.4085260041042));
#34323=CARTESIAN_POINT('Ctrl Pts',(-1.43625760423782,-2.88534324690704,
37.4114783217196));
#34324=CARTESIAN_POINT('Ctrl Pts',(-1.39683575020098,-2.90463337997842,
37.4144193805815));
#34325=CARTESIAN_POINT('Ctrl Pts',(-1.27393816816533,-2.96168666266681,
37.4234325092417));
#34326=CARTESIAN_POINT('Ctrl Pts',(-1.1892482247323,-2.9966979124969,37.429427020127));
#34327=CARTESIAN_POINT('Ctrl Pts',(-1.09009691860782,-3.03282046492186,
37.4361111154649));
#34328=CARTESIAN_POINT('Ctrl Pts',(-1.0769890306239,-3.03749994383052,37.4369881523242));
#34329=CARTESIAN_POINT('Ctrl Pts',(-1.05717493303045,-3.04442913262363,
37.4383035141713));
#34330=CARTESIAN_POINT('Ctrl Pts',(-1.05049115905415,-3.04674185148841,
37.4387454441221));
#34331=CARTESIAN_POINT('Ctrl Pts',(-1.03851967456026,-3.05084014569193,
37.4395337580483));
#34332=CARTESIAN_POINT('Ctrl Pts',(-1.03323490810244,-3.05263399955876,
37.4398806263606));
#34333=CARTESIAN_POINT('Ctrl Pts',(-1.02177956153736,-3.05648923004023,
37.4406300496742));
#34334=CARTESIAN_POINT('Ctrl Pts',(-1.01560741011654,-3.0585456472008,37.4410323099559));
#34335=CARTESIAN_POINT('Ctrl Pts',(-0.998341982499454,-3.06424005945056,
37.4421533973977));
#34336=CARTESIAN_POINT('Ctrl Pts',(-0.987234969882515,-3.0678365308348,
37.4428698150333));
#34337=CARTESIAN_POINT('Ctrl Pts',(-0.92237377082824,-3.08844997402597,
37.4470269220475));
#34338=CARTESIAN_POINT('Ctrl Pts',(-0.868196327896372,-3.10411543744507,
37.4503933551825));
#34339=CARTESIAN_POINT('Ctrl Pts',(-0.567968942834488,-3.18244995353801,
37.4686115598272));
#34340=CARTESIAN_POINT('Ctrl Pts',(-0.315569757793848,-3.21730000377383,
37.4823896948693));
#34341=CARTESIAN_POINT('Ctrl Pts',(0.102172048858668,-3.22529598914287,
37.505990032542));
#34342=CARTESIAN_POINT('Ctrl Pts',(0.265998739668756,-3.21593028080837,
37.5154334030571));
#34343=CARTESIAN_POINT('Ctrl Pts',(0.450099879470417,-3.19123917122849,
37.5266056965123));
#34344=CARTESIAN_POINT('Ctrl Pts',(0.47177886739132,-3.18810633660193,37.5279298974547));
#34345=CARTESIAN_POINT('Ctrl Pts',(0.506362463765492,-3.1827481905488,37.530056797019));
#34346=CARTESIAN_POINT('Ctrl Pts',(0.519288604395263,-3.18066476173729,
37.5308549945278));
#34347=CARTESIAN_POINT('Ctrl Pts',(0.542142228265927,-3.17683820086012,
37.5322720981139));
#34348=CARTESIAN_POINT('Ctrl Pts',(0.552074959888118,-3.17512714471595,
37.5328899751805));
#34349=CARTESIAN_POINT('Ctrl Pts',(0.572681199104011,-3.17147780788289,
37.534175972722));
#34350=CARTESIAN_POINT('Ctrl Pts',(0.58335325957357,-3.16953217551716,37.5348443208466));
#34351=CARTESIAN_POINT('Ctrl Pts',(0.610891962848549,-3.16436777485636,
37.5365750642616));
#34352=CARTESIAN_POINT('Ctrl Pts',(0.627742901766128,-3.16106805300211,
37.5376400362361));
#34353=CARTESIAN_POINT('Ctrl Pts',(0.699516743483176,-3.14641689040722,
37.5422019819395));
#34354=CARTESIAN_POINT('Ctrl Pts',(0.754161905297265,-3.1337680363353,37.5457402667464));
#34355=CARTESIAN_POINT('Ctrl Pts',(0.897409856562916,-3.09664642239335,
37.555194229315));
#34356=CARTESIAN_POINT('Ctrl Pts',(0.98533890770676,-3.06979937999765,37.5611815026519));
#34357=CARTESIAN_POINT('Ctrl Pts',(1.2095339777098,-2.99072159863251,37.5769081150617));
#34358=CARTESIAN_POINT('Ctrl Pts',(1.34361342306006,-2.93293127891763,37.5867751799219));
#34359=CARTESIAN_POINT('Ctrl Pts',(1.64055446299926,-2.78029852200403,37.6093749174947));
#34360=CARTESIAN_POINT('Ctrl Pts',(1.79997494065692,-2.67984805879226,37.6220741106077));
#34361=CARTESIAN_POINT('Ctrl Pts',(1.9613994561847,-2.55719460177184,37.6349237909817));
#34362=CARTESIAN_POINT('Ctrl Pts',(1.97300052435852,-2.54825450221348,37.6358470784723));
#34363=CARTESIAN_POINT('Ctrl Pts',(1.99015393674327,-2.53484824568232,37.6372114851217));
#34364=CARTESIAN_POINT('Ctrl Pts',(1.99575287536791,-2.53044240862144,37.637656708983));
#34365=CARTESIAN_POINT('Ctrl Pts',(2.00571489348871,-2.5225496074878,37.6384485903369));
#34366=CARTESIAN_POINT('Ctrl Pts',(2.01008355105668,-2.51906984333524,37.6387957505675));
#34367=CARTESIAN_POINT('Ctrl Pts',(2.01446052691476,-2.51556481699289,37.6391434612459));
#34368=CARTESIAN_POINT('Ctrl Pts',(2.01447780796669,-2.51555097825504,37.6391448340657));
#34369=CARTESIAN_POINT('Ctrl Pts',(2.01451209387071,-2.51552352138144,37.6391475577606));
#34370=CARTESIAN_POINT('Ctrl Pts',(2.01452909869127,-2.5155099032802,37.6391489086332));
#34371=CARTESIAN_POINT('Ctrl Pts',(2.0145628373658,-2.51548288351646,37.6391515888495));
#34372=CARTESIAN_POINT('Ctrl Pts',(2.01457957132563,-2.51546948177812,37.6391529182017));
#34373=CARTESIAN_POINT('Ctrl Pts',(2.01461277389525,-2.51544289026868,37.6391555558235));
#34374=CARTESIAN_POINT('Ctrl Pts',(2.01462924241462,-2.51542970057863,37.639156864086));
#34375=CARTESIAN_POINT('Ctrl Pts',(2.0146619193043,-2.51540352902598,37.6391594599418));
#34376=CARTESIAN_POINT('Ctrl Pts',(2.01467812761216,-2.51539054722172,37.6391607475302));
#34377=CARTESIAN_POINT('Ctrl Pts',(2.01471028907978,-2.51536478746003,37.6391633024351));
#34378=CARTESIAN_POINT('Ctrl Pts',(2.01472624225204,-2.51535200950061,37.6391645697527));
#34379=CARTESIAN_POINT('Ctrl Pts',(2.01972807099056,-2.51134563322859,37.6395619138407));
#34380=CARTESIAN_POINT('Ctrl Pts',(2.02470211271556,-2.50733717850673,37.6399569153863));
#34381=CARTESIAN_POINT('Ctrl Pts',(2.03827249452963,-2.49633443583687,37.6410343068212));
#34382=CARTESIAN_POINT('Ctrl Pts',(2.04684482313504,-2.48931047799182,37.6417145931564));
#34383=CARTESIAN_POINT('Ctrl Pts',(2.06606395237776,-2.47339638665036,37.6432395665484));
#34384=CARTESIAN_POINT('Ctrl Pts',(2.07669000471623,-2.4644814019076,37.6440825502383));
#34385=CARTESIAN_POINT('Ctrl Pts',(2.10951810837679,-2.43657637541224,37.6466875629647));
#34386=CARTESIAN_POINT('Ctrl Pts',(2.13152033616147,-2.41735232524608,37.6484345170127));
#34387=CARTESIAN_POINT('Ctrl Pts',(2.21662868366218,-2.34092479432583,37.6552100180404));
#34388=CARTESIAN_POINT('Ctrl Pts',(2.277722411028,-2.28152455949615,37.6601136487935));
#34389=CARTESIAN_POINT('Ctrl Pts',(2.47910493352838,-2.06956152673026,37.6767133184336));
#34390=CARTESIAN_POINT('Ctrl Pts',(2.60699792545665,-1.90594121404209,37.6880679711775));
#34391=CARTESIAN_POINT('Ctrl Pts',(2.79364918059233,-1.61285988383586,37.7078258502478));
#34392=CARTESIAN_POINT('Ctrl Pts',(2.86118440054439,-1.48976823541654,37.7159683100511));
#34393=CARTESIAN_POINT('Ctrl Pts',(2.92950456987935,-1.3433449777783,37.7256914787533));
#34394=CARTESIAN_POINT('Ctrl Pts',(2.93833337958235,-1.32392207894861,37.7269817553788));
#34395=CARTESIAN_POINT('Ctrl Pts',(2.95220046439086,-1.29259315699834,37.7290644168006));
#34396=CARTESIAN_POINT('Ctrl Pts',(2.9573611778658,-1.28074178017141,37.7298525949595));
#34397=CARTESIAN_POINT('Ctrl Pts',(2.96640875182672,-1.25961809982176,37.7312581549325));
#34398=CARTESIAN_POINT('Ctrl Pts',(2.97032380494049,-1.25035800092514,37.7318745637));
#34399=CARTESIAN_POINT('Ctrl Pts',(2.97840216178564,-1.23099855951164,37.7331638276924));
#34400=CARTESIAN_POINT('Ctrl Pts',(2.98255756835005,-1.22089607977979,37.7338369421164));
#34401=CARTESIAN_POINT('Ctrl Pts',(2.99324152136314,-1.19454154661972,37.7355938605544));
#34402=CARTESIAN_POINT('Ctrl Pts',(2.9996890194264,-1.17825722107829,37.7366803906561));
#34403=CARTESIAN_POINT('Ctrl Pts',(3.02738045597171,-1.10661678915694,37.7414651034141));
#34404=CARTESIAN_POINT('Ctrl Pts',(3.04722600175411,-1.05073597301318,37.745209778755));
#34405=CARTESIAN_POINT('Ctrl Pts',(3.09618601212435,-0.899794217254751,
37.7553646995311));
#34406=CARTESIAN_POINT('Ctrl Pts',(3.12246079401988,-0.803886135467158,
37.7618604483947));
#34407=CARTESIAN_POINT('Ctrl Pts',(3.19655906508416,-0.474311713053508,
37.7842838470966));
#34408=CARTESIAN_POINT('Ctrl Pts',(3.22287775861272,-0.236643276283802,
37.8006859445876));
#34409=CARTESIAN_POINT('Ctrl Pts',(3.22274953375635,0.00173354353987881,
37.8165056021994));
#34410=CARTESIAN_POINT('Origin',(0.,0.,4.68922655072688));
#34411=CARTESIAN_POINT('',(-1.47525533429856,-2.86526425676998,36.1542047394732));
#34412=CARTESIAN_POINT('',(-1.47525545662511,-2.865264193787,36.4017031386693));
#34413=CARTESIAN_POINT('',(-1.47525540501186,-2.86526422036142,4.68922655072688));
#34414=CARTESIAN_POINT('',(3.22710931890567,0.00161487490920624,36.8107734492731));
#34415=CARTESIAN_POINT('Ctrl Pts',(3.22274952067548,0.00175769336351857,
36.8082682062519));
#34416=CARTESIAN_POINT('Ctrl Pts',(3.22276605484594,-0.0285578844381251,
36.80650283569));
#34417=CARTESIAN_POINT('Ctrl Pts',(3.22235483219543,-0.05887312616645,36.8047522247304));
#34418=CARTESIAN_POINT('Ctrl Pts',(3.21327137318411,-0.387005561556071,
36.7859214086916));
#34419=CARTESIAN_POINT('Ctrl Pts',(3.16376992247395,-0.68224905193963,36.7698842931772));
#34420=CARTESIAN_POINT('Ctrl Pts',(3.04938585646319,-1.04609995332455,36.7476979918744));
#34421=CARTESIAN_POINT('Ctrl Pts',(3.02128342954484,-1.1246883395346,36.742763256182));
#34422=CARTESIAN_POINT('Ctrl Pts',(2.98285032186027,-1.22028936190716,36.7365420512188));
#34423=CARTESIAN_POINT('Ctrl Pts',(2.9753694133729,-1.23841794118675,36.7353524918587));
#34424=CARTESIAN_POINT('Ctrl Pts',(2.96328290429647,-1.266965558166,36.7334631611481));
#34425=CARTESIAN_POINT('Ctrl Pts',(2.95878664247503,-1.27743058344845,36.7327671204464));
#34426=CARTESIAN_POINT('Ctrl Pts',(2.95025209269912,-1.2970078992249,36.7314584368492));
#34427=CARTESIAN_POINT('Ctrl Pts',(2.94622681528071,-1.30612574068935,36.7308462461957));
#34428=CARTESIAN_POINT('Ctrl Pts',(2.93712178009111,-1.32649371637484,36.7294725934711));
#34429=CARTESIAN_POINT('Ctrl Pts',(2.93201957254121,-1.33773358711513,36.7287103643352));
#34430=CARTESIAN_POINT('Ctrl Pts',(2.91892192023341,-1.36615204620692,36.7267723867528));
#34431=CARTESIAN_POINT('Ctrl Pts',(2.91083939729689,-1.38328976290622,36.7255936367331));
#34432=CARTESIAN_POINT('Ctrl Pts',(2.86351639764259,-1.48137920989517,36.7187880237311));
#34433=CARTESIAN_POINT('Ctrl Pts',(2.82105450547159,-1.56072400536159,36.7130492195396));
#34434=CARTESIAN_POINT('Ctrl Pts',(2.63326649012482,-1.87886563895286,36.6890430908086));
#34435=CARTESIAN_POINT('Ctrl Pts',(2.46050134454939,-2.10002863479042,36.669822646677));
#34436=CARTESIAN_POINT('Ctrl Pts',(2.20945924073325,-2.34728117032595,36.6462732745994));
#34437=CARTESIAN_POINT('Ctrl Pts',(2.1557594856927,-2.39669386755196,36.6414506258617));
#34438=CARTESIAN_POINT('Ctrl Pts',(2.0804396760161,-2.46141884193578,36.6350203875209));
#34439=CARTESIAN_POINT('Ctrl Pts',(2.0602432364287,-2.47834821289421,36.6333272889481));
#34440=CARTESIAN_POINT('Ctrl Pts',(2.02986562523331,-2.50318379611761,36.6308294108307));
#34441=CARTESIAN_POINT('Ctrl Pts',(2.01984151149068,-2.51127932629666,36.6300128964112));
#34442=CARTESIAN_POINT('Ctrl Pts',(2.00160723725369,-2.52582561469292,36.6285419920877));
#34443=CARTESIAN_POINT('Ctrl Pts',(1.99341382175586,-2.5322969633083,36.6278862401827));
#34444=CARTESIAN_POINT('Ctrl Pts',(1.98027247466594,-2.54257299615543,36.6268429385855));
#34445=CARTESIAN_POINT('Ctrl Pts',(1.97534477213949,-2.54640325703751,36.62645360774));
#34446=CARTESIAN_POINT('Ctrl Pts',(1.96619282674201,-2.5534744324519,36.6257340567563));
#34447=CARTESIAN_POINT('Ctrl Pts',(1.96197172778946,-2.55671915723209,36.6254035717015));
#34448=CARTESIAN_POINT('Ctrl Pts',(1.95207787242992,-2.56428555302981,36.624632163286));
#34449=CARTESIAN_POINT('Ctrl Pts',(1.94639880479212,-2.56859886173743,36.624191832511));
#34450=CARTESIAN_POINT('Ctrl Pts',(1.92899148777409,-2.58172901126351,36.6228494776079));
#34451=CARTESIAN_POINT('Ctrl Pts',(1.91721711122963,-2.59048478375062,36.6219516327591));
#34452=CARTESIAN_POINT('Ctrl Pts',(1.75489781846419,-2.70947723984751,36.6097061108786));
#34453=CARTESIAN_POINT('Ctrl Pts',(1.59509190662659,-2.80653453996464,36.5991877727189));
#34454=CARTESIAN_POINT('Ctrl Pts',(1.2958759370638,-2.95439752107189,36.5805075949685));
#34455=CARTESIAN_POINT('Ctrl Pts',(1.15968358011756,-3.01046368765049,36.5723406741485));
#34456=CARTESIAN_POINT('Ctrl Pts',(0.932892404282599,-3.08614478306714,
36.5587297343269));
#34457=CARTESIAN_POINT('Ctrl Pts',(0.844441674176579,-3.111509952806,36.5534208244709));
#34458=CARTESIAN_POINT('Ctrl Pts',(0.700471980442569,-3.14620505278839,
36.5446884902619));
#34459=CARTESIAN_POINT('Ctrl Pts',(0.645580608867946,-3.15792532051728,
36.5413386643411));
#34460=CARTESIAN_POINT('Ctrl Pts',(0.573525407193728,-3.17135322634818,
36.536903343233));
#34461=CARTESIAN_POINT('Ctrl Pts',(0.556612567602607,-3.17436530833754,
36.5358595874755));
#34462=CARTESIAN_POINT('Ctrl Pts',(0.52897770913344,-3.17905928174248,36.5341494268078));
#34463=CARTESIAN_POINT('Ctrl Pts',(0.518269707133551,-3.18082250993434,
36.5334856213996));
#34464=CARTESIAN_POINT('Ctrl Pts',(0.497596464884699,-3.18411949787508,
36.5322017561688));
#34465=CARTESIAN_POINT('Ctrl Pts',(0.487632518424355,-3.18566064449777,
36.5315819396622));
#34466=CARTESIAN_POINT('Ctrl Pts',(0.464709565415272,-3.18909612670047,
36.5301535621975));
#34467=CARTESIAN_POINT('Ctrl Pts',(0.451745981609123,-3.19095826445369,
36.5293439885043));
#34468=CARTESIAN_POINT('Ctrl Pts',(0.417066885607546,-3.19572413789937,
36.5271733542962));
#34469=CARTESIAN_POINT('Ctrl Pts',(0.395332806374885,-3.19848549887924,
36.5258078129339));
#34470=CARTESIAN_POINT('Ctrl Pts',(0.210804253310464,-3.2200207344675,36.5141683524406));
#34471=CARTESIAN_POINT('Ctrl Pts',(0.0468498156986263,-3.22657130235436,
36.5035071245191));
#34472=CARTESIAN_POINT('Ctrl Pts',(-0.370926724992662,-3.21141096296261,
36.4756243991621));
#34473=CARTESIAN_POINT('Ctrl Pts',(-0.622986109466305,-3.17216495732823,
36.4580755360971));
#34474=CARTESIAN_POINT('Ctrl Pts',(-0.921844436026495,-3.08860298168915,
36.4377768145144));
#34475=CARTESIAN_POINT('Ctrl Pts',(-0.975479136866018,-3.07208510679403,
36.4341589201158));
#34476=CARTESIAN_POINT('Ctrl Pts',(-1.03970943635549,-3.05045206800001,
36.4298790289116));
#34477=CARTESIAN_POINT('Ctrl Pts',(-1.05073997555764,-3.04667015687418,
36.4291459310195));
#34478=CARTESIAN_POINT('Ctrl Pts',(-1.06789081565318,-3.04068562500645,
36.4280093161713));
#34479=CARTESIAN_POINT('Ctrl Pts',(-1.07402525303346,-3.03852425066817,
36.4276034256032));
#34480=CARTESIAN_POINT('Ctrl Pts',(-1.0854135811211,-3.03447295164859,36.4268511698193));
#34481=CARTESIAN_POINT('Ctrl Pts',(-1.09066905278063,-3.03258796317373,
36.4265045275812));
#34482=CARTESIAN_POINT('Ctrl Pts',(-1.10257831092685,-3.02828148707774,
36.425720142159));
#34483=CARTESIAN_POINT('Ctrl Pts',(-1.10922901640343,-3.02585172937019,
36.4252828985485));
#34484=CARTESIAN_POINT('Ctrl Pts',(-1.12895768572347,-3.01857030311774,
36.4239880705158));
#34485=CARTESIAN_POINT('Ctrl Pts',(-1.14201241672374,-3.01365555221201,
36.4231341595343));
#34486=CARTESIAN_POINT('Ctrl Pts',(-1.24129942132,-2.9755388743415,36.4166589295455));
#34487=CARTESIAN_POINT('Ctrl Pts',(-1.32610848080994,-2.93872346122117,
36.4112379686349));
#34488=CARTESIAN_POINT('Ctrl Pts',(-1.4313674177628,-2.8875441186618,36.4045101853076));
#34489=CARTESIAN_POINT('Ctrl Pts',(-1.45337870525942,-2.87652800565308,
36.4031033493262));
#34490=CARTESIAN_POINT('Ctrl Pts',(-1.47525545662511,-2.865264193787,36.4017031386693));
#34491=CARTESIAN_POINT('Ctrl Pts',(3.22710931890567,0.00161487490920624,
36.8107734492731));
#34492=CARTESIAN_POINT('Ctrl Pts',(3.22766820945557,0.092902302212634,36.8164301670323));
#34493=CARTESIAN_POINT('Ctrl Pts',(3.18268013141034,1.25374923679401,36.8883978642459));
#34494=CARTESIAN_POINT('Ctrl Pts',(1.77912732379145,3.37157490318388,37.0266765409141));
#34495=CARTESIAN_POINT('Ctrl Pts',(-1.875636683147,3.31885498005365,37.2256094792775));
#34496=CARTESIAN_POINT('Ctrl Pts',(-3.806119388409,0.2150966389413,37.4245424176409));
#34497=CARTESIAN_POINT('Ctrl Pts',(-2.68065523389285,-2.15386545564773,
37.5672850871675));
#34498=CARTESIAN_POINT('Ctrl Pts',(-1.62254331795257,-2.79407246706486,
37.6437167772396));
#34499=CARTESIAN_POINT('Ctrl Pts',(-1.47642197926477,-2.86757701908447,
37.6538374878573));
#34500=CARTESIAN_POINT('Ctrl Pts',(-1.47525533429857,-2.86526425676998,
36.1542047394732));
#34501=CARTESIAN_POINT('Ctrl Pts',(-1.35648519049259,-2.92641613405012,
36.1626885432144));
#34502=CARTESIAN_POINT('Ctrl Pts',(-1.23401696002696,-2.98012972438504,
36.171426215797));
#34503=CARTESIAN_POINT('Ctrl Pts',(-0.871056753745843,-3.11309363011468,
36.1972043428991));
#34504=CARTESIAN_POINT('Ctrl Pts',(-0.62415665607532,-3.17183152281709,
36.2146603565864));
#34505=CARTESIAN_POINT('Ctrl Pts',(-0.315582863209829,-3.20778098899618,
36.2349996513337));
#34506=CARTESIAN_POINT('Ctrl Pts',(-0.258057652374377,-3.21292057905945,
36.2387254237883));
#34507=CARTESIAN_POINT('Ctrl Pts',(-0.188689003787312,-3.21724295097161,
36.2431149691367));
#34508=CARTESIAN_POINT('Ctrl Pts',(-0.176952494959484,-3.21790981388537,
36.2438540833031));
#34509=CARTESIAN_POINT('Ctrl Pts',(-0.158697769992497,-3.21884686376737,
36.2449978860274));
#34510=CARTESIAN_POINT('Ctrl Pts',(-0.152182082262523,-3.21916149489491,
36.2454049970216));
#34511=CARTESIAN_POINT('Ctrl Pts',(-0.140091921436821,-3.21970851840367,
36.2461582237465));
#34512=CARTESIAN_POINT('Ctrl Pts',(-0.134517851565134,-3.21994621667609,
36.246504624429));
#34513=CARTESIAN_POINT('Ctrl Pts',(-0.121899983884943,-3.22045146537396,
36.2472868186752));
#34514=CARTESIAN_POINT('Ctrl Pts',(-0.114855926478386,-3.22071038208709,
36.2477221232154));
#34515=CARTESIAN_POINT('Ctrl Pts',(-0.0940122937803075,-3.2214080568381,
36.2490063209519));
#34516=CARTESIAN_POINT('Ctrl Pts',(-0.0802104780147182,-3.2217812581072,
36.249851628328));
#34517=CARTESIAN_POINT('Ctrl Pts',(0.0221298499941792,-3.22389048050423,
36.2560850492217));
#34518=CARTESIAN_POINT('Ctrl Pts',(0.110712612917276,-3.22206538514645,
36.2612892835029));
#34519=CARTESIAN_POINT('Ctrl Pts',(0.445915510658712,-3.2013154222992,36.2806307746532));
#34520=CARTESIAN_POINT('Ctrl Pts',(0.690145716217482,-3.15768500635991,
36.2940591626006));
#34521=CARTESIAN_POINT('Ctrl Pts',(1.01452756133985,-3.06026212167359,36.3133462070023));
#34522=CARTESIAN_POINT('Ctrl Pts',(1.10089540739617,-3.03026365611643,36.3186227453361));
#34523=CARTESIAN_POINT('Ctrl Pts',(1.23781003456563,-2.97608206240529,36.327306455389));
#34524=CARTESIAN_POINT('Ctrl Pts',(1.28920685994301,-2.95418063542867,36.3306410855843));
#34525=CARTESIAN_POINT('Ctrl Pts',(1.35560046236527,-2.92382608149794,36.3350588579925));
#34526=CARTESIAN_POINT('Ctrl Pts',(1.37113718712766,-2.91657236577657,36.3361006719362));
#34527=CARTESIAN_POINT('Ctrl Pts',(1.39640277016724,-2.90452998414118,36.337808298884));
#34528=CARTESIAN_POINT('Ctrl Pts',(1.40616678114284,-2.89981552936949,36.3384715255641));
#34529=CARTESIAN_POINT('Ctrl Pts',(1.42496266930354,-2.89062287066295,36.3397547264029));
#34530=CARTESIAN_POINT('Ctrl Pts',(1.43399770170545,-2.88615137806843,36.3403744598718));
#34531=CARTESIAN_POINT('Ctrl Pts',(1.45472976009375,-2.87576957325743,36.341803297677));
#34532=CARTESIAN_POINT('Ctrl Pts',(1.46641195118515,-2.86983018568026,36.342613418507));
#34533=CARTESIAN_POINT('Ctrl Pts',(1.49755967260083,-2.85375441088964,36.3447869664951));
#34534=CARTESIAN_POINT('Ctrl Pts',(1.51695816490364,-2.84349030209702,36.3461548952742));
#34535=CARTESIAN_POINT('Ctrl Pts',(1.68083909316897,-2.75462355953177,36.357835068579));
#34536=CARTESIAN_POINT('Ctrl Pts',(1.81919097537173,-2.66527678924624,36.3685375908901));
#34537=CARTESIAN_POINT('Ctrl Pts',(2.15338260351415,-2.41127628278103,36.3965392768757));
#34538=CARTESIAN_POINT('Ctrl Pts',(2.33757028432234,-2.23317501815466,36.4141675774876));
#34539=CARTESIAN_POINT('Ctrl Pts',(2.53323312048606,-1.99294232868106,36.4344160582179));
#34540=CARTESIAN_POINT('Ctrl Pts',(2.56658298813822,-1.94980557244468,36.4379287022976));
#34541=CARTESIAN_POINT('Ctrl Pts',(2.60566044690566,-1.89651913145639,36.4421009236364));
#34542=CARTESIAN_POINT('Ctrl Pts',(2.61244621916695,-1.88716081510612,36.4428275825417));
#34543=CARTESIAN_POINT('Ctrl Pts',(2.62295753273703,-1.87249922315853,36.4439563210097));
#34544=CARTESIAN_POINT('Ctrl Pts',(2.62671759778278,-1.86722098920448,36.4443607233275));
#34545=CARTESIAN_POINT('Ctrl Pts',(2.63368774521397,-1.85737384537279,36.4451115070263));
#34546=CARTESIAN_POINT('Ctrl Pts',(2.63690184234078,-1.85280798122805,36.4454581572087));
#34547=CARTESIAN_POINT('Ctrl Pts',(2.64418024368227,-1.84241116954627,36.4462441981131));
#34548=CARTESIAN_POINT('Ctrl Pts',(2.64823712627546,-1.83657512888788,36.4466830793902));
#34549=CARTESIAN_POINT('Ctrl Pts',(2.65871239544762,-1.82139902013144,36.447818410412));
#34550=CARTESIAN_POINT('Ctrl Pts',(2.66510094696543,-1.81203833942282,36.4485128787553));
#34551=CARTESIAN_POINT('Ctrl Pts',(2.70510337492795,-1.75275647877739,36.4528757988539));
#34552=CARTESIAN_POINT('Ctrl Pts',(2.73736513833007,-1.70193205234039,36.4564596009306));
#34553=CARTESIAN_POINT('Ctrl Pts',(2.93892976009823,-1.36381649689437,36.4794989374551));
#34554=CARTESIAN_POINT('Ctrl Pts',(3.06420210421427,-1.05262467792409,36.4972114672141));
#34555=CARTESIAN_POINT('Ctrl Pts',(3.15914205093584,-0.643036144895613,
36.521630007708));
#34556=CARTESIAN_POINT('Ctrl Pts',(3.17533518873855,-0.557600584126361,
36.526765492885));
#34557=CARTESIAN_POINT('Ctrl Pts',(3.19095975778362,-0.451981742642096,
36.533210627656));
#34558=CARTESIAN_POINT('Ctrl Pts',(3.19368337042743,-0.43231721414448,36.5344146060057));
#34559=CARTESIAN_POINT('Ctrl Pts',(3.19768988748429,-0.401282733161163,
36.5363215020611));
#34560=CARTESIAN_POINT('Ctrl Pts',(3.19909424851081,-0.389928752815022,
36.5370205673367));
#34561=CARTESIAN_POINT('Ctrl Pts',(3.20160785947631,-0.368678505116161,
36.5383317097633));
#34562=CARTESIAN_POINT('Ctrl Pts',(3.20273175667167,-0.358784081663207,
36.5389433152643));
#34563=CARTESIAN_POINT('Ctrl Pts',(3.2051375239809,-0.336691909387495,36.5403114660003));
#34564=CARTESIAN_POINT('Ctrl Pts',(3.20639565045291,-0.324491780416018,
36.5410687525325));
#34565=CARTESIAN_POINT('Ctrl Pts',(3.20939615766952,-0.293672553523231,
36.5429862892245));
#34566=CARTESIAN_POINT('Ctrl Pts',(3.21104615788522,-0.275045112098162,
36.5441494336786));
#34567=CARTESIAN_POINT('Ctrl Pts',(3.21939660122333,-0.170421113847801,
36.5507066252172));
#34568=CARTESIAN_POINT('Ctrl Pts',(3.2228039392682,-0.0842040481459283,
36.5562032879677));
#34569=CARTESIAN_POINT('Ctrl Pts',(3.22263357550004,0.184970274485804,36.5736660170257));
#34570=CARTESIAN_POINT('Ctrl Pts',(3.20694277966631,0.367538399943799,36.5859673833119));
#34571=CARTESIAN_POINT('Ctrl Pts',(3.15894344069144,0.645829823717705,36.6050828408999));
#34572=CARTESIAN_POINT('Ctrl Pts',(3.13749662835673,0.743058334153712,36.6118258198534));
#34573=CARTESIAN_POINT('Ctrl Pts',(3.10457565432211,0.865131329287124,36.620278234588));
#34574=CARTESIAN_POINT('Ctrl Pts',(3.09724088761861,0.89103375506053,36.6220708041795));
#34575=CARTESIAN_POINT('Ctrl Pts',(3.06654473160006,0.994473963037814,36.6292184191876));
#34576=CARTESIAN_POINT('Ctrl Pts',(3.04058708029015,1.07121786073489,36.6344970946243));
#34577=CARTESIAN_POINT('Ctrl Pts',(3.00695581531393,1.15953299579155,36.6404799419706));
#34578=CARTESIAN_POINT('Ctrl Pts',(3.00206897881807,1.17212708571676,36.6413308873444));
#34579=CARTESIAN_POINT('Ctrl Pts',(2.99453543051912,1.19118592291648,36.6426148360029));
#34580=CARTESIAN_POINT('Ctrl Pts',(2.99194672477672,1.19767322165597,36.6430511985206));
#34581=CARTESIAN_POINT('Ctrl Pts',(2.9872538715903,1.20932334375856,36.6438335579084));
#34582=CARTESIAN_POINT('Ctrl Pts',(2.98515741117633,1.21448914159256,36.6441800079051));
#34583=CARTESIAN_POINT('Ctrl Pts',(2.98056009655472,1.22573336116057,36.6449331118216));
#34584=CARTESIAN_POINT('Ctrl Pts',(2.9780540571047,1.23180956183125,36.6453394461138));
#34585=CARTESIAN_POINT('Ctrl Pts',(2.97092667178849,1.24894189853023,36.6464834692871));
#34586=CARTESIAN_POINT('Ctrl Pts',(2.96626216830768,1.2599801246071,36.6472185866358));
#34587=CARTESIAN_POINT('Ctrl Pts',(2.93716503604649,1.32777928414764,36.651723219759));
#34588=CARTESIAN_POINT('Ctrl Pts',(2.91116378962115,1.38385794959682,36.6554032242125));
#34589=CARTESIAN_POINT('Ctrl Pts',(2.76347261567103,1.67977881225645,36.6747539223773));
#34590=CARTESIAN_POINT('Ctrl Pts',(2.61372736611706,1.90444108728551,36.6892804506745));
#34591=CARTESIAN_POINT('Ctrl Pts',(2.34376095287608,2.21665787511883,36.7127248839091));
#34592=CARTESIAN_POINT('Ctrl Pts',(2.24256419857794,2.31898376879698,36.7210616337054));
#34593=CARTESIAN_POINT('Ctrl Pts',(2.11882836152967,2.4284034428552,36.731000513484));
#34594=CARTESIAN_POINT('Ctrl Pts',(2.10263219673709,2.44244032027682,36.7322965821504));
#34595=CARTESIAN_POINT('Ctrl Pts',(2.07642359732163,2.46470088149511,36.7343868019875));
#34596=CARTESIAN_POINT('Ctrl Pts',(2.0664993079806,2.47302769761647,36.735176696898));
#34597=CARTESIAN_POINT('Ctrl Pts',(2.04878125856672,2.48771262000182,36.7365842272608));
#34598=CARTESIAN_POINT('Ctrl Pts',(2.04100738834421,2.49409453755293,36.7372008800983));
#34599=CARTESIAN_POINT('Ctrl Pts',(2.02473884915917,2.50732311237492,36.7384895474435));
#34600=CARTESIAN_POINT('Ctrl Pts',(2.016239043971,2.51416322262954,36.7391618156184));
#34601=CARTESIAN_POINT('Ctrl Pts',(1.99405204187911,2.53183305872703,36.7409140909781));
#34602=CARTESIAN_POINT('Ctrl Pts',(1.9803114508983,2.54259487947004,36.7419967975236));
#34603=CARTESIAN_POINT('Ctrl Pts',(1.91997054415686,2.58906886700687,36.7467412015817));
#34604=CARTESIAN_POINT('Ctrl Pts',(1.87248916450982,2.62361355511462,36.7504484297529));
#34605=CARTESIAN_POINT('Ctrl Pts',(1.74328790330577,2.71231859679064,36.7604747270384));
#34606=CARTESIAN_POINT('Ctrl Pts',(1.66000072818877,2.76407660133745,36.7668766405699));
#34607=CARTESIAN_POINT('Ctrl Pts',(1.40766936111291,2.90536384818186,36.786061721988));
#34608=CARTESIAN_POINT('Ctrl Pts',(1.232871877232,2.9837377322838,36.7991106145913));
#34609=CARTESIAN_POINT('Ctrl Pts',(0.926532175384797,3.08955104591862,36.8209196403535));
#34610=CARTESIAN_POINT('Ctrl Pts',(0.798307190894622,3.12514024818465,36.8297459469964));
#34611=CARTESIAN_POINT('Ctrl Pts',(0.653620244386708,3.15580756373062,36.8391233165872));
#34612=CARTESIAN_POINT('Ctrl Pts',(0.638982021735399,3.15880401407526,36.8400654689786));
#34613=CARTESIAN_POINT('Ctrl Pts',(0.617276612328088,3.16309006136898,36.8414522305245));
#34614=CARTESIAN_POINT('Ctrl Pts',(0.610225350643649,3.16445795931336,36.8419011387716));
#34615=CARTESIAN_POINT('Ctrl Pts',(0.597677836891366,3.1668485942409,36.8426970460851));
#34616=CARTESIAN_POINT('Ctrl Pts',(0.592183448714921,3.16788061333103,36.8430445684284));
#34617=CARTESIAN_POINT('Ctrl Pts',(0.58036448649849,3.17006876268273,36.8437899708233));
#34618=CARTESIAN_POINT('Ctrl Pts',(0.574039147667095,3.17122026292387,36.8441875851245));
#34619=CARTESIAN_POINT('Ctrl Pts',(0.55656201494484,3.17434789388611,36.8452826853262));
#34620=CARTESIAN_POINT('Ctrl Pts',(0.545403057365658,3.17628420356421,36.8459779394641));
#34621=CARTESIAN_POINT('Ctrl Pts',(0.48400431868569,3.18660504084151,36.8497827884402));
#34622=CARTESIAN_POINT('Ctrl Pts',(0.433578292551593,3.19385697964606,36.8528320604096));
#34623=CARTESIAN_POINT('Ctrl Pts',(0.126694374032891,3.23058801392747,36.8710472475619));
#34624=CARTESIAN_POINT('Ctrl Pts',(-0.132392916066827,3.23036419740347,
36.8850459308302));
#34625=CARTESIAN_POINT('Ctrl Pts',(-0.553144886143904,3.17924354978906,
36.9089761751536));
#34626=CARTESIAN_POINT('Ctrl Pts',(-0.715783007048575,3.14661767538846,
36.9185165948688));
#34627=CARTESIAN_POINT('Ctrl Pts',(-0.896295515390018,3.09568300091237,
36.9297975036102));
#34628=CARTESIAN_POINT('Ctrl Pts',(-0.917348495585595,3.08950976600439,
36.931123803746));
#34629=CARTESIAN_POINT('Ctrl Pts',(-0.950871975286829,3.07930702346509,
36.9332534381652));
#34630=CARTESIAN_POINT('Ctrl Pts',(-0.963384003351651,3.07541550237927,
36.9340522528097));
#34631=CARTESIAN_POINT('Ctrl Pts',(-0.985479219561552,3.06839532825165,
36.9354700707615));
#34632=CARTESIAN_POINT('Ctrl Pts',(-0.995072167840309,3.06529779299603,
36.9360880416007));
#34633=CARTESIAN_POINT('Ctrl Pts',(-1.01495353803362,3.05877499347314,36.9373738543905));
#34634=CARTESIAN_POINT('Ctrl Pts',(-1.02523950770585,3.05534271274126,36.9380419221032));
#34635=CARTESIAN_POINT('Ctrl Pts',(-1.05174915691184,3.04634788252861,36.9397711234567));
#34636=CARTESIAN_POINT('Ctrl Pts',(-1.06794594537064,3.04070767254742,36.940834825075));
#34637=CARTESIAN_POINT('Ctrl Pts',(-1.13673876207206,3.01613450103769,36.9453839773432));
#34638=CARTESIAN_POINT('Ctrl Pts',(-1.18887980529481,2.99596503961827,36.9489104514787));
#34639=CARTESIAN_POINT('Ctrl Pts',(-1.32490043599684,2.93923888201575,36.958324879121));
#34640=CARTESIAN_POINT('Ctrl Pts',(-1.40778887040859,2.90045072006253,36.9642836859241));
#34641=CARTESIAN_POINT('Ctrl Pts',(-1.70772472929498,2.74420604356364,36.9866514534945));
#34642=CARTESIAN_POINT('Ctrl Pts',(-1.91270368009395,2.60548260354482,37.0036323679565));
#34643=CARTESIAN_POINT('Ctrl Pts',(-2.16733902784523,2.38677102064044,37.0259392947688));
#34644=CARTESIAN_POINT('Ctrl Pts',(-2.23241276480209,2.32602036633145,37.0317570263363));
#34645=CARTESIAN_POINT('Ctrl Pts',(-2.30459826389271,2.25280612658301,37.0382686764267));
#34646=CARTESIAN_POINT('Ctrl Pts',(-2.3142390779141,2.24290127029268,37.0391395910877));
#34647=CARTESIAN_POINT('Ctrl Pts',(-2.32870215248365,2.22784954115069,37.0404475897907));
#34648=CARTESIAN_POINT('Ctrl Pts',(-2.33357158612701,2.22274851201286,37.0408882204375));
#34649=CARTESIAN_POINT('Ctrl Pts',(-2.34226356460735,2.2135830876514,37.0416751359755));
#34650=CARTESIAN_POINT('Ctrl Pts',(-2.346092319323,2.20952472780483,37.0420218979329));
#34651=CARTESIAN_POINT('Ctrl Pts',(-2.35437302294139,2.2007016498423,37.0427721404088));
#34652=CARTESIAN_POINT('Ctrl Pts',(-2.3588210427999,2.19593337162044,37.0431753205467));
#34653=CARTESIAN_POINT('Ctrl Pts',(-2.37123931686889,2.18253970971524,37.0443015737209));
#34654=CARTESIAN_POINT('Ctrl Pts',(-2.37917703781714,2.17388410798806,37.0450222011656));
#34655=CARTESIAN_POINT('Ctrl Pts',(-2.42573118851716,2.12255921522773,37.0492543391556));
#34656=CARTESIAN_POINT('Ctrl Pts',(-2.46324908445984,2.07890219088969,37.0526884271842));
#34657=CARTESIAN_POINT('Ctrl Pts',(-2.65930140451222,1.83800460723727,37.0709110177983));
#34658=CARTESIAN_POINT('Ctrl Pts',(-2.79536817759413,1.62360345248578,37.0846448609797));
#34659=CARTESIAN_POINT('Ctrl Pts',(-2.97573333399933,1.24813681637361,37.1081755874179));
#34660=CARTESIAN_POINT('Ctrl Pts',(-3.03518938676924,1.09565021399464,37.1175957507025));
#34661=CARTESIAN_POINT('Ctrl Pts',(-3.08920302742152,0.918379895379297,
37.1287420858921));
#34662=CARTESIAN_POINT('Ctrl Pts',(-3.09537110838261,0.897370961205556,
37.1300657795763));
#34663=CARTESIAN_POINT('Ctrl Pts',(-3.10488397570805,0.863703896920118,
37.1321920182396));
#34664=CARTESIAN_POINT('Ctrl Pts',(-3.10836660299303,0.851085176480857,
37.1329900665771));
#34665=CARTESIAN_POINT('Ctrl Pts',(-3.11439433102335,0.828714120288518,
37.1344069975532));
#34666=CARTESIAN_POINT('Ctrl Pts',(-3.11697075770407,0.818970350030057,
37.1350248520166));
#34667=CARTESIAN_POINT('Ctrl Pts',(-3.12222555820101,0.798713233184525,
37.1363108945144));
#34668=CARTESIAN_POINT('Ctrl Pts',(-3.12489663064067,0.788198140285589,
37.1369793106554));
#34669=CARTESIAN_POINT('Ctrl Pts',(-3.13165917973631,0.761001547505315,
37.1387104280406));
#34670=CARTESIAN_POINT('Ctrl Pts',(-3.13567044260096,0.744300631681173,
37.1397757080816));
#34671=CARTESIAN_POINT('Ctrl Pts',(-3.15221945776199,0.672889607208716,
37.1443407616012));
#34672=CARTESIAN_POINT('Ctrl Pts',(-3.16345965886952,0.617891803538932,
37.1478819161826));
#34673=CARTESIAN_POINT('Ctrl Pts',(-3.18931977790645,0.472039927098291,
37.1573454942228));
#34674=CARTESIAN_POINT('Ctrl Pts',(-3.20149397223313,0.380809869881011,
37.1633396944617));
#34675=CARTESIAN_POINT('Ctrl Pts',(-3.23146072734248,0.0482064408569172,
37.1854324681332));
#34676=CARTESIAN_POINT('Ctrl Pts',(-3.22596406277041,-0.194430714669504,
37.2020723137423));
#34677=CARTESIAN_POINT('Ctrl Pts',(-3.18088225099349,-0.526024420256396,
37.22434190437));
#34678=CARTESIAN_POINT('Ctrl Pts',(-3.16443211676231,-0.617321996036819,
37.2304125155196));
#34679=CARTESIAN_POINT('Ctrl Pts',(-3.14100181686343,-0.721401250402509,
37.2371701970664));
#34680=CARTESIAN_POINT('Ctrl Pts',(-3.13784956707135,-0.734991352746937,
37.238049324232));
#34681=CARTESIAN_POINT('Ctrl Pts',(-3.13296472537972,-0.755446696316358,
37.2393671989953));
#34682=CARTESIAN_POINT('Ctrl Pts',(-3.1312976444493,-0.762327190639459,
37.2398095715792));
#34683=CARTESIAN_POINT('Ctrl Pts',(-3.12827571303548,-0.774622345565591,
37.24059836306));
#34684=CARTESIAN_POINT('Ctrl Pts',(-3.12692946109608,-0.780039013078377,
37.240945268769));
#34685=CARTESIAN_POINT('Ctrl Pts',(-3.12398479059021,-0.791756810987841,
37.2416944183312));
#34686=CARTESIAN_POINT('Ctrl Pts',(-3.1223813824102,-0.798056592057209,
37.242096369373));
#34687=CARTESIAN_POINT('Ctrl Pts',(-3.11785094746984,-0.815633975101017,
37.243215721764));
#34688=CARTESIAN_POINT('Ctrl Pts',(-3.11488177370662,-0.826900754306286,
37.2439307256483));
#34689=CARTESIAN_POINT('Ctrl Pts',(-3.09728790003992,-0.89222251294425,
37.2480630269886));
#34690=CARTESIAN_POINT('Ctrl Pts',(-3.08131642639808,-0.945908721459504,
37.2514070996175));
#34691=CARTESIAN_POINT('Ctrl Pts',(-2.98515110660766,-1.24080389563577,
37.2696241341481));
#34692=CARTESIAN_POINT('Ctrl Pts',(-2.87803202414719,-1.47230447864389,
37.2834171147081));
#34693=CARTESIAN_POINT('Ctrl Pts',(-2.65885976161363,-1.82851934396009,
37.3070405146908));
#34694=CARTESIAN_POINT('Ctrl Pts',(-2.56238400196479,-1.96142702769182,
37.3164913659328));
#34695=CARTESIAN_POINT('Ctrl Pts',(-2.44203953090745,-2.10310256496634,
37.3276720280684));
#34696=CARTESIAN_POINT('Ctrl Pts',(-2.42768750438157,-2.11965346555868,
37.328996392058));
#34697=CARTESIAN_POINT('Ctrl Pts',(-2.40448948106646,-2.14586097999958,
37.3311235040547));
#34698=CARTESIAN_POINT('Ctrl Pts',(-2.39575127014583,-2.15561240804024,
37.3319217495112));
#34699=CARTESIAN_POINT('Ctrl Pts',(-2.3801819403947,-2.17277543323153,37.3333389085882));
#34700=CARTESIAN_POINT('Ctrl Pts',(-2.37337498200137,-2.18020878444696,
37.3339567929294));
#34701=CARTESIAN_POINT('Ctrl Pts',(-2.35916991163932,-2.19557567899414,
37.3352427760587));
#34702=CARTESIAN_POINT('Ctrl Pts',(-2.35176639903119,-2.20350403538454,
37.3359111023494));
#34703=CARTESIAN_POINT('Ctrl Pts',(-2.33254173034325,-2.2238843106004,37.3376417256947));
#34704=CARTESIAN_POINT('Ctrl Pts',(-2.3206609577078,-2.23627928750168,37.3387065987548));
#34705=CARTESIAN_POINT('Ctrl Pts',(-2.26956127909485,-2.28874483413571,
37.3432675469909));
#34706=CARTESIAN_POINT('Ctrl Pts',(-2.22940126084228,-2.32788116026025,
37.3468049107828));
#34707=CARTESIAN_POINT('Ctrl Pts',(-2.12079814275964,-2.4283271441839,37.3562557881338));
#34708=CARTESIAN_POINT('Ctrl Pts',(-2.05072260321249,-2.48778852983414,
37.3622408391819));
#34709=CARTESIAN_POINT('Ctrl Pts',(-1.82076289780361,-2.66659256755328,
37.3815103996241));
#34710=CARTESIAN_POINT('Ctrl Pts',(-1.65238201600226,-2.77406600268191,
37.3951166831969));
#34711=CARTESIAN_POINT('Ctrl Pts',(-1.47525540431025,-2.86526422072266,
37.4085260041042));
#34712=CARTESIAN_POINT('Origin',(0.,0.,4.68922655072688));
#34713=CARTESIAN_POINT('',(-1.47525540501186,-2.86526422036142,34.9999952908233));
#34714=CARTESIAN_POINT('',(-1.47525552646581,-2.8652641578277,35.1563175586878));
#34715=CARTESIAN_POINT('',(-1.47525540501186,-2.86526422036142,4.68922655072688));
#34716=CARTESIAN_POINT('',(-3.05037901532684,-1.03985836792983,35.0000143649096));
#34717=CARTESIAN_POINT('Origin',(0.,0.,35.));
#34718=CARTESIAN_POINT('Ctrl Pts',(-1.47525552646581,-2.8652641578277,35.1563175586878));
#34719=CARTESIAN_POINT('Ctrl Pts',(-1.5179786368742,-2.84326705694414,35.1534900287168));
#34720=CARTESIAN_POINT('Ctrl Pts',(-1.56021632410078,-2.82031103518203,
35.150632229143));
#34721=CARTESIAN_POINT('Ctrl Pts',(-1.62096631363004,-2.78551014190289,
35.146421317202));
#34722=CARTESIAN_POINT('Ctrl Pts',(-1.63988409403924,-2.7744150126229,35.1450954968172));
#34723=CARTESIAN_POINT('Ctrl Pts',(-1.6699213053194,-2.75638387962761,35.1429663459599));
#34724=CARTESIAN_POINT('Ctrl Pts',(-1.68111443427663,-2.74957151366147,
35.1421675300128));
#34725=CARTESIAN_POINT('Ctrl Pts',(-1.70084704537755,-2.73739631176315,
35.1407495369148));
#34726=CARTESIAN_POINT('Ctrl Pts',(-1.70940353540863,-2.73206127107097,
35.1401313914053));
#34727=CARTESIAN_POINT('Ctrl Pts',(-1.72711415399747,-2.72090278595853,
35.1388450421301));
#34728=CARTESIAN_POINT('Ctrl Pts',(-1.73626418293619,-2.71507310288679,
35.1381766115914));
#34729=CARTESIAN_POINT('Ctrl Pts',(-1.75981505434774,-2.69990059222446,
35.1364460971715));
#34730=CARTESIAN_POINT('Ctrl Pts',(-1.77417085675511,-2.6904888005836,35.135381439547));
#34731=CARTESIAN_POINT('Ctrl Pts',(-1.83503964978362,-2.64988367822589,
35.130824774063));
#34732=CARTESIAN_POINT('Ctrl Pts',(-1.88080814757814,-2.61759700897596,
35.1272915814473));
#34733=CARTESIAN_POINT('Ctrl Pts',(-1.99924781255354,-2.52933522155223,
35.1178552546094));
#34734=CARTESIAN_POINT('Ctrl Pts',(-2.07040678604797,-2.47142503715811,
35.1118808696354));
#34735=CARTESIAN_POINT('Ctrl Pts',(-2.32202096135386,-2.24815717635066,
35.0896297664439));
#34736=CARTESIAN_POINT('Ctrl Pts',(-2.48593682768389,-2.06545269928067,
35.0727943646564));
#34737=CARTESIAN_POINT('Ctrl Pts',(-2.68002016186566,-1.7921516345158,35.0505052130097));
#34738=CARTESIAN_POINT('Ctrl Pts',(-2.72931560658516,-1.71614543216571,
35.0445815800732));
#34739=CARTESIAN_POINT('Ctrl Pts',(-2.78240414784869,-1.62620336552493,
35.0379665134103));
#34740=CARTESIAN_POINT('Ctrl Pts',(-2.7893825488052,-1.61420421283992,35.037091854403));
#34741=CARTESIAN_POINT('Ctrl Pts',(-2.79979613030385,-1.59602917237582,
35.0357792620165));
#34742=CARTESIAN_POINT('Ctrl Pts',(-2.80328877516139,-1.58988664239112,
35.0353377469127));
#34743=CARTESIAN_POINT('Ctrl Pts',(-2.80950444728965,-1.57887095232093,
35.0345497698746));
#34744=CARTESIAN_POINT('Ctrl Pts',(-2.81223503144743,-1.574002176899,35.0342028264667));
#34745=CARTESIAN_POINT('Ctrl Pts',(-2.81812494196711,-1.5634359004169,35.0334527747247));
#34746=CARTESIAN_POINT('Ctrl Pts',(-2.82127963779431,-1.55773592447216,
35.0330499638339));
#34747=CARTESIAN_POINT('Ctrl Pts',(-2.83005619289586,-1.54176412620451,
35.0319261826464));
#34748=CARTESIAN_POINT('Ctrl Pts',(-2.83563945374104,-1.53147104902214,
35.0312076395943));
#34749=CARTESIAN_POINT('Ctrl Pts',(-2.86803336675817,-1.47096639833774,
35.0270157530493));
#34750=CARTESIAN_POINT('Ctrl Pts',(-2.89356790136217,-1.42007861040143,
35.0236181149031));
#34751=CARTESIAN_POINT('Ctrl Pts',(-2.96799167462051,-1.26140600856599,
35.0133313483208));
#34752=CARTESIAN_POINT('Ctrl Pts',(-3.01226077392425,-1.15167656092768,
35.0066413036545));
#34753=CARTESIAN_POINT('Ctrl Pts',(-3.05037901532683,-1.03985836792984,
35.0000143649095));
#34754=CARTESIAN_POINT('Ctrl Pts',(1.43039598794072,-2.88162839993989,6.58668234580631));
#34755=CARTESIAN_POINT('Ctrl Pts',(2.3908869304735,-2.40485547853165,6.65299332526079));
#34756=CARTESIAN_POINT('Ctrl Pts',(3.78068485083689,-0.42330470969778,6.78561528416975));
#34757=CARTESIAN_POINT('Ctrl Pts',(2.39660828659712,2.9593008547868,6.98454822253319));
#34758=CARTESIAN_POINT('Ctrl Pts',(-1.19393826692811,3.61225397709376,7.18348116089663));
#34759=CARTESIAN_POINT('Ctrl Pts',(-3.68522155716544,0.949002744436199,
7.38241409926007));
#34760=CARTESIAN_POINT('Ctrl Pts',(-2.78953196244949,-2.58902355773568,
7.5813470376235));
#34761=CARTESIAN_POINT('Ctrl Pts',(0.671039291373588,-3.74572463321816,
7.78027997598695));
#34762=CARTESIAN_POINT('Ctrl Pts',(3.51448527473695,-1.45960212386322,7.97921291435037));
#34763=CARTESIAN_POINT('Ctrl Pts',(3.12717197768531,2.16867191230057,8.17814585271383));
#34764=CARTESIAN_POINT('Ctrl Pts',(-0.135028807280012,3.80310255787661,
8.37707879107726));
#34765=CARTESIAN_POINT('Ctrl Pts',(-3.27306356366253,1.94141424541036,8.5760117294407));
#34766=CARTESIAN_POINT('Ctrl Pts',(-3.40217358758694,-1.70507215059562,
8.77494466780414));
#34767=CARTESIAN_POINT('Ctrl Pts',(-0.403640923403273,-3.78405339475958,
8.97387760616759));
#34768=CARTESIAN_POINT('Ctrl Pts',(2.96595593022244,-2.38435003081143,9.172810544531));
#34769=CARTESIAN_POINT('Ctrl Pts',(3.60893852822567,1.20730380998424,9.37174348289446));
#34770=CARTESIAN_POINT('Ctrl Pts',(0.934206293343398,3.68907429945195,9.57067642125789));
#34771=CARTESIAN_POINT('Ctrl Pts',(-2.59934534842778,2.77946388606067,9.76960935962134));
#34772=CARTESIAN_POINT('Ctrl Pts',(-3.7433073822935,-0.685321221973841,
9.96854229798476));
#34773=CARTESIAN_POINT('Ctrl Pts',(-1.4460297930754,-3.52008693042821,10.1674752363482));
#34774=CARTESIAN_POINT('Ctrl Pts',(2.18058944266648,-3.11882102941849,10.3664081747117));
#34775=CARTESIAN_POINT('Ctrl Pts',(3.80258297155867,0.14959131214445,10.5653411130751));
#34776=CARTESIAN_POINT('Ctrl Pts',(1.92884471639216,3.28048361242447,10.7642740514386));
#34777=CARTESIAN_POINT('Ctrl Pts',(-1.71808921409888,3.39561249800469,10.963206989802));
#34778=CARTESIAN_POINT('Ctrl Pts',(-3.78557595114969,0.389139407006486,
11.1621399281654));
#34779=CARTESIAN_POINT('Ctrl Pts',(-2.37296555731667,-2.97507129439684,
11.3610728665289));
#34780=CARTESIAN_POINT('Ctrl Pts',(1.2211228251491,-3.60428547773973,11.5600058048923));
#34781=CARTESIAN_POINT('Ctrl Pts',(3.69262746162031,-0.920063684940536,
11.7589387432558));
#34782=CARTESIAN_POINT('Ctrl Pts',(2.76948293800576,2.60997682152157,11.9578716816192));
#34783=CARTESIAN_POINT('Ctrl Pts',(-0.699659800874596,3.74065380890841,
12.1568046199826));
#34784=CARTESIAN_POINT('Ctrl Pts',(-3.52560211426312,1.43253079764144,12.3557375583461));
#34785=CARTESIAN_POINT('Ctrl Pts',(-3.11044242675709,-2.19252426758155,
12.5546704967095));
#34786=CARTESIAN_POINT('Ctrl Pts',(0.164161079403195,-3.8019818377298,12.7536034350729));
#34787=CARTESIAN_POINT('Ctrl Pts',(3.2878505613498,-1.91626027473385,12.9525363734364));
#34788=CARTESIAN_POINT('Ctrl Pts',(3.38900412249117,1.73108804282604,13.1514693117998));
#34789=CARTESIAN_POINT('Ctrl Pts',(0.374630835682455,3.78703927775718,13.3504022501632));
#34790=CARTESIAN_POINT('Ctrl Pts',(-2.98414227610861,2.36154814268967,13.5493351885267));
#34791=CARTESIAN_POINT('Ctrl Pts',(-3.59957987005836,-1.23492490191512,
13.7482681268901));
#34792=CARTESIAN_POINT('Ctrl Pts',(-0.905907377036315,-3.69612588780959,
13.9472010652536));
#34793=CARTESIAN_POINT('Ctrl Pts',(2.6205698730494,-2.7594615950884,14.146134003617));
#34794=CARTESIAN_POINT('Ctrl Pts',(3.73794536304987,0.713988247211487,14.3450669419804));
#34795=CARTESIAN_POINT('Ctrl Pts',(1.41901074133174,3.53106545822759,14.5439998803439));
#34796=CARTESIAN_POINT('Ctrl Pts',(-2.2044268855072,3.10201819155779,14.7429328187073));
#34797=CARTESIAN_POINT('Ctrl Pts',(-3.8013248865683,-0.178728456209389,
14.9418657570708));
#34798=CARTESIAN_POINT('Ctrl Pts',(-1.90364769271949,-3.29516922422906,
15.1407986954342));
#34799=CARTESIAN_POINT('Ctrl Pts',(1.74406145191863,-3.38234599150264,15.3397316337976));
#34800=CARTESIAN_POINT('Ctrl Pts',(3.78844700014203,-0.360116760811474,
15.5386645721611));
#34801=CARTESIAN_POINT('Ctrl Pts',(2.35009605280664,2.993169440056,15.7375975105245));
#34802=CARTESIAN_POINT('Ctrl Pts',(-1.24870884594248,3.59482141035789,15.9365304488879));
#34803=CARTESIAN_POINT('Ctrl Pts',(-3.69957004376932,0.891737767254035,
16.1354633872514));
#34804=CARTESIAN_POINT('Ctrl Pts',(-2.74939973479973,-2.63112444642698,
16.3343963256148));
#34805=CARTESIAN_POINT('Ctrl Pts',(0.728306209987826,-3.73518203288617,
16.5333292639783));
#34806=CARTESIAN_POINT('Ctrl Pts',(3.53647695542546,-1.40546984956888,16.7322622023417));
#34807=CARTESIAN_POINT('Ctrl Pts',(3.09354840927974,2.21629713570752,16.9311951407051));
#34808=CARTESIAN_POINT('Ctrl Pts',(-0.193293208732243,3.80061212040383,
17.1301280790686));
#34809=CARTESIAN_POINT('Ctrl Pts',(-3.30243950399845,1.89100715935529,17.329061017432));
#34810=CARTESIAN_POINT('Ctrl Pts',(-3.37563819737945,-1.75700925287699,
17.5279939557954));
#34811=CARTESIAN_POINT('Ctrl Pts',(-0.345597398331251,-3.78979909659722,
17.7269268941589));
#34812=CARTESIAN_POINT('Ctrl Pts',(3.00215265516693,-2.33860945636005,17.9258598325223));
#34813=CARTESIAN_POINT('Ctrl Pts',(3.5900101677383,1.26247445512302,18.1247927708858));
#34814=CARTESIAN_POINT('Ctrl Pts',(0.877555064047497,3.70295987878172,18.3237257092492));
#34815=CARTESIAN_POINT('Ctrl Pts',(-2.6416403868901,2.73929750495517,18.5226586476126));
#34816=CARTESIAN_POINT('Ctrl Pts',(-3.73236385888241,-0.742613479012362,
18.7215915859761));
#34817=CARTESIAN_POINT('Ctrl Pts',(-1.39190832123119,-3.54183652637864,
18.9205245243395));
#34818=CARTESIAN_POINT('Ctrl Pts',(2.22813484392072,-3.085033204296,19.119457462703));
#34819=CARTESIAN_POINT('Ctrl Pts',(3.79984354968653,0.20785512312247,19.3183904010664));
#34820=CARTESIAN_POINT('Ctrl Pts',(1.87833886025086,3.30966129390517,19.5173233394298));
#34821=CARTESIAN_POINT('Ctrl Pts',(-1.76993125559216,3.36888083861398,19.7162562777933));
#34822=CARTESIAN_POINT('Ctrl Pts',(-3.79109554726769,0.331072961429409,
19.9151892161567));
#34823=CARTESIAN_POINT('Ctrl Pts',(-2.32708852200922,-3.01109178954004,
20.1141221545202));
#34824=CARTESIAN_POINT('Ctrl Pts',(1.27622152733633,-3.58514621284347,20.3130550928836));
#34825=CARTESIAN_POINT('Ctrl Pts',(3.70629534307339,-0.863359475661814,
20.511988031247));
#34826=CARTESIAN_POINT('Ctrl Pts',(2.72915505388636,2.65211754003269,20.7109209696104));
#34827=CARTESIAN_POINT('Ctrl Pts',(-0.756909844210963,3.729490882418,20.9098539079739));
#34828=CARTESIAN_POINT('Ctrl Pts',(-3.54714409239226,1.37832635544315,21.1087868463373));
#34829=CARTESIAN_POINT('Ctrl Pts',(-3.07647270163572,-2.23993983633326,
21.3077197847008));
#34830=CARTESIAN_POINT('Ctrl Pts',(0.222413985566929,-3.79901918570132,
21.5066527230642));
#34831=CARTESIAN_POINT('Ctrl Pts',(3.31683448791136,-1.86564298141534,21.7055856614276));
#34832=CARTESIAN_POINT('Ctrl Pts',(3.36207401442483,1.78282727032986,21.9045185997911));
#34833=CARTESIAN_POINT('Ctrl Pts',(0.316543663368888,3.79233633311756,22.1034515381545));
#34834=CARTESIAN_POINT('Ctrl Pts',(-3.01998671192163,2.31553341891654,22.3023844765179));
#34835=CARTESIAN_POINT('Ctrl Pts',(-3.58022961709107,-1.28994986073349,
22.5013174148814));
#34836=CARTESIAN_POINT('Ctrl Pts',(-0.849151210531485,-3.70957638766954,
22.7002503532448));
#34837=CARTESIAN_POINT('Ctrl Pts',(2.66255575201821,-2.71897253051539,22.8991832916083));
#34838=CARTESIAN_POINT('Ctrl Pts',(3.72656314567699,0.771195095669392,23.0981162299717));
#34839=CARTESIAN_POINT('Ctrl Pts',(1.3647241516294,3.55239957553509,23.2970491683351));
#34840=CARTESIAN_POINT('Ctrl Pts',(-2.25171193961186,3.06786702699317,23.4959821066986));
#34841=CARTESIAN_POINT('Ctrl Pts',(-3.79813904055242,-0.236969582297126,
23.694915045062));
#34842=CARTESIAN_POINT('Ctrl Pts',(-1.85291970926293,-3.32395898069267,
23.8938479834255));
#34843=CARTESIAN_POINT('Ctrl Pts',(1.79569710773726,-3.35521782475692,24.0927809217889));
#34844=CARTESIAN_POINT('Ctrl Pts',(3.79352143592832,-0.302009717484061,
24.2917138601523));
#34845=CARTESIAN_POINT('Ctrl Pts',(2.30394431674614,3.02883729170711,24.4906467985158));
#34846=CARTESIAN_POINT('Ctrl Pts',(-1.30365925374081,3.57526045267173,24.6895797368792));
#34847=CARTESIAN_POINT('Ctrl Pts',(-3.71280296439449,0.834930477277034,
24.8885126752426));
#34848=CARTESIAN_POINT('Ctrl Pts',(-2.70875008435262,-2.67295486958203,
25.0874456136061));
#34849=CARTESIAN_POINT('Ctrl Pts',(0.785469023636781,-3.72358069164743,
25.2863785519695));
#34850=CARTESIAN_POINT('Ctrl Pts',(3.55760289864069,-1.35110190951161,25.485311490333));
#34851=CARTESIAN_POINT('Ctrl Pts',(3.05921630672578,2.26345098090627,25.6842444286964));
#34852=CARTESIAN_POINT('Ctrl Pts',(-0.251521699592702,3.79720312716301,
25.8831773670599));
#34853=CARTESIAN_POINT('Ctrl Pts',(-3.33103466763993,1.84016923060991,26.0821103054233));
#34854=CARTESIAN_POINT('Ctrl Pts',(-3.34831237027993,-1.80854057884607,
26.2810432437867));
#34855=CARTESIAN_POINT('Ctrl Pts',(-0.287471337177379,-3.79465083829908,
26.4799761821502));
#34856=CARTESIAN_POINT('Ctrl Pts',(3.03764339894311,-2.29232138566123,26.6789091205136));
#34857=CARTESIAN_POINT('Ctrl Pts',(3.57023879254785,1.31734950506271,26.877842058877));
#34858=CARTESIAN_POINT('Ctrl Pts',(0.820697484702102,3.71597502587224,27.0767749972405));
#34859=CARTESIAN_POINT('Ctrl Pts',(-2.68331474003338,2.69848786549469,27.2757079356039));
#34860=CARTESIAN_POINT('Ctrl Pts',(-3.72054356412085,-0.799731418528385,
27.4746408739674));
#34861=CARTESIAN_POINT('Ctrl Pts',(-1.3374598291058,-3.56275398530838,27.6735738123308));
#34862=CARTESIAN_POINT('Ctrl Pts',(2.27515678785163,-3.05052066785249,27.8725067506942));
#34863=CARTESIAN_POINT('Ctrl Pts',(3.79621145927515,0.266070123784241,28.0714396890576));
#34864=CARTESIAN_POINT('Ctrl Pts',(1.82739173267215,3.33806144486047,28.2703726274211));
#34865=CARTESIAN_POINT('Ctrl Pts',(-1.82135749507502,3.34135775238698,28.4693055657845));
#34866=CARTESIAN_POINT('Ctrl Pts',(-3.79572452364676,0.272928735916584,
28.668238504148));
#34867=CARTESIAN_POINT('Ctrl Pts',(-2.28066479632187,-3.04640490432913,
28.8671714425114));
#34868=CARTESIAN_POINT('Ctrl Pts',(1.33102041368457,-3.56516471045272,29.0661043808749));
#34869=CARTESIAN_POINT('Ctrl Pts',(3.71909252552727,-0.806452441790404,
29.2650373192383));
#34870=CARTESIAN_POINT('Ctrl Pts',(2.68818602462228,2.69363521125782,29.4639702576017));
#34871=CARTESIAN_POINT('Ctrl Pts',(-0.81398207092878,3.71745180769153,29.6629031959652));
#34872=CARTESIAN_POINT('Ctrl Pts',(-3.56785275990456,1.32379811071928,29.8618361343286));
#34873=CARTESIAN_POINT('Ctrl Pts',(-3.04178023805176,-2.286829188571,30.060769072692));
#34874=CARTESIAN_POINT('Ctrl Pts',(0.280614641256556,-3.79516405144956,
30.2597020110555));
#34875=CARTESIAN_POINT('Ctrl Pts',(3.34503920917982,-1.81458740306222,30.4586349494189));
#34876=CARTESIAN_POINT('Ctrl Pts',(3.33435407319303,1.83414766823269,30.6575678877823));
#34877=CARTESIAN_POINT('Ctrl Pts',(0.258382127231354,3.7967424762064,30.8565008261458));
#34878=CARTESIAN_POINT('Ctrl Pts',(-3.05512167921966,2.26897471988225,31.0554337645092));
#34879=CARTESIAN_POINT('Ctrl Pts',(-3.56003828088928,-1.34467177887595,
31.2543667028727));
#34880=CARTESIAN_POINT('Ctrl Pts',(-0.792195557702424,-3.7221554175852,
31.4532996412361));
#34881=CARTESIAN_POINT('Ctrl Pts',(2.70391613171949,-2.67784471299768,31.6522325795996));
#34882=CARTESIAN_POINT('Ctrl Pts',(3.71430546775585,0.828220771595132,31.851165517963));
#34883=CARTESIAN_POINT('Ctrl Pts',(1.31011695494754,3.57289914756372,32.0500984563264));
#34884=CARTESIAN_POINT('Ctrl Pts',(-2.29846801167811,3.03299514565962,32.2490313946898));
#34885=CARTESIAN_POINT('Ctrl Pts',(-3.79406091906533,-0.295155038451869,
32.4479643330533));
#34886=CARTESIAN_POINT('Ctrl Pts',(-1.8017564297867,-3.35196785814317,32.6468972714167));
#34887=CARTESIAN_POINT('Ctrl Pts',(1.84691091052057,-3.32730143553342,32.8458302097802));
#34888=CARTESIAN_POINT('Ctrl Pts',(3.79770468103133,-0.243831724710034,
33.0447631481436));
#34889=CARTESIAN_POINT('Ctrl Pts',(2.25725132798827,3.06379359562579,33.2436960865071));
#34890=CARTESIAN_POINT('Ctrl Pts',(-1.35830340019312,3.55485957912918,33.4426290248705));
#34891=CARTESIAN_POINT('Ctrl Pts',(-3.72516365707354,0.777927041772669,
33.6415619632339));
#34892=CARTESIAN_POINT('Ctrl Pts',(-2.66746408246281,-2.71415735046314,
33.8404949015973));
#34893=CARTESIAN_POINT('Ctrl Pts',(0.842447311459858,-3.71110459051167,
34.0394278399608));
#34894=CARTESIAN_POINT('Ctrl Pts',(3.57789307418948,-1.29641656267163,34.2383607783242));
#34895=CARTESIAN_POINT('Ctrl Pts',(3.02416551966811,2.31007308627943,34.4372937166877));
#34896=CARTESIAN_POINT('Ctrl Pts',(-0.309691101873131,3.79290207832017,
34.6362266550511));
#34897=CARTESIAN_POINT('Ctrl Pts',(-3.35884729001673,1.78889900124255,34.8351595934145));
#34898=CARTESIAN_POINT('Ctrl Pts',(-3.32019994296254,-1.85964703453407,
35.034092531778));
#34899=CARTESIAN_POINT('Ctrl Pts',(-0.229277741996502,-3.79861112399583,
35.2330254701414));
#34900=CARTESIAN_POINT('Ctrl Pts',(3.07242052621671,-2.24549479277051,35.4319584085049));
#34901=CARTESIAN_POINT('Ctrl Pts',(3.54962868121306,1.37191507747408,35.6308913468683));
#34902=CARTESIAN_POINT('Ctrl Pts',(0.763647103503218,3.72811719983819,35.8298242852317));
#34903=CARTESIAN_POINT('Ctrl Pts',(-2.72435871711047,2.65704428540604,36.0287572235952));
#34904=CARTESIAN_POINT('Ctrl Pts',(-3.70784922296926,-0.856661481574834,
36.2276901619586));
#34905=CARTESIAN_POINT('Ctrl Pts',(-1.28269713503262,-3.58283446656971,
36.426623100322));
#34906=CARTESIAN_POINT('Ctrl Pts',(2.3216442419344,-3.01529148950444,36.6255560386855));
#34907=CARTESIAN_POINT('Ctrl Pts',(3.79168754631124,0.324222617667434,36.8244889770489));
#34908=CARTESIAN_POINT('Ctrl Pts',(1.77601530605909,3.36567740459321,37.0234219154124));
#34909=CARTESIAN_POINT('Ctrl Pts',(-1.8723558529673,3.31304969821073,37.2223548537758));
#34910=CARTESIAN_POINT('Ctrl Pts',(-3.7994617923675,0.214720395742962,37.4212877921392));
#34911=CARTESIAN_POINT('Ctrl Pts',(-2.23370528574428,-3.08100234999048,
37.6202207305027));
#34912=CARTESIAN_POINT('Ctrl Pts',(1.38550660873585,-3.54434565307739,37.8191536688661));
#34913=CARTESIAN_POINT('Ctrl Pts',(3.73101600658191,-0.749355973410843,
38.0180866072295));
#34914=CARTESIAN_POINT('Ctrl Pts',(2.64658546701708,2.7345201218469,38.217019545593));
#34915=CARTESIAN_POINT('Ctrl Pts',(-0.870863058265686,3.70453933627131,
38.4159524839564));
#34916=CARTESIAN_POINT('Ctrl Pts',(-3.58772328085212,1.26895902047793,38.6148854223199));
#34917=CARTESIAN_POINT('Ctrl Pts',(-3.00637313042353,-2.33318159065596,
38.8138183606833));
#34918=CARTESIAN_POINT('Ctrl Pts',(0.338749266911483,-3.79041680024323,
39.0127512990467));
#34919=CARTESIAN_POINT('Ctrl Pts',(3.37245830401273,-1.76310657017941,39.2116842374102));
#34920=CARTESIAN_POINT('Ctrl Pts',(3.30585041806794,1.88503916744779,39.4106171757737));
#34921=CARTESIAN_POINT('Ctrl Pts',(0.200160644147806,3.80025286079382,39.609550114137));
#34922=CARTESIAN_POINT('Ctrl Pts',(-3.08954036858721,2.2218902919993,39.8084830525005));
#34923=CARTESIAN_POINT('Ctrl Pts',(-3.53900783447175,-1.39909181671731,
40.0074159908639));
#34924=CARTESIAN_POINT('Ctrl Pts',(-0.735059111694563,-3.73383314394713,
40.2063489292274));
#34925=CARTESIAN_POINT('Ctrl Pts',(2.74465148416864,-2.63613934982058,40.4052818675907));
#34926=CARTESIAN_POINT('Ctrl Pts',(3.70115567014427,0.885150728230919,40.6042148059543));
#34927=CARTESIAN_POINT('Ctrl Pts',(1.25523944945949,3.59236978650378,40.8031477443176));
#34928=CARTESIAN_POINT('Ctrl Pts',(-2.34475597191911,2.99777433843635,41.0020806826812));
#34929=CARTESIAN_POINT('Ctrl Pts',(-3.78895369938313,-0.353968922753305,
41.2010136210445));
#34930=CARTESIAN_POINT('Ctrl Pts',(-1.75043395750614,-3.37784670177234,
41.399946559408));
#34931=CARTESIAN_POINT('Ctrl Pts',(1.89819598814578,-3.30121868695718,41.5988794977715));
#34932=CARTESIAN_POINT('Ctrl Pts',(3.80045064895368,-0.179534356723371,
41.7978556019462));
#34933=CARTESIAN_POINT('Ctrl Pts',(2.74058008982409,1.99769120286346,41.9305207266665));
#34934=CARTESIAN_POINT('Ctrl Pts',(1.86660756886202,2.62022723339283,41.9968748719324));
#34935=CARTESIAN_POINT('Ctrl Pts',(1.53698740838146,-3.09636394654476,6.72509367227838));
#34936=CARTESIAN_POINT('Ctrl Pts',(2.56905300209345,-2.58406246986299,6.79140465173286));
#34937=CARTESIAN_POINT('Ctrl Pts',(4.06241702282764,-0.454848876953752,
6.92402661064182));
#34938=CARTESIAN_POINT('Ctrl Pts',(2.5752007069213,3.17982446103466,7.12295954900526));
#34939=CARTESIAN_POINT('Ctrl Pts',(-1.28290913713704,3.88143487920559,7.32189248736869));
#34940=CARTESIAN_POINT('Ctrl Pts',(-3.9598399172061,1.01972130865502,7.52082542573213));
#34941=CARTESIAN_POINT('Ctrl Pts',(-2.9974045912523,-2.78195453691917,7.71975836409557));
#34942=CARTESIAN_POINT('Ctrl Pts',(0.721044347205764,-4.02485161106244,
7.91869130245901));
#34943=CARTESIAN_POINT('Ctrl Pts',(3.776380568565,-1.56836995107503,8.11762424082243));
#34944=CARTESIAN_POINT('Ctrl Pts',(3.36020514183989,2.33027878309083,8.3165571791859));
#34945=CARTESIAN_POINT('Ctrl Pts',(-0.145090994597224,4.08650527093188,
8.51549011754931));
#34946=CARTESIAN_POINT('Ctrl Pts',(-3.51696839657934,2.08608614314127,8.71442305591277));
#34947=CARTESIAN_POINT('Ctrl Pts',(-3.65569954707234,-1.83213211442255,
8.91335599427619));
#34948=CARTESIAN_POINT('Ctrl Pts',(-0.433719768517655,-4.06603658666688,
9.11228893263964));
#34949=CARTESIAN_POINT('Ctrl Pts',(3.18697546483547,-2.5620289803853,9.31122187100306));
#34950=CARTESIAN_POINT('Ctrl Pts',(3.87787236700172,1.2972706646837,9.51015480936652));
#34951=CARTESIAN_POINT('Ctrl Pts',(1.00382224349398,3.96397976129963,9.70908774772995));
#34952=CARTESIAN_POINT('Ctrl Pts',(-2.7930454952688,2.98658625369632,9.90802068609338));
#34953=CARTESIAN_POINT('Ctrl Pts',(-4.02225422945243,-0.736390550414543,
10.1069536244569));
#34954=CARTESIAN_POINT('Ctrl Pts',(-1.55378622621903,-3.78239965302563,
10.3058865628203));
#34955=CARTESIAN_POINT('Ctrl Pts',(2.34308439375097,-3.3512318907665,10.5048195011837));
#34956=CARTESIAN_POINT('Ctrl Pts',(4.08594696565489,0.160738680133138,10.7037524395472));
#34957=CARTESIAN_POINT('Ctrl Pts',(2.07257994765896,3.52494137861565,10.9026853779106));
#34958=CARTESIAN_POINT('Ctrl Pts',(-1.84611919413145,3.64864953283978,11.101618316274));
#34959=CARTESIAN_POINT('Ctrl Pts',(-4.06767260216181,0.418137616238003,
11.3005512546375));
#34960=CARTESIAN_POINT('Ctrl Pts',(-2.54979614936507,-3.19677009518745,
11.4994841930009));
#34961=CARTESIAN_POINT('Ctrl Pts',(1.31211945654531,-3.87287257668649,11.6984171313644));
#34962=CARTESIAN_POINT('Ctrl Pts',(3.96779770091828,-0.98862574460827,11.8973500697278));
#34963=CARTESIAN_POINT('Ctrl Pts',(2.97586153717486,2.80446921318709,12.0962830080912));
#34964=CARTESIAN_POINT('Ctrl Pts',(-0.75179762328831,4.01940291491122,12.2952159464547));
#34965=CARTESIAN_POINT('Ctrl Pts',(-3.78832582184925,1.53928130158088,12.4941488848181));
#34966=CARTESIAN_POINT('Ctrl Pts',(-3.34222892452571,-2.35590858772967,
12.6930818231815));
#34967=CARTESIAN_POINT('Ctrl Pts',(0.176394169248418,-4.08530103604272,
12.892014761545));
#34968=CARTESIAN_POINT('Ctrl Pts',(3.53285730387823,-2.05905772826418,13.0909476999084));
#34969=CARTESIAN_POINT('Ctrl Pts',(3.64154870898418,1.86008668023026,13.2898806382719));
#34970=CARTESIAN_POINT('Ctrl Pts',(0.402547883306248,4.06924497414062,13.4888135766353));
#34971=CARTESIAN_POINT('Ctrl Pts',(-3.20651703574811,2.53752792247832,13.6877465149988));
#34972=CARTESIAN_POINT('Ctrl Pts',(-3.86781631267568,-1.32695004777861,
13.8866794533622));
#34973=CARTESIAN_POINT('Ctrl Pts',(-0.973414525350525,-3.97155682569729,
14.0856123917256));
#34974=CARTESIAN_POINT('Ctrl Pts',(2.81585164640969,-2.96509341561348,14.284545330089));
#34975=CARTESIAN_POINT('Ctrl Pts',(4.01649263886463,0.767193808531516,14.4834782684525));
#34976=CARTESIAN_POINT('Ctrl Pts',(1.52475374663538,3.79419628775648,14.6824112068159));
#34977=CARTESIAN_POINT('Ctrl Pts',(-2.36869817469211,3.33317692526415,14.8813441451794));
#34978=CARTESIAN_POINT('Ctrl Pts',(-4.08459512965621,-0.192047089777438,
15.0802770835428));
#34979=CARTESIAN_POINT('Ctrl Pts',(-2.04550527152725,-3.54072134487557,
15.2792100219063));
#34980=CARTESIAN_POINT('Ctrl Pts',(1.87402685245334,-3.63439442193429,15.4781429602697));
#34981=CARTESIAN_POINT('Ctrl Pts',(4.07075759833579,-0.386952236709728,
15.6770758986331));
#34982=CARTESIAN_POINT('Ctrl Pts',(2.52522243637638,3.21621689329631,15.8760088369966));
#34983=CARTESIAN_POINT('Ctrl Pts',(-1.34176115504296,3.86270325817569,16.07494177536));
#34984=CARTESIAN_POINT('Ctrl Pts',(-3.97525763609332,0.958189012974472,
16.2738747137235));
#34985=CARTESIAN_POINT('Ctrl Pts',(-2.95428175737412,-2.8271927341357,16.4728076520868));
#34986=CARTESIAN_POINT('Ctrl Pts',(0.782578728991608,-4.01352338859924,
16.6717405904503));
#34987=CARTESIAN_POINT('Ctrl Pts',(3.80001104333727,-1.51020380360336,16.8706735288137));
#34988=CARTESIAN_POINT('Ctrl Pts',(3.3240759848093,2.38145298192455,17.0696064671772));
#34989=CARTESIAN_POINT('Ctrl Pts',(-0.207697190464619,4.08382924899859,
17.2685394055406));
#34990=CARTESIAN_POINT('Ctrl Pts',(-3.54853339731083,2.03192278053888,17.4674723439041));
#34991=CARTESIAN_POINT('Ctrl Pts',(-3.62718677091157,-1.88793950825425,
17.6664052822675));
#34992=CARTESIAN_POINT('Ctrl Pts',(-0.37135090847757,-4.07221045142267,
17.8653382206309));
#34993=CARTESIAN_POINT('Ctrl Pts',(3.22586952699263,-2.51287987232251,18.0642711589944));
#34994=CARTESIAN_POINT('Ctrl Pts',(3.85753348743574,1.35655256116935,18.2632040973578));
#34995=CARTESIAN_POINT('Ctrl Pts',(0.942949431467649,3.97890007760914,18.4621370357212));
#34996=CARTESIAN_POINT('Ctrl Pts',(-2.83849231006808,2.94342672128722,18.6610699740847));
#34997=CARTESIAN_POINT('Ctrl Pts',(-4.01049520759558,-0.797952158814143,
18.8600029124481));
#34998=CARTESIAN_POINT('Ctrl Pts',(-1.49563168618331,-3.80577000319091,
19.0589358508116));
#34999=CARTESIAN_POINT('Ctrl Pts',(2.3941728221794,-3.31492623680237,19.257868789175));
#35000=CARTESIAN_POINT('Ctrl Pts',(4.08300340529871,0.223344241524889,19.4568017275385));
#35001=CARTESIAN_POINT('Ctrl Pts',(2.01831045474011,3.55629334647608,19.6557346659019));
#35002=CARTESIAN_POINT('Ctrl Pts',(-1.90182444335736,3.61992586174797,19.8546676042653));
#35003=CARTESIAN_POINT('Ctrl Pts',(-4.07360351206664,0.355744127683883,
20.0536005426287));
#35004=CARTESIAN_POINT('Ctrl Pts',(-2.5005004115443,-3.23547479510659,20.2525334809922));
#35005=CARTESIAN_POINT('Ctrl Pts',(1.37132404897559,-3.85230707636404,20.4514664193556));
#35006=CARTESIAN_POINT('Ctrl Pts',(3.98248409676232,-0.927696004593339,
20.6503993577191));
#35007=CARTESIAN_POINT('Ctrl Pts',(2.93252846673791,2.84975020829459,20.8493322960825));
#35008=CARTESIAN_POINT('Ctrl Pts',(-0.813313872270502,4.00740814031659,
21.0482652344459));
#35009=CARTESIAN_POINT('Ctrl Pts',(-3.8114730827583,1.48103760833823,21.2471981728094));
#35010=CARTESIAN_POINT('Ctrl Pts',(-3.30572781558952,-2.40685750869074,
21.4461311111728));
#35011=CARTESIAN_POINT('Ctrl Pts',(0.238988013211991,-4.0821176106825,21.6450640495362));
#35012=CARTESIAN_POINT('Ctrl Pts',(3.56400107843168,-2.00466849400123,21.8439969878997));
#35013=CARTESIAN_POINT('Ctrl Pts',(3.61261180105568,1.91568145388957,22.0429299262631));
#35014=CARTESIAN_POINT('Ctrl Pts',(0.340132123483712,4.0749367598133,22.2418628646266));
#35015=CARTESIAN_POINT('Ctrl Pts',(-3.24503255660361,2.48808423580994,22.44079580299));
#35016=CARTESIAN_POINT('Ctrl Pts',(-3.84702410170021,-1.38607540157123,
22.6397287413534));
#35017=CARTESIAN_POINT('Ctrl Pts',(-0.912428956318338,-3.98600964092851,
22.8386616797169));
#35018=CARTESIAN_POINT('Ctrl Pts',(2.86096626351498,-2.92158715374577,23.0375946180803));
#35019=CARTESIAN_POINT('Ctrl Pts',(4.00426223208981,0.828663643803887,23.2365275564438));
#35020=CARTESIAN_POINT('Ctrl Pts',(1.46642178435367,3.81712019830084,23.4354604948072));
#35021=CARTESIAN_POINT('Ctrl Pts',(-2.4195068552087,3.29648085623159,23.6343934331707));
#35022=CARTESIAN_POINT('Ctrl Pts',(-4.08117187815611,-0.254628275827654,
23.8333263715341));
#35023=CARTESIAN_POINT('Ctrl Pts',(-1.99099709862783,-3.57165648000459,
24.0322593098975));
#35024=CARTESIAN_POINT('Ctrl Pts',(1.92951033638773,-3.60524469622744,24.2311922482609));
#35025=CARTESIAN_POINT('Ctrl Pts',(4.07621017508652,-0.324515125108852,
24.4301251866244));
#35026=CARTESIAN_POINT('Ctrl Pts',(2.47563152742672,3.2545426711466,24.6290581249878));
#35027=CARTESIAN_POINT('Ctrl Pts',(-1.40080640236154,3.84168464101443,24.8279910633513));
#35028=CARTESIAN_POINT('Ctrl Pts',(-3.98947665834203,0.897148510809323,
25.0269240017147));
#35029=CARTESIAN_POINT('Ctrl Pts',(-2.91060294296254,-2.8721403110435,25.2258569400782));
#35030=CARTESIAN_POINT('Ctrl Pts',(0.844001248033056,-4.00105752910675,
25.4247898784416));
#35031=CARTESIAN_POINT('Ctrl Pts',(3.82271126690174,-1.45178442883431,25.623722816805));
#35032=CARTESIAN_POINT('Ctrl Pts',(3.28718549450203,2.43212067600246,25.8226557551684));
#35033=CARTESIAN_POINT('Ctrl Pts',(-0.270264799725342,4.08016622160577,
26.0215886935319));
#35034=CARTESIAN_POINT('Ctrl Pts',(-3.57925943879032,1.97729646935751,26.2205216318953));
#35035=CARTESIAN_POINT('Ctrl Pts',(-3.59782465543471,-1.94331088780188,
26.4194545702588));
#35036=CARTESIAN_POINT('Ctrl Pts',(-0.308893361864258,-4.07742373918868,
26.6183875086222));
#35037=CARTESIAN_POINT('Ctrl Pts',(3.26400499909824,-2.46314246923822,26.8173204469857));
#35038=CARTESIAN_POINT('Ctrl Pts',(3.83628877270618,1.41551683505063,27.016253385349));
#35039=CARTESIAN_POINT('Ctrl Pts',(0.881854892429735,3.99288509809649,27.2151863237125));
#35040=CARTESIAN_POINT('Ctrl Pts',(-2.88327218681108,2.89957599566987,27.4141192620759));
#35041=CARTESIAN_POINT('Ctrl Pts',(-3.99779407842222,-0.859326459755243,
27.6130522004394));
#35042=CARTESIAN_POINT('Ctrl Pts',(-1.43712575670111,-3.82824620646707,
27.8119851388028));
#35043=CARTESIAN_POINT('Ctrl Pts',(2.44469878586269,-3.2778418668851,28.0109180771663));
#35044=CARTESIAN_POINT('Ctrl Pts',(4.07910065579756,0.285897355313241,28.2098510155297));
#35045=CARTESIAN_POINT('Ctrl Pts',(1.96356680735725,3.58680984315424,28.4087839538932));
#35046=CARTESIAN_POINT('Ctrl Pts',(-1.95708290549785,3.59035178762629,28.6077168922566));
#35047=CARTESIAN_POINT('Ctrl Pts',(-4.07857743430098,0.293267063125026,
28.80664983062));
#35048=CARTESIAN_POINT('Ctrl Pts',(-2.45061724462188,-3.27341940152267,
29.0055827689835));
#35049=CARTESIAN_POINT('Ctrl Pts',(1.43020648364449,-3.83083657600328,29.2045157073469));
#35050=CARTESIAN_POINT('Ctrl Pts',(3.99623491014561,-0.866548325736514,
29.4034486457103));
#35051=CARTESIAN_POINT('Ctrl Pts',(2.88850647377694,2.89436172736787,29.6023815840738));
#35052=CARTESIAN_POINT('Ctrl Pts',(-0.874639053949637,3.9944719279536,29.8013145224372));
#35053=CARTESIAN_POINT('Ctrl Pts',(-3.83372493572705,1.42244598318807,30.0002474608007));
#35054=CARTESIAN_POINT('Ctrl Pts',(-3.26845011057368,-2.45724100010441,
30.1991803991641));
#35055=CARTESIAN_POINT('Ctrl Pts',(0.301525713057809,-4.07797519637728,
30.3981133375275));
#35056=CARTESIAN_POINT('Ctrl Pts',(3.59430758223343,-1.94980831422029,30.5970462758909));
#35057=CARTESIAN_POINT('Ctrl Pts',(3.58282620252664,1.97082618726046,30.7959792142544));
#35058=CARTESIAN_POINT('Ctrl Pts',(0.277636458332829,4.07967124348368,30.9949121526178));
#35059=CARTESIAN_POINT('Ctrl Pts',(-3.2827857401879,2.4380560374861,31.1938450909813));
#35060=CARTESIAN_POINT('Ctrl Pts',(-3.82532813096051,-1.44487513245452,
31.3927780293447));
#35061=CARTESIAN_POINT('Ctrl Pts',(-0.851229035476529,-3.99952604530396,
31.5917109677081));
#35062=CARTESIAN_POINT('Ctrl Pts',(2.90540876988572,-2.877394539818,31.7906439060716));
#35063=CARTESIAN_POINT('Ctrl Pts',(3.99109112648016,0.889938805780879,31.989576844435));
#35064=CARTESIAN_POINT('Ctrl Pts',(1.4077453238388,3.83914737423731,32.1885097827985));
#35065=CARTESIAN_POINT('Ctrl Pts',(-2.46974713456985,3.25901036346728,32.3874427211619));
#35066=CARTESIAN_POINT('Ctrl Pts',(-4.07678985987002,-0.317149643487198,
32.5863756595253));
#35067=CARTESIAN_POINT('Ctrl Pts',(-1.93602119196322,-3.60175254593826,
32.7853085978888));
#35068=CARTESIAN_POINT('Ctrl Pts',(1.98454053129662,-3.57524801063428,32.9842415362522));
#35069=CARTESIAN_POINT('Ctrl Pts',(4.08070515067628,-0.262001776992349,
33.1831744746156));
#35070=CARTESIAN_POINT('Ctrl Pts',(2.42545903226761,3.29210387756742,33.3821074129791));
#35071=CARTESIAN_POINT('Ctrl Pts',(-1.45952256610013,3.81976351845869,33.5810403513425));
#35072=CARTESIAN_POINT('Ctrl Pts',(-4.00275845524774,0.835897246583656,
33.7799732897059));
#35073=CARTESIAN_POINT('Ctrl Pts',(-2.86624035694998,-2.91641315216041,
33.9789062280695));
#35074=CARTESIAN_POINT('Ctrl Pts',(0.905225490601913,-3.98765172364236,
34.1778391664328));
#35075=CARTESIAN_POINT('Ctrl Pts',(3.84451344237989,-1.3930239945038,34.3767721047963));
#35076=CARTESIAN_POINT('Ctrl Pts',(3.24952276417025,2.48221700563069,34.5757050431597));
#35077=CARTESIAN_POINT('Ctrl Pts',(-0.332768917194808,4.07554466368054,
34.7746379815232));
#35078=CARTESIAN_POINT('Ctrl Pts',(-3.60914462495387,1.92220564302213,34.9735709198866));
#35079=CARTESIAN_POINT('Ctrl Pts',(-3.56761732322031,-1.99822573623664,
35.17250385825));
#35080=CARTESIAN_POINT('Ctrl Pts',(-0.246363248667963,-4.08167914070044,
35.3714367966135));
#35081=CARTESIAN_POINT('Ctrl Pts',(3.30137367684192,-2.41282641392402,35.5703697349769));
#35082=CARTESIAN_POINT('Ctrl Pts',(3.81414282020493,1.47414856950349,35.7693026733403));
#35083=CARTESIAN_POINT('Ctrl Pts',(0.820553184171816,4.00593209253256,35.9682356117038));
#35084=CARTESIAN_POINT('Ctrl Pts',(-2.9273747126076,2.8550440889171,36.1671685500672));
#35085=CARTESIAN_POINT('Ctrl Pts',(-3.98415376995365,-0.920498883894049,
36.3661014884307));
#35086=CARTESIAN_POINT('Ctrl Pts',(-1.37828221131289,-3.849823061487,36.5650344267941));
#35087=CARTESIAN_POINT('Ctrl Pts',(2.49465043014533,-3.23998745175455,36.7639673651575));
#35088=CARTESIAN_POINT('Ctrl Pts',(4.07423962618006,0.348383304391666,36.962900303521));
#35089=CARTESIAN_POINT('Ctrl Pts',(1.90836187008279,3.61648371160565,37.1618332418844));
#35090=CARTESIAN_POINT('Ctrl Pts',(-2.01188160081678,3.55993425067045,37.3607661802478));
#35091=CARTESIAN_POINT('Ctrl Pts',(-4.08259319987495,0.230721106156537,
37.5596991186113));
#35092=CARTESIAN_POINT('Ctrl Pts',(-2.40015836675168,-3.31059500799247,
37.7586320569747));
#35093=CARTESIAN_POINT('Ctrl Pts',(1.48875292563011,-3.8084661070492,37.9575649953382));
#35094=CARTESIAN_POINT('Ctrl Pts',(4.00904691493279,-0.805197095935613,
38.1564979337016));
#35095=CARTESIAN_POINT('Ctrl Pts',(2.84380589172842,2.93829333322945,38.3554308720651));
#35096=CARTESIAN_POINT('Ctrl Pts',(-0.935758745314963,3.9805972344063,38.5543638104285));
#35097=CARTESIAN_POINT('Ctrl Pts',(-3.85507618443849,1.3635203486794,38.7532967487919));
#35098=CARTESIAN_POINT('Ctrl Pts',(-3.23040450708304,-2.50704752847379,
38.9522296871554));
#35099=CARTESIAN_POINT('Ctrl Pts',(0.363992462388689,-4.07287418561517,
39.1511626255188));
#35100=CARTESIAN_POINT('Ctrl Pts',(3.62376991564507,-1.8944911904441,39.3500955638822));
#35101=CARTESIAN_POINT('Ctrl Pts',(3.55219848867015,2.02551006091971,39.5490285022457));
#35102=CARTESIAN_POINT('Ctrl Pts',(0.215076379060282,4.08344321778653,39.7479614406091));
#35103=CARTESIAN_POINT('Ctrl Pts',(-3.31976926965591,2.38746293362043,39.9468943789726));
#35104=CARTESIAN_POINT('Ctrl Pts',(-3.80273052050235,-1.50335048727303,
40.145827317336));
#35105=CARTESIAN_POINT('Ctrl Pts',(-0.789834848961668,-4.01207398204883,
40.3447602556994));
#35106=CARTESIAN_POINT('Ctrl Pts',(2.94917967271135,-2.83258134221006,40.5436931940629));
#35107=CARTESIAN_POINT('Ctrl Pts',(3.97696142147388,0.951111115579423,40.7426261324263));
#35108=CARTESIAN_POINT('Ctrl Pts',(1.34877841142462,3.86006894220613,40.9415590707897));
#35109=CARTESIAN_POINT('Ctrl Pts',(-2.51948441896513,3.22116494326784,41.1404920091532));
#35110=CARTESIAN_POINT('Ctrl Pts',(-4.07130205620617,-0.380346269017061,
41.3394249475166));
#35111=CARTESIAN_POINT('Ctrl Pts',(-1.88087422963442,-3.62955985044473,
41.5383578858801));
#35112=CARTESIAN_POINT('Ctrl Pts',(2.0396473123645,-3.54722160642478,41.7372908242435));
#35113=CARTESIAN_POINT('Ctrl Pts',(4.08365574488659,-0.19291304504628,41.9362669284183));
#35114=CARTESIAN_POINT('Ctrl Pts',(2.94480488286648,2.14655679302897,42.0689320531386));
#35115=CARTESIAN_POINT('Ctrl Pts',(2.00570496136574,2.81548347365039,42.1352861984045));
#35116=CARTESIAN_POINT('Ctrl Pts',(1.6435788288222,-3.31109949314964,6.86350499875044));
#35117=CARTESIAN_POINT('Ctrl Pts',(2.74721907371341,-2.76326946119434,6.92981597820492));
#35118=CARTESIAN_POINT('Ctrl Pts',(4.34414919481839,-0.486393044209725,
7.06243793711388));
#35119=CARTESIAN_POINT('Ctrl Pts',(2.75379312724547,3.40034806728253,7.26137087547732));
#35120=CARTESIAN_POINT('Ctrl Pts',(-1.37188000734597,4.15061578131742,7.46030381384076));
#35121=CARTESIAN_POINT('Ctrl Pts',(-4.23445827724675,1.09043987287385,7.65923675220419));
#35122=CARTESIAN_POINT('Ctrl Pts',(-3.2052772200551,-2.97488551610267,7.85816969056764));
#35123=CARTESIAN_POINT('Ctrl Pts',(0.771049403037938,-4.30397858890673,
8.05710262893107));
#35124=CARTESIAN_POINT('Ctrl Pts',(4.03827586239305,-1.67713777828685,8.25603556729451));
#35125=CARTESIAN_POINT('Ctrl Pts',(3.59323830599447,2.49188565388108,8.45496850565795));
#35126=CARTESIAN_POINT('Ctrl Pts',(-0.155153181914435,4.36990798398716,
8.65390144402138));
#35127=CARTESIAN_POINT('Ctrl Pts',(-3.76087322949614,2.23075804087219,8.85283438238483));
#35128=CARTESIAN_POINT('Ctrl Pts',(-3.90922550655774,-1.95919207824947,
9.05176732074826));
#35129=CARTESIAN_POINT('Ctrl Pts',(-0.463798613632033,-4.34801977857419,
9.2507002591117));
#35130=CARTESIAN_POINT('Ctrl Pts',(3.40799499944848,-2.73970792995919,9.44963319747514));
#35131=CARTESIAN_POINT('Ctrl Pts',(4.14680620577778,1.38723751938316,9.64856613583857));
#35132=CARTESIAN_POINT('Ctrl Pts',(1.07343819364456,4.23888522314733,9.84749907420202));
#35133=CARTESIAN_POINT('Ctrl Pts',(-2.9867456421098,3.19370862133198,10.0464320125655));
#35134=CARTESIAN_POINT('Ctrl Pts',(-4.30120107661137,-0.787459878855247,
10.2453649509289));
#35135=CARTESIAN_POINT('Ctrl Pts',(-1.66154265936265,-4.04471237562304,
10.4442978892923));
#35136=CARTESIAN_POINT('Ctrl Pts',(2.50557934483546,-3.58364275211452,10.6432308276558));
#35137=CARTESIAN_POINT('Ctrl Pts',(4.36931095975112,0.171886048121829,10.8421637660192));
#35138=CARTESIAN_POINT('Ctrl Pts',(2.21631517892575,3.76939914480685,11.0410967043827));
#35139=CARTESIAN_POINT('Ctrl Pts',(-1.97414917416402,3.90168656767488,11.2400296427461));
#35140=CARTESIAN_POINT('Ctrl Pts',(-4.34976925317394,0.447135825469514,
11.4389625811095));
#35141=CARTESIAN_POINT('Ctrl Pts',(-2.72662674141349,-3.41846889597808,
11.6378955194729));
#35142=CARTESIAN_POINT('Ctrl Pts',(1.40311608794153,-4.14145967563326,11.8368284578364));
#35143=CARTESIAN_POINT('Ctrl Pts',(4.24296794021624,-1.057187804276,12.0357613961998));
#35144=CARTESIAN_POINT('Ctrl Pts',(3.18224013634397,2.99896160485262,12.2346943345633));
#35145=CARTESIAN_POINT('Ctrl Pts',(-0.803935445702029,4.29815202091405,
12.4336272729267));
#35146=CARTESIAN_POINT('Ctrl Pts',(-4.05104952943537,1.64603180552031,12.6325602112902));
#35147=CARTESIAN_POINT('Ctrl Pts',(-3.57401542229434,-2.51929290787779,
12.8314931496536));
#35148=CARTESIAN_POINT('Ctrl Pts',(0.18862725909364,-4.36862023435567,13.030426088017));
#35149=CARTESIAN_POINT('Ctrl Pts',(3.77786404640665,-2.20185518179452,13.2293590263804));
#35150=CARTESIAN_POINT('Ctrl Pts',(3.89409329547718,1.98908531763447,13.4282919647439));
#35151=CARTESIAN_POINT('Ctrl Pts',(0.430464930930045,4.35145067052408,13.6272249031073));
#35152=CARTESIAN_POINT('Ctrl Pts',(-3.42889179538761,2.71350770226696,13.8261578414708));
#35153=CARTESIAN_POINT('Ctrl Pts',(-4.13605275529299,-1.4189751936421,14.0250907798342));
#35154=CARTESIAN_POINT('Ctrl Pts',(-1.04092167366474,-4.246987763585,14.2240237181976));
#35155=CARTESIAN_POINT('Ctrl Pts',(3.01113341976998,-3.17072523613856,14.4229566565611));
#35156=CARTESIAN_POINT('Ctrl Pts',(4.29503991467939,0.820399369851541,14.6218895949245));
#35157=CARTESIAN_POINT('Ctrl Pts',(1.63049675193903,4.05732711728536,14.820822533288));
#35158=CARTESIAN_POINT('Ctrl Pts',(-2.53296946387702,3.56433565897051,15.0197554716514));
#35159=CARTESIAN_POINT('Ctrl Pts',(-4.36786537274413,-0.205365723345486,
15.2186884100148));
#35160=CARTESIAN_POINT('Ctrl Pts',(-2.18736285033501,-3.7862734655221,15.4176213483783));
#35161=CARTESIAN_POINT('Ctrl Pts',(2.00399225298804,-3.88644285236594,15.6165542867417));
#35162=CARTESIAN_POINT('Ctrl Pts',(4.35306819652955,-0.41378771260799,15.8154872251052));
#35163=CARTESIAN_POINT('Ctrl Pts',(2.70034881994612,3.43926434653661,16.0144201634686));
#35164=CARTESIAN_POINT('Ctrl Pts',(-1.43481346414344,4.13058510599347,16.213353101832));
#35165=CARTESIAN_POINT('Ctrl Pts',(-4.25094522841732,1.02464025869492,16.4122860401955));
#35166=CARTESIAN_POINT('Ctrl Pts',(-3.15916377994851,-3.02326102184444,
16.6112189785589));
#35167=CARTESIAN_POINT('Ctrl Pts',(0.836851247995388,-4.29186474431231,
16.8101519169224));
#35168=CARTESIAN_POINT('Ctrl Pts',(4.06354513124908,-1.61493775763784,17.0090848552858));
#35169=CARTESIAN_POINT('Ctrl Pts',(3.55460356033887,2.54660882814157,17.2080177936493));
#35170=CARTESIAN_POINT('Ctrl Pts',(-0.222101172196999,4.36704637759334,
17.4069507320126));
#35171=CARTESIAN_POINT('Ctrl Pts',(-3.79462729062322,2.17283840172248,17.6058836703761));
#35172=CARTESIAN_POINT('Ctrl Pts',(-3.87873534444371,-2.0188697636315,17.8048166087395));
#35173=CARTESIAN_POINT('Ctrl Pts',(-0.397104418623892,-4.35462180624813,
18.003749547103));
#35174=CARTESIAN_POINT('Ctrl Pts',(3.44958639881833,-2.68715028828496,18.2026824854664));
#35175=CARTESIAN_POINT('Ctrl Pts',(4.12505680713318,1.45063066721568,18.4016154238299));
#35176=CARTESIAN_POINT('Ctrl Pts',(1.00834379888781,4.25484027643657,18.6005483621933));
#35177=CARTESIAN_POINT('Ctrl Pts',(-3.03534423324606,3.14755593761926,18.7994813005568));
#35178=CARTESIAN_POINT('Ctrl Pts',(-4.28862655630873,-0.853290838615923,
18.9984142389201));
#35179=CARTESIAN_POINT('Ctrl Pts',(-1.59935505113543,-4.06970348000317,
19.1973471772837));
#35180=CARTESIAN_POINT('Ctrl Pts',(2.56021080043808,-3.54481926930875,19.396280115647));
#35181=CARTESIAN_POINT('Ctrl Pts',(4.36616326091091,0.238833359927311,19.5952130540105));
#35182=CARTESIAN_POINT('Ctrl Pts',(2.15828204922935,3.802925399047,19.7941459923739));
#35183=CARTESIAN_POINT('Ctrl Pts',(-2.03371763112254,3.87097088488195,19.9930789307374));
#35184=CARTESIAN_POINT('Ctrl Pts',(-4.3561114768656,0.380415293938357,20.1920118691008));
#35185=CARTESIAN_POINT('Ctrl Pts',(-2.67391230107938,-3.45985780067314,
20.3909448074643));
#35186=CARTESIAN_POINT('Ctrl Pts',(1.46642657061485,-4.11946793988461,20.5898777458277));
#35187=CARTESIAN_POINT('Ctrl Pts',(4.25867285045125,-0.992032533524869,
20.7888106841911));
#35188=CARTESIAN_POINT('Ctrl Pts',(3.13590187958944,3.0473828765565,20.9877436225545));
#35189=CARTESIAN_POINT('Ctrl Pts',(-0.869717900330041,4.28532539821516,
21.186676560918));
#35190=CARTESIAN_POINT('Ctrl Pts',(-4.07580207312432,1.58374886123332,21.3856094992814));
#35191=CARTESIAN_POINT('Ctrl Pts',(-3.53498292954331,-2.57377518104822,
21.5845424376449));
#35192=CARTESIAN_POINT('Ctrl Pts',(0.255562040857054,-4.36521603566368,
21.7834753760083));
#35193=CARTESIAN_POINT('Ctrl Pts',(3.81116766895198,-2.14369400658712,21.9824083143717));
#35194=CARTESIAN_POINT('Ctrl Pts',(3.86314958768654,2.04853563744927,22.1813412527352));
#35195=CARTESIAN_POINT('Ctrl Pts',(0.363720583598531,4.35753718650904,22.3802741910986));
#35196=CARTESIAN_POINT('Ctrl Pts',(-3.47007840128558,2.66063505270333,22.5792071294621));
#35197=CARTESIAN_POINT('Ctrl Pts',(-4.11381858630935,-1.48220094240897,
22.7781400678255));
#35198=CARTESIAN_POINT('Ctrl Pts',(-0.975706702105193,-4.26244289418747,
22.9770730061889));
#35199=CARTESIAN_POINT('Ctrl Pts',(3.05937677501175,-3.12420177697617,23.1760059445524));
#35200=CARTESIAN_POINT('Ctrl Pts',(4.28196131850264,0.886132191938384,23.3749388829158));
#35201=CARTESIAN_POINT('Ctrl Pts',(1.56811941707795,4.08184082106659,23.5738718212792));
#35202=CARTESIAN_POINT('Ctrl Pts',(-2.58730177080555,3.52509468547,23.7728047596427));
#35203=CARTESIAN_POINT('Ctrl Pts',(-4.3642047157598,-0.272286969358187,
23.9717376980061));
#35204=CARTESIAN_POINT('Ctrl Pts',(-2.12907448799273,-3.81935397931651,
24.1706706363695));
#35205=CARTESIAN_POINT('Ctrl Pts',(2.06332356503822,-3.85527156769798,24.369603574733));
#35206=CARTESIAN_POINT('Ctrl Pts',(4.3588989142447,-0.347020532733638,24.5685365130964));
#35207=CARTESIAN_POINT('Ctrl Pts',(2.6473187381073,3.4802480505861,24.7674694514599));
#35208=CARTESIAN_POINT('Ctrl Pts',(-1.49795355098226,4.10810882935714,24.9664023898233));
#35209=CARTESIAN_POINT('Ctrl Pts',(-4.26615035228957,0.959366544341607,
25.1653353281867));
#35210=CARTESIAN_POINT('Ctrl Pts',(-3.11245580157246,-3.07132575250498,
25.3642682665502));
#35211=CARTESIAN_POINT('Ctrl Pts',(0.902533472429329,-4.27853436656609,
25.5632012049136));
#35212=CARTESIAN_POINT('Ctrl Pts',(4.0878196351628,-1.55246694815701,25.7621341432771));
#35213=CARTESIAN_POINT('Ctrl Pts',(3.51515468227829,2.60079037109864,25.9610670816405));
#35214=CARTESIAN_POINT('Ctrl Pts',(-0.289007899857984,4.36312931604853,
26.160000020004));
#35215=CARTESIAN_POINT('Ctrl Pts',(-3.8274842099407,2.11442370810511,26.3589329583674));
#35216=CARTESIAN_POINT('Ctrl Pts',(-3.8473369405895,-2.07808119675769,26.5578658967308));
#35217=CARTESIAN_POINT('Ctrl Pts',(-0.330315386551131,-4.36019664007829,
26.7567988350943));
#35218=CARTESIAN_POINT('Ctrl Pts',(3.49036659925336,-2.6339635528152,26.9557317734577));
#35219=CARTESIAN_POINT('Ctrl Pts',(4.10233875286451,1.51368416503854,27.1546647118211));
#35220=CARTESIAN_POINT('Ctrl Pts',(0.943012300157368,4.26979517032074,27.3535976501846));
#35221=CARTESIAN_POINT('Ctrl Pts',(-3.08322963358878,3.10066412584504,27.552530588548));
#35222=CARTESIAN_POINT('Ctrl Pts',(-4.27504459272359,-0.9189215009821,27.7514635269115));
#35223=CARTESIAN_POINT('Ctrl Pts',(-1.53679168429643,-4.09373842762575,
27.9503964652748));
#35224=CARTESIAN_POINT('Ctrl Pts',(2.61424078387375,-3.50516306591769,28.1493294036383));
#35225=CARTESIAN_POINT('Ctrl Pts',(4.36198985231999,0.305724586842239,28.3482623420017));
#35226=CARTESIAN_POINT('Ctrl Pts',(2.09974188204234,3.835558241448,28.5471952803652));
#35227=CARTESIAN_POINT('Ctrl Pts',(-2.09280831592068,3.83934582286561,28.7461282187286));
#35228=CARTESIAN_POINT('Ctrl Pts',(-4.36143034495521,0.313605390333471,
28.9450611570921));
#35229=CARTESIAN_POINT('Ctrl Pts',(-2.62056969292188,-3.50043389871622,
29.1439940954555));
#35230=CARTESIAN_POINT('Ctrl Pts',(1.52939255360441,-4.09650844155383,29.342927033819));
#35231=CARTESIAN_POINT('Ctrl Pts',(4.27337729476395,-0.926644209682624,
29.5418599721824));
#35232=CARTESIAN_POINT('Ctrl Pts',(3.08882692293162,3.09508824347791,29.7407929105458));
#35233=CARTESIAN_POINT('Ctrl Pts',(-0.935296036970499,4.27149204821567,
29.9397258489092));
#35234=CARTESIAN_POINT('Ctrl Pts',(-4.09959711154953,1.52109385565686,30.1386587872727));
#35235=CARTESIAN_POINT('Ctrl Pts',(-3.49511998309561,-2.62765281163783,
30.3375917256362));
#35236=CARTESIAN_POINT('Ctrl Pts',(0.322436784859063,-4.360786341305,30.5365246639996));
#35237=CARTESIAN_POINT('Ctrl Pts',(3.84357595528703,-2.08502922537836,30.735457602363));
#35238=CARTESIAN_POINT('Ctrl Pts',(3.83129833186026,2.10750470628822,30.9343905407264));
#35239=CARTESIAN_POINT('Ctrl Pts',(0.296890789434302,4.36260001076095,31.1333234790899));
#35240=CARTESIAN_POINT('Ctrl Pts',(-3.51044980115615,2.60713735508994,31.3322564174533));
#35241=CARTESIAN_POINT('Ctrl Pts',(-4.09061798103173,-1.54507848603308,
31.5311893558168));
#35242=CARTESIAN_POINT('Ctrl Pts',(-0.910262513250637,-4.27689667302272,
31.7301222941802));
#35243=CARTESIAN_POINT('Ctrl Pts',(3.10690140805196,-3.07694436663831,31.9290552325437));
#35244=CARTESIAN_POINT('Ctrl Pts',(4.26787678520448,0.951656839966625,32.127988170907));
#35245=CARTESIAN_POINT('Ctrl Pts',(1.50537369273006,4.10539560091092,32.3269211092706));
#35246=CARTESIAN_POINT('Ctrl Pts',(-2.64102625746159,3.48502558127492,32.5258540476339));
#35247=CARTESIAN_POINT('Ctrl Pts',(-4.35951880067472,-0.339144248522522,
32.7247869859974));
#35248=CARTESIAN_POINT('Ctrl Pts',(-2.07028595413972,-3.85153723373335,
32.9237199243608));
#35249=CARTESIAN_POINT('Ctrl Pts',(2.12217015207268,-3.82319458573513,33.1226528627243));
#35250=CARTESIAN_POINT('Ctrl Pts',(4.36370562032123,-0.280171829274663,
33.3215858010877));
#35251=CARTESIAN_POINT('Ctrl Pts',(2.59366673654697,3.52041415950907,33.5205187394511));
#35252=CARTESIAN_POINT('Ctrl Pts',(-1.56074173200713,4.08466745778821,33.7194516778146));
#35253=CARTESIAN_POINT('Ctrl Pts',(-4.28035325342194,0.893867451394637,
33.9183846161781));
#35254=CARTESIAN_POINT('Ctrl Pts',(-3.06501663143715,-3.11866895385767,
34.1173175545414));
#35255=CARTESIAN_POINT('Ctrl Pts',(0.968003669743968,-4.26419885677308,
34.3162504929049));
#35256=CARTESIAN_POINT('Ctrl Pts',(4.11113381057032,-1.48963142633595,34.5151834312683));
#35257=CARTESIAN_POINT('Ctrl Pts',(3.47488000867237,2.65436092498193,34.7141163696317));
#35258=CARTESIAN_POINT('Ctrl Pts',(-0.355846732516481,4.35818724904092,
34.9130493079952));
#35259=CARTESIAN_POINT('Ctrl Pts',(-3.85944195989102,2.05551228480171,35.1119822463586));
#35260=CARTESIAN_POINT('Ctrl Pts',(-3.81503470347808,-2.13680443793921,
35.3109151847221));
#35261=CARTESIAN_POINT('Ctrl Pts',(-0.263448755339423,-4.36474715740505,
35.5098481230855));
#35262=CARTESIAN_POINT('Ctrl Pts',(3.53032682746711,-2.58015803507752,35.708781061449));
#35263=CARTESIAN_POINT('Ctrl Pts',(4.07865695919681,1.5763820615329,35.9077139998124));
#35264=CARTESIAN_POINT('Ctrl Pts',(0.87745926484041,4.28374698522694,36.1066469381758));
#35265=CARTESIAN_POINT('Ctrl Pts',(-3.13039070810472,3.05304389242815,36.3055798765393));
#35266=CARTESIAN_POINT('Ctrl Pts',(-4.26045831693806,-0.984336286213261,
36.5045128149027));
#35267=CARTESIAN_POINT('Ctrl Pts',(-1.47386728759316,-4.11681165640429,
36.7034457532661));
#35268=CARTESIAN_POINT('Ctrl Pts',(2.66765661835625,-3.46468341400465,36.9023786916296));
#35269=CARTESIAN_POINT('Ctrl Pts',(4.35679170604889,0.372543991115891,37.101311629993));
#35270=CARTESIAN_POINT('Ctrl Pts',(2.04070843410648,3.86729001861809,37.3002445683564));
#35271=CARTESIAN_POINT('Ctrl Pts',(-2.15140734866625,3.80681880313016,37.4991775067199));
#35272=CARTESIAN_POINT('Ctrl Pts',(-4.3657246073824,0.246721816570115,37.6981104450834));
#35273=CARTESIAN_POINT('Ctrl Pts',(-2.56661144775907,-3.54018766599446,
37.8970433834468));
#35274=CARTESIAN_POINT('Ctrl Pts',(1.59199924252436,-4.07258656102101,38.0959763218102));
#35275=CARTESIAN_POINT('Ctrl Pts',(4.28707782328367,-0.861038218460384,
38.2949092601736));
#35276=CARTESIAN_POINT('Ctrl Pts',(3.04102631643975,3.14206654461201,38.4938421985371));
#35277=CARTESIAN_POINT('Ctrl Pts',(-1.00065443236423,4.25665513254129,38.6927751369005));
#35278=CARTESIAN_POINT('Ctrl Pts',(-4.12242908802487,1.45808167688089,38.8917080752639));
#35279=CARTESIAN_POINT('Ctrl Pts',(-3.45443588374254,-2.68091346629163,
39.0906410136274));
#35280=CARTESIAN_POINT('Ctrl Pts',(0.389235657865896,-4.35533157098711,
39.2895739519908));
#35281=CARTESIAN_POINT('Ctrl Pts',(3.8750815272774,-2.02587581070879,39.4885068903542));
#35282=CARTESIAN_POINT('Ctrl Pts',(3.79854655927238,2.16598095439164,39.6874398287178));
#35283=CARTESIAN_POINT('Ctrl Pts',(0.22999211397275,4.36663357477926,39.8863727670811));
#35284=CARTESIAN_POINT('Ctrl Pts',(-3.5499981707246,2.55303557524153,40.0853057054446));
#35285=CARTESIAN_POINT('Ctrl Pts',(-4.06645320653296,-1.60760915782874,
40.284238643808));
#35286=CARTESIAN_POINT('Ctrl Pts',(-0.844610586228765,-4.29031482015054,
40.4831715821715));
#35287=CARTESIAN_POINT('Ctrl Pts',(3.15370786125407,-3.02902333459953,40.6821045205349));
#35288=CARTESIAN_POINT('Ctrl Pts',(4.2527671728035,1.01707150292793,40.8810374588983));
#35289=CARTESIAN_POINT('Ctrl Pts',(1.44231737338975,4.12776809790848,41.0799703972618));
#35290=CARTESIAN_POINT('Ctrl Pts',(-2.69421286601115,3.44455554809932,41.2789033356252));
#35291=CARTESIAN_POINT('Ctrl Pts',(-4.3536504130292,-0.406723615280815,
41.4778362739886));
#35292=CARTESIAN_POINT('Ctrl Pts',(-2.0113145017627,-3.88127299911711,41.6767692123521));
#35293=CARTESIAN_POINT('Ctrl Pts',(2.18109863658322,-3.79322452589238,41.8757021507155));
#35294=CARTESIAN_POINT('Ctrl Pts',(4.3668608408195,-0.206291733369188,42.0746782548904));
#35295=CARTESIAN_POINT('Ctrl Pts',(3.14902967590887,2.29542238319448,42.2073433796106));
#35296=CARTESIAN_POINT('Ctrl Pts',(2.14480235386948,3.01073971390795,42.2736975248765));
#35297=CARTESIAN_POINT('Ctrl Pts',(1.75017024926294,-3.52583503975451,7.00191632522251));
#35298=CARTESIAN_POINT('Ctrl Pts',(2.92538514533336,-2.94247645252568,7.06822730467699));
#35299=CARTESIAN_POINT('Ctrl Pts',(4.62588136680913,-0.517937211465701,
7.20084926358595));
#35300=CARTESIAN_POINT('Ctrl Pts',(2.93238554756965,3.6208716735304,7.39978220194938));
#35301=CARTESIAN_POINT('Ctrl Pts',(-1.46085087755489,4.41979668342923,7.59871514031282));
#35302=CARTESIAN_POINT('Ctrl Pts',(-4.5090766372874,1.16115843709268,7.79764807867627));
#35303=CARTESIAN_POINT('Ctrl Pts',(-3.4131498488579,-3.16781649528616,7.99658101703969));
#35304=CARTESIAN_POINT('Ctrl Pts',(0.821054458870111,-4.58310556675101,
8.19551395540314));
#35305=CARTESIAN_POINT('Ctrl Pts',(4.30017115622109,-1.78590560549867,8.39444689376657));
#35306=CARTESIAN_POINT('Ctrl Pts',(3.82627147014904,2.65349252467134,8.59337983213001));
#35307=CARTESIAN_POINT('Ctrl Pts',(-0.165215369231643,4.65331069704242,
8.79231277049345));
#35308=CARTESIAN_POINT('Ctrl Pts',(-4.00477806241297,2.37542993860311,8.99124570885689));
#35309=CARTESIAN_POINT('Ctrl Pts',(-4.16275146604314,-2.0862520420764,9.19017864722033));
#35310=CARTESIAN_POINT('Ctrl Pts',(-0.493877458746418,-4.63000297048149,
9.38911158558376));
#35311=CARTESIAN_POINT('Ctrl Pts',(3.62901453406151,-2.91738687953307,9.5880445239472));
#35312=CARTESIAN_POINT('Ctrl Pts',(4.41574004455383,1.47720437408262,9.78697746231064));
#35313=CARTESIAN_POINT('Ctrl Pts',(1.14305414379514,4.513790684995,9.98591040067408));
#35314=CARTESIAN_POINT('Ctrl Pts',(-3.18044578895083,3.40083098896765,10.1848433390375));
#35315=CARTESIAN_POINT('Ctrl Pts',(-4.58014792377031,-0.838529207295953,
10.3837762774009));
#35316=CARTESIAN_POINT('Ctrl Pts',(-1.76929909250628,-4.30702509822045,
10.5827092157644));
#35317=CARTESIAN_POINT('Ctrl Pts',(2.66807429591995,-3.81605361346254,10.7816421541278));
#35318=CARTESIAN_POINT('Ctrl Pts',(4.65267495384734,0.183033416110524,10.9805750924913));
#35319=CARTESIAN_POINT('Ctrl Pts',(2.36005041019255,4.01385691099803,11.1795080308547));
#35320=CARTESIAN_POINT('Ctrl Pts',(-2.10217915419658,4.15472360250998,11.3784409692181));
#35321=CARTESIAN_POINT('Ctrl Pts',(-4.63186590418606,0.476134034701025,
11.5773739075816));
#35322=CARTESIAN_POINT('Ctrl Pts',(-2.90345733346189,-3.6401676967687,11.776306845945));
#35323=CARTESIAN_POINT('Ctrl Pts',(1.49411271933775,-4.41004677458003,11.9752397843084));
#35324=CARTESIAN_POINT('Ctrl Pts',(4.51813817951421,-1.12574986394373,12.1741727226719));
#35325=CARTESIAN_POINT('Ctrl Pts',(3.38861873551307,3.19345399651813,12.3731056610353));
#35326=CARTESIAN_POINT('Ctrl Pts',(-0.856073268115742,4.57690112691687,
12.5720385993988));
#35327=CARTESIAN_POINT('Ctrl Pts',(-4.3137732370215,1.75278230945974,12.7709715377622));
#35328=CARTESIAN_POINT('Ctrl Pts',(-3.80580192006295,-2.68267722802591,
12.9699044761256));
#35329=CARTESIAN_POINT('Ctrl Pts',(0.200860348938858,-4.6519394326686,13.1688374144891));
#35330=CARTESIAN_POINT('Ctrl Pts',(4.0228707889351,-2.34465263532486,13.3677703528525));
#35331=CARTESIAN_POINT('Ctrl Pts',(4.14663788197017,2.11808395503869,13.566703291216));
#35332=CARTESIAN_POINT('Ctrl Pts',(0.458381978553845,4.63365636690753,13.7656362295794));
#35333=CARTESIAN_POINT('Ctrl Pts',(-3.65126655502712,2.88948748205561,13.9645691679428));
#35334=CARTESIAN_POINT('Ctrl Pts',(-4.4042891979103,-1.51100033950559,14.1635021063063));
#35335=CARTESIAN_POINT('Ctrl Pts',(-1.10842882197895,-4.52241870147271,
14.3624350446697));
#35336=CARTESIAN_POINT('Ctrl Pts',(3.20641519313028,-3.37635705666365,14.5613679830331));
#35337=CARTESIAN_POINT('Ctrl Pts',(4.57358719049415,0.873604931171569,14.7603009213966));
#35338=CARTESIAN_POINT('Ctrl Pts',(1.73623975724267,4.32045794681424,14.95923385976));
#35339=CARTESIAN_POINT('Ctrl Pts',(-2.69724075306194,3.79549439267688,15.1581667981235));
#35340=CARTESIAN_POINT('Ctrl Pts',(-4.65113561583202,-0.218684356913533,
15.3570997364869));
#35341=CARTESIAN_POINT('Ctrl Pts',(-2.32922042914278,-4.03182558616862,
15.5560326748503));
#35342=CARTESIAN_POINT('Ctrl Pts',(2.13395765352274,-4.13849128279759,15.7549656132138));
#35343=CARTESIAN_POINT('Ctrl Pts',(4.63537879472331,-0.44062318850625,15.9538985515772));
#35344=CARTESIAN_POINT('Ctrl Pts',(2.87547520351587,3.66231179977693,16.1528314899406));
#35345=CARTESIAN_POINT('Ctrl Pts',(-1.52786577324392,4.39846695381126,16.3517644283041));
#35346=CARTESIAN_POINT('Ctrl Pts',(-4.52663282074132,1.09109150441536,16.5506973666675));
#35347=CARTESIAN_POINT('Ctrl Pts',(-3.36404580252289,-3.21932930955316,
16.749630305031));
#35348=CARTESIAN_POINT('Ctrl Pts',(0.891123766999176,-4.57020610002538,
16.9485632433944));
#35349=CARTESIAN_POINT('Ctrl Pts',(4.32707921916088,-1.71967171167232,17.1474961817578));
#35350=CARTESIAN_POINT('Ctrl Pts',(3.78513113586845,2.7117646743586,17.3464291201213));
#35351=CARTESIAN_POINT('Ctrl Pts',(-0.236505153929377,4.65026350618809,
17.5453620584847));
#35352=CARTESIAN_POINT('Ctrl Pts',(-4.0407211839356,2.31375402290608,17.7442949968481));
#35353=CARTESIAN_POINT('Ctrl Pts',(-4.13028391797584,-2.14980001900876,
17.9432279352116));
#35354=CARTESIAN_POINT('Ctrl Pts',(-0.422857928770215,-4.63703316107358,
18.142160873575));
#35355=CARTESIAN_POINT('Ctrl Pts',(3.67330327064404,-2.86142070424742,18.3410938119385));
#35356=CARTESIAN_POINT('Ctrl Pts',(4.39258012683063,1.544708773262,18.5400267503019));
#35357=CARTESIAN_POINT('Ctrl Pts',(1.07373816630795,4.53078047526401,18.7389596886653));
#35358=CARTESIAN_POINT('Ctrl Pts',(-3.23219615642406,3.35168515395129,18.9378926270288));
#35359=CARTESIAN_POINT('Ctrl Pts',(-4.56675790502189,-0.9086295184177,19.1368255653922));
#35360=CARTESIAN_POINT('Ctrl Pts',(-1.70307841608756,-4.33363695681545,
19.3357585037557));
#35361=CARTESIAN_POINT('Ctrl Pts',(2.72624877869676,-3.77471230181512,19.5346914421191));
#35362=CARTESIAN_POINT('Ctrl Pts',(4.6493231165231,0.254322478329726,19.7336243804825));
#35363=CARTESIAN_POINT('Ctrl Pts',(2.2982536437186,4.04955745161791,19.932557318846));
#35364=CARTESIAN_POINT('Ctrl Pts',(-2.16561081888772,4.12201590801593,20.1314902572094));
#35365=CARTESIAN_POINT('Ctrl Pts',(-4.63861944166455,0.405086460192834,
20.3304231955728));
#35366=CARTESIAN_POINT('Ctrl Pts',(-2.84732419061446,-3.68424080623969,
20.5293561339363));
#35367=CARTESIAN_POINT('Ctrl Pts',(1.56152909225411,-4.38662880340519,20.7282890722997));
#35368=CARTESIAN_POINT('Ctrl Pts',(4.53486160414019,-1.05636906245639,20.9272220106632));
#35369=CARTESIAN_POINT('Ctrl Pts',(3.33927529244099,3.24501554481841,21.1261549490266));
#35370=CARTESIAN_POINT('Ctrl Pts',(-0.926121928389577,4.56324265611374,
21.32508788739));
#35371=CARTESIAN_POINT('Ctrl Pts',(-4.34013106349035,1.68646011412841,21.5240208257534));
#35372=CARTESIAN_POINT('Ctrl Pts',(-3.76423804349709,-2.74069285340571,
21.7229537641169));
#35373=CARTESIAN_POINT('Ctrl Pts',(0.272136068502114,-4.64831446064486,
21.9218867024803));
#35374=CARTESIAN_POINT('Ctrl Pts',(4.05833425947229,-2.282719519173,22.1208196408438));
#35375=CARTESIAN_POINT('Ctrl Pts',(4.1136873743174,2.18138982100898,22.3197525792072));
#35376=CARTESIAN_POINT('Ctrl Pts',(0.387309043713353,4.64013761320478,22.5186855175706));
#35377=CARTESIAN_POINT('Ctrl Pts',(-3.69512424596756,2.83318586959673,22.7176184559341));
#35378=CARTESIAN_POINT('Ctrl Pts',(-4.38061307091849,-1.5783264832467,22.9165513942975));
#35379=CARTESIAN_POINT('Ctrl Pts',(-1.03898444789204,-4.53887614744645,
23.115484332661));
#35380=CARTESIAN_POINT('Ctrl Pts',(3.25778728650852,-3.32681640020656,23.3144172710244));
#35381=CARTESIAN_POINT('Ctrl Pts',(4.55966040491547,0.943600740072882,23.5133502093879));
#35382=CARTESIAN_POINT('Ctrl Pts',(1.66981704980222,4.34656144383233,23.7122831477513));
#35383=CARTESIAN_POINT('Ctrl Pts',(-2.7550966864024,3.75370851470842,23.9112160861147));
#35384=CARTESIAN_POINT('Ctrl Pts',(-4.6472375533635,-0.289945662888717,
24.1101490244782));
#35385=CARTESIAN_POINT('Ctrl Pts',(-2.26715187735763,-4.06705147862843,
24.3090819628416));
#35386=CARTESIAN_POINT('Ctrl Pts',(2.19713679368869,-4.10529843916849,24.508014901205));
#35387=CARTESIAN_POINT('Ctrl Pts',(4.6415876534029,-0.369525940358427,24.7069478395685));
#35388=CARTESIAN_POINT('Ctrl Pts',(2.81900594878788,3.70595343002559,24.9058807779319));
#35389=CARTESIAN_POINT('Ctrl Pts',(-1.59510069960298,4.37453301769984,25.1048137162954));
#35390=CARTESIAN_POINT('Ctrl Pts',(-4.54282404623711,1.02158457787389,25.3037466546588));
#35391=CARTESIAN_POINT('Ctrl Pts',(-3.31430866018239,-3.27051119396646,
25.5026795930222));
#35392=CARTESIAN_POINT('Ctrl Pts',(0.961065696825607,-4.55601120402541,
25.7016125313856));
#35393=CARTESIAN_POINT('Ctrl Pts',(4.35292800342385,-1.65314946747969,25.9005454697491));
#35394=CARTESIAN_POINT('Ctrl Pts',(3.74312387005455,2.76946006619482,26.0994784081125));
#35395=CARTESIAN_POINT('Ctrl Pts',(-0.307750999990631,4.64609241049128,
26.298411346476));
#35396=CARTESIAN_POINT('Ctrl Pts',(-4.0757089810911,2.25155094685271,26.4973442848394));
#35397=CARTESIAN_POINT('Ctrl Pts',(-4.09684922574428,-2.21285150571349,
26.6962772232029));
#35398=CARTESIAN_POINT('Ctrl Pts',(-0.351737411238005,-4.64296954096788,
26.8952101615663));
#35399=CARTESIAN_POINT('Ctrl Pts',(3.71672819940849,-2.8047846363922,27.0941430999298));
#35400=CARTESIAN_POINT('Ctrl Pts',(4.36838873302285,1.61185149502644,27.2930760382932));
#35401=CARTESIAN_POINT('Ctrl Pts',(1.00416970788501,4.54670524254498,27.4920089766566));
#35402=CARTESIAN_POINT('Ctrl Pts',(-3.28318708036648,3.30175225602021,27.69094191502));
#35403=CARTESIAN_POINT('Ctrl Pts',(-4.55229510702496,-0.97851654220896,
27.8898748533835));
#35404=CARTESIAN_POINT('Ctrl Pts',(-1.63645761189174,-4.35923064878442,
28.0888077917469));
#35405=CARTESIAN_POINT('Ctrl Pts',(2.78378278188482,-3.7324842649503,28.2877407301104));
#35406=CARTESIAN_POINT('Ctrl Pts',(4.6448790488424,0.32555181837124,28.4866736684738));
#35407=CARTESIAN_POINT('Ctrl Pts',(2.23591695672744,4.08430663974176,28.6856066068372));
#35408=CARTESIAN_POINT('Ctrl Pts',(-2.22853372634353,4.08833985810493,28.8845395452007));
#35409=CARTESIAN_POINT('Ctrl Pts',(-4.64428325560944,0.333943717541912,
29.0834724835641));
#35410=CARTESIAN_POINT('Ctrl Pts',(-2.79052214122188,-3.72744839590976,
29.2824054219276));
#35411=CARTESIAN_POINT('Ctrl Pts',(1.62857862356433,-4.36218030710437,29.481338360291));
#35412=CARTESIAN_POINT('Ctrl Pts',(4.55051967938229,-0.986740093628734,
29.6802712986544));
#35413=CARTESIAN_POINT('Ctrl Pts',(3.28914737208629,3.29581475958795,29.8792042370179));
#35414=CARTESIAN_POINT('Ctrl Pts',(-0.995953019991353,4.54851216847773,
30.0781371753813));
#35415=CARTESIAN_POINT('Ctrl Pts',(-4.36546928737203,1.61974172812565,30.2770701137447));
#35416=CARTESIAN_POINT('Ctrl Pts',(-3.72178985561752,-2.79806462317125,
30.4760030521082));
#35417=CARTESIAN_POINT('Ctrl Pts',(0.343347856660311,-4.64359748623272,
30.6749359904716));
#35418=CARTESIAN_POINT('Ctrl Pts',(4.09284432834063,-2.22025013653641,30.8738689288351));
#35419=CARTESIAN_POINT('Ctrl Pts',(4.07977046119387,2.24418322531598,31.0728018671985));
#35420=CARTESIAN_POINT('Ctrl Pts',(0.316145120535775,4.64552877803824,31.2717348055619));
#35421=CARTESIAN_POINT('Ctrl Pts',(-3.73811386212439,2.77621867269378,31.4706677439254));
#35422=CARTESIAN_POINT('Ctrl Pts',(-4.35590783110296,-1.64528183961164,
31.6696006822888));
#35423=CARTESIAN_POINT('Ctrl Pts',(-0.969295991024743,-4.55426730074148,
31.8685336206522));
#35424=CARTESIAN_POINT('Ctrl Pts',(3.30839404621819,-3.27649419345861,32.0674665590156));
#35425=CARTESIAN_POINT('Ctrl Pts',(4.54466244392879,1.01337487415237,32.2663994973791));
#35426=CARTESIAN_POINT('Ctrl Pts',(1.60300206162132,4.3716438275845,32.4653324357425));
#35427=CARTESIAN_POINT('Ctrl Pts',(-2.81230538035333,3.71104079908257,32.664265374106));
#35428=CARTESIAN_POINT('Ctrl Pts',(-4.64224774147941,-0.361138853557849,
32.8631983124694));
#35429=CARTESIAN_POINT('Ctrl Pts',(-2.20455071631624,-4.10132192152844,
33.0621312508329));
#35430=CARTESIAN_POINT('Ctrl Pts',(2.25979977284874,-4.07114116083598,33.2610641891963));
#35431=CARTESIAN_POINT('Ctrl Pts',(4.64670608996618,-0.298341881556976,
33.4599971275598));
#35432=CARTESIAN_POINT('Ctrl Pts',(2.76187444082632,3.74872444145071,33.6589300659231));
#35433=CARTESIAN_POINT('Ctrl Pts',(-1.66196089791414,4.34957139711773,33.8578630042867));
#35434=CARTESIAN_POINT('Ctrl Pts',(-4.55794805159614,0.951837656205623,
34.05679594265));
#35435=CARTESIAN_POINT('Ctrl Pts',(-3.26379290592433,-3.32092475555494,
34.2557288810135));
#35436=CARTESIAN_POINT('Ctrl Pts',(1.03078184888602,-4.54074598990379,34.4546618193769));
#35437=CARTESIAN_POINT('Ctrl Pts',(4.37775417876074,-1.58623885816811,34.6535947577404));
#35438=CARTESIAN_POINT('Ctrl Pts',(3.70023725317449,2.82650484433319,34.8525276961038));
#35439=CARTESIAN_POINT('Ctrl Pts',(-0.378924547838154,4.64082983440129,
35.0514606344673));
#35440=CARTESIAN_POINT('Ctrl Pts',(-4.10973929482816,2.18881892658129,35.2503935728307));
#35441=CARTESIAN_POINT('Ctrl Pts',(-4.06245208373585,-2.27538313964179,
35.4493265111941));
#35442=CARTESIAN_POINT('Ctrl Pts',(-0.280534262010886,-4.64781517410965,
35.6482594495575));
#35443=CARTESIAN_POINT('Ctrl Pts',(3.75927997809232,-2.74748965623102,35.847192387921));
#35444=CARTESIAN_POINT('Ctrl Pts',(4.34317109818868,1.67861555356232,36.0461253262844));
#35445=CARTESIAN_POINT('Ctrl Pts',(0.934365345509009,4.56156187792131,36.2450582646479));
#35446=CARTESIAN_POINT('Ctrl Pts',(-3.33340670360185,3.25104369593922,36.4439912030113));
#35447=CARTESIAN_POINT('Ctrl Pts',(-4.53676286392246,-1.04817368853247,
36.6429241413748));
#35448=CARTESIAN_POINT('Ctrl Pts',(-1.56945236387344,-4.38380025132158,
36.8418570797382));
#35449=CARTESIAN_POINT('Ctrl Pts',(2.84066280656719,-3.68937937625476,37.0407900181016));
#35450=CARTESIAN_POINT('Ctrl Pts',(4.63934378591771,0.396704677840125,37.239722956465));
#35451=CARTESIAN_POINT('Ctrl Pts',(2.17305499813018,4.11809632563053,37.4386558948285));
#35452=CARTESIAN_POINT('Ctrl Pts',(-2.29093309651572,4.05370335558988,37.6375888331919));
#35453=CARTESIAN_POINT('Ctrl Pts',(-4.64885601488985,0.262722526983691,
37.8365217715554));
#35454=CARTESIAN_POINT('Ctrl Pts',(-2.73306452876649,-3.76978032399644,
38.0354547099188));
#35455=CARTESIAN_POINT('Ctrl Pts',(1.69524555941862,-4.33670701499282,38.2343876482823));
#35456=CARTESIAN_POINT('Ctrl Pts',(4.56510873163454,-0.91687934098516,38.4333205866457));
#35457=CARTESIAN_POINT('Ctrl Pts',(3.23824674115109,3.34583975599457,38.6322535250092));
#35458=CARTESIAN_POINT('Ctrl Pts',(-1.0655501194135,4.53271303067627,38.8311864633726));
#35459=CARTESIAN_POINT('Ctrl Pts',(-4.38978199161124,1.55264300508237,39.030119401736));
#35460=CARTESIAN_POINT('Ctrl Pts',(-3.67846726040206,-2.85477940410947,
39.2290523400994));
#35461=CARTESIAN_POINT('Ctrl Pts',(0.414478853343105,-4.63778895635907,
39.4279852784629));
#35462=CARTESIAN_POINT('Ctrl Pts',(4.12639313890974,-2.15726043097348,39.6269182168263));
#35463=CARTESIAN_POINT('Ctrl Pts',(4.04489462987461,2.30645184786356,39.8258511551898));
#35464=CARTESIAN_POINT('Ctrl Pts',(0.244907848885221,4.64982393177198,40.0247840935532));
#35465=CARTESIAN_POINT('Ctrl Pts',(-3.7802270717933,2.71860821686265,40.2237170319166));
#35466=CARTESIAN_POINT('Ctrl Pts',(-4.33017589256357,-1.71186782838445,
40.4226499702801));
#35467=CARTESIAN_POINT('Ctrl Pts',(-0.899386323495868,-4.56855565825224,
40.6215829086435));
#35468=CARTESIAN_POINT('Ctrl Pts',(3.35823604979678,-3.22546532698901,40.820515847007));
#35469=CARTESIAN_POINT('Ctrl Pts',(4.52857292413312,1.08303189027643,41.0194487853703));
#35470=CARTESIAN_POINT('Ctrl Pts',(1.53585633535487,4.39546725361082,41.2183817237339));
#35471=CARTESIAN_POINT('Ctrl Pts',(-2.86894131305717,3.66794615293081,41.4173146620972));
#35472=CARTESIAN_POINT('Ctrl Pts',(-4.63599876985225,-0.433100961544568,
41.6162476004607));
#35473=CARTESIAN_POINT('Ctrl Pts',(-2.14175477389098,-4.13298614778951,
41.8151805388241));
#35474=CARTESIAN_POINT('Ctrl Pts',(2.32254996080195,-4.03922744535998,42.0141134771876));
#35475=CARTESIAN_POINT('Ctrl Pts',(4.65006593675241,-0.219670421692099,
42.2130895813624));
#35476=CARTESIAN_POINT('Ctrl Pts',(3.35325446895125,2.44428797335999,42.3457547060828));
#35477=CARTESIAN_POINT('Ctrl Pts',(2.28389974637321,3.20599595416551,42.4121088513486));
#35478=CARTESIAN_POINT('Ctrl Pts',(0.611508770536539,3.88132595430304,35.));
#35479=CARTESIAN_POINT('Ctrl Pts',(0.118578222943326,3.92028118933608,35.));
#35480=CARTESIAN_POINT('Ctrl Pts',(-0.330793196286837,3.8649362500333,35.));
#35481=CARTESIAN_POINT('Ctrl Pts',(-1.19936559364089,3.59881466306489,35.));
#35482=CARTESIAN_POINT('Ctrl Pts',(-1.62149749117243,3.37535010249507,35.));
#35483=CARTESIAN_POINT('Ctrl Pts',(-2.36867762403761,2.78818662381047,35.));
#35484=CARTESIAN_POINT('Ctrl Pts',(-2.6932378844351,2.41841696079855,35.));
#35485=CARTESIAN_POINT('Ctrl Pts',(-3.15963245702077,1.58300838024013,35.));
#35486=CARTESIAN_POINT('Ctrl Pts',(-3.27506359737994,1.16827729677819,35.));
#35487=CARTESIAN_POINT('Ctrl Pts',(-3.36041119364516,0.460553542036781,
35.));
#35488=CARTESIAN_POINT('Ctrl Pts',(-3.3545966628611,0.135941322369615,35.));
#35489=CARTESIAN_POINT('Ctrl Pts',(-3.25862262511255,-0.476833139036369,
35.));
#35490=CARTESIAN_POINT('Ctrl Pts',(-3.17389841532412,-0.767201663680286,
35.));
#35491=CARTESIAN_POINT('Ctrl Pts',(-3.05035511918376,-1.03985107319943,
35.));
#35492=CARTESIAN_POINT('Ctrl Pts',(3.9282775211904,0.00261363778016546,
35.9708380071379));
#35493=CARTESIAN_POINT('Ctrl Pts',(3.93118033843727,0.487443495032958,35.9952950051125));
#35494=CARTESIAN_POINT('Ctrl Pts',(3.62292672813806,2.28323870400638,36.086062982542));
#35495=CARTESIAN_POINT('Ctrl Pts',(0.933577472432809,4.55771548976854,36.2431419394252));
#35496=CARTESIAN_POINT('Ctrl Pts',(-3.3305959172111,3.24830235946759,36.4420748777888));
#35497=CARTESIAN_POINT('Ctrl Pts',(-4.53293738673136,-1.04728985028724,
36.6410078161523));
#35498=CARTESIAN_POINT('Ctrl Pts',(-1.56812897439943,-4.38010375485825,
36.8399407545156));
#35499=CARTESIAN_POINT('Ctrl Pts',(2.7129575081135,-3.70599985813041,37.0332163973897));
#35500=CARTESIAN_POINT('Ctrl Pts',(3.93099554165428,-1.19260423393931,37.1601810608092));
#35501=CARTESIAN_POINT('Ctrl Pts',(3.93831984400274,0.00193663700642166,
37.2208347447742));
#35502=CARTESIAN_POINT('Ctrl Pts',(3.07780630188836,-0.968536646922482,
38.));
#35503=CARTESIAN_POINT('Ctrl Pts',(2.99903510824282,-1.34635453962162,38.));
#35504=CARTESIAN_POINT('Ctrl Pts',(2.84886247697082,-1.70893883494449,38.));
#35505=CARTESIAN_POINT('Ctrl Pts',(2.40059258209399,-2.42969373277311,38.));
#35506=CARTESIAN_POINT('Ctrl Pts',(2.07741558654446,-2.77581644702267,38.));
#35507=CARTESIAN_POINT('Ctrl Pts',(1.44890409383044,-3.22190503673451,38.));
#35508=CARTESIAN_POINT('Ctrl Pts',(1.05009098077866,-3.45341296726265,38.));
#35509=CARTESIAN_POINT('Ctrl Pts',(0.0196169452910218,-3.68379679183913,
38.));
#35510=CARTESIAN_POINT('Ctrl Pts',(-0.46849028901934,-3.69578977970723,
38.));
#35511=CARTESIAN_POINT('Ctrl Pts',(-1.28710045430295,-3.56665885634214,
38.));
#35512=CARTESIAN_POINT('Ctrl Pts',(-1.62645567600777,-3.46531472498767,
38.));
#35513=CARTESIAN_POINT('Ctrl Pts',(-2.1711767312706,-3.2135327704138,38.));
#35514=CARTESIAN_POINT('Ctrl Pts',(-2.46327288395651,-3.05058587178992,
38.));
#35515=CARTESIAN_POINT('Ctrl Pts',(-2.77271538323007,-2.7876149603501,38.));
#35516=CARTESIAN_POINT('Ctrl Pts',(-1.4752554566251,-2.865264193787,36.4017031386693));
#35517=CARTESIAN_POINT('Ctrl Pts',(-1.66869427635609,-2.76566720899584,
36.3893221826344));
#35518=CARTESIAN_POINT('Ctrl Pts',(-1.85161275111611,-2.64670560438004,
36.3774197811539));
#35519=CARTESIAN_POINT('Ctrl Pts',(-2.09281079697536,-2.45249159555157,
36.3597902555439));
#35520=CARTESIAN_POINT('Ctrl Pts',(-2.16192269046745,-2.39179020980833,
36.3544830894472));
#35521=CARTESIAN_POINT('Ctrl Pts',(-2.26887596446572,-2.28942515554214,
36.3457533615933));
#35522=CARTESIAN_POINT('Ctrl Pts',(-2.30838825200233,-2.24957969103573,
36.3424043407513));
#35523=CARTESIAN_POINT('Ctrl Pts',(-2.35861129851129,-2.19621614818392,
36.3379699373801));
#35524=CARTESIAN_POINT('Ctrl Pts',(-2.37028355000504,-2.183613633822,36.3369262723467));
#35525=CARTESIAN_POINT('Ctrl Pts',(-2.38916441559391,-2.16289822266887,
36.3352162229861));
#35526=CARTESIAN_POINT('Ctrl Pts',(-2.39643388059001,-2.15484105626593,
36.3345524375081));
#35527=CARTESIAN_POINT('Ctrl Pts',(-2.41037868396717,-2.13922738878082,
36.3332685845929));
#35528=CARTESIAN_POINT('Ctrl Pts',(-2.4170595355309,-2.13167596483264,36.3326487603306));
#35529=CARTESIAN_POINT('Ctrl Pts',(-2.43233722136632,-2.11424330367405,
36.3312203273868));
#35530=CARTESIAN_POINT('Ctrl Pts',(-2.44090943012627,-2.10434081159747,
36.330410705713));
#35531=CARTESIAN_POINT('Ctrl Pts',(-2.46366055643201,-2.077732978578,36.3282398591823));
#35532=CARTESIAN_POINT('Ctrl Pts',(-2.47772967263198,-2.06093505444706,
36.3268741521003));
#35533=CARTESIAN_POINT('Ctrl Pts',(-2.59564432521869,-1.91719733185216,
36.3152262642827));
#35534=CARTESIAN_POINT('Ctrl Pts',(-2.68981555077983,-1.78266448109943,
36.3045561258471));
#35535=CARTESIAN_POINT('Ctrl Pts',(-2.90296655650853,-1.42255880187577,
36.2766451192449));
#35536=CARTESIAN_POINT('Ctrl Pts',(-3.00619697526368,-1.1889757742665,36.2590762793693));
#35537=CARTESIAN_POINT('Ctrl Pts',(-3.09723001100283,-0.892406918471076,
36.2387879909886));
#35538=CARTESIAN_POINT('Ctrl Pts',(-3.11220098758202,-0.838707191176308,
36.2351947135659));
#35539=CARTESIAN_POINT('Ctrl Pts',(-3.12860596231211,-0.77335485671857,
36.2309399339579));
#35540=CARTESIAN_POINT('Ctrl Pts',(-3.1313783140909,-0.762051747337994,
36.23020828139));
#35541=CARTESIAN_POINT('Ctrl Pts',(-3.13560336091536,-0.744413435422304,
36.2290734147302));
#35542=CARTESIAN_POINT('Ctrl Pts',(-3.13709819101134,-0.738088572967554,
36.2286678385843));
#35543=CARTESIAN_POINT('Ctrl Pts',(-3.13984177468579,-0.72632112201274,
36.2279158659925));
#35544=CARTESIAN_POINT('Ctrl Pts',(-3.14109550405649,-0.720879863391161,
36.2275691944005));
#35545=CARTESIAN_POINT('Ctrl Pts',(-3.14390848360291,-0.708524692862517,
36.2267843606805));
#35546=CARTESIAN_POINT('Ctrl Pts',(-3.14545906890058,-0.7016088951856,36.2263467005048));
#35547=CARTESIAN_POINT('Ctrl Pts',(-3.15000053601545,-0.681035719783496,
36.2250494938298));
#35548=CARTESIAN_POINT('Ctrl Pts',(-3.15292541978737,-0.667363725563551,
36.2241936408038));
#35549=CARTESIAN_POINT('Ctrl Pts',(-3.17473630572985,-0.562066480390239,
36.217646818863));
#35550=CARTESIAN_POINT('Ctrl Pts',(-3.18971552183379,-0.469667736758124,
36.2121612808798));
#35551=CARTESIAN_POINT('Ctrl Pts',(-3.22881685393737,-0.137475661207952,
36.1929448764684));
#35552=CARTESIAN_POINT('Ctrl Pts',(-3.23006391976129,0.104198470726065,
36.1798418610527));
#35553=CARTESIAN_POINT('Ctrl Pts',(-3.19454133368619,0.435317819656115,
36.160884215462));
#35554=CARTESIAN_POINT('Ctrl Pts',(-3.18080107331359,0.526401492349101,
36.1555698766831));
#35555=CARTESIAN_POINT('Ctrl Pts',(-3.15243249578763,0.671893889730702,
36.1468294285881));
#35556=CARTESIAN_POINT('Ctrl Pts',(-3.14024503129078,0.726727324839323,
36.1434770969363));
#35557=CARTESIAN_POINT('Ctrl Pts',(-3.12246623469435,0.797883107871334,
36.1390389195492));
#35558=CARTESIAN_POINT('Ctrl Pts',(-3.11816761874797,0.814520425915876,
36.1379948815497));
#35559=CARTESIAN_POINT('Ctrl Pts',(-3.11093724354449,0.841608473586556,
36.1362843746005));
#35560=CARTESIAN_POINT('Ctrl Pts',(-3.10808534167546,0.852080313344894,
36.1356205071843));
#35561=CARTESIAN_POINT('Ctrl Pts',(-3.10248225175357,0.872251734680528,
36.1343366035991));
#35562=CARTESIAN_POINT('Ctrl Pts',(-3.09973833263651,0.881953216784308,
36.1337168111851));
#35563=CARTESIAN_POINT('Ctrl Pts',(-3.09332614644484,0.904224736958464,
36.1322886061585));
#35564=CARTESIAN_POINT('Ctrl Pts',(-3.08962672060242,0.916785548758172,
36.1314791816102));
#35565=CARTESIAN_POINT('Ctrl Pts',(-3.07953558225134,0.950293529925363,
36.129309207357));
#35566=CARTESIAN_POINT('Ctrl Pts',(-3.07300680849741,0.971198389648268,
36.1279441810858));
#35567=CARTESIAN_POINT('Ctrl Pts',(-3.0159472071808,1.14756308465134,36.1163308383265));
#35568=CARTESIAN_POINT('Ctrl Pts',(-2.95387687150754,1.29901325345948,36.105697220258));
#35569=CARTESIAN_POINT('Ctrl Pts',(-2.76697646274527,1.67157634412449,36.0778999850928));
#35570=CARTESIAN_POINT('Ctrl Pts',(-2.62704589908076,1.8838659841783,36.0604107198992));
#35571=CARTESIAN_POINT('Ctrl Pts',(-2.4268025361608,2.12132573757848,36.0400797143045));
#35572=CARTESIAN_POINT('Ctrl Pts',(-2.38874354333528,2.16409303804695,36.0363872694324));
#35573=CARTESIAN_POINT('Ctrl Pts',(-2.34153542950344,2.2143773270336,36.0320314379602));
#35574=CARTESIAN_POINT('Ctrl Pts',(-2.33346121713322,2.22288413378063,36.0312940349814));
#35575=CARTESIAN_POINT('Ctrl Pts',(-2.32082720425748,2.23605034476201,36.0301522142088));
#35576=CARTESIAN_POINT('Ctrl Pts',(-2.31629950050604,2.24074020851906,36.029745388234));
#35577=CARTESIAN_POINT('Ctrl Pts',(-2.30786846486906,2.24942034050592,36.0289922854517));
#35578=CARTESIAN_POINT('Ctrl Pts',(-2.30396903297706,2.2534141685973,36.0286457260504));
#35579=CARTESIAN_POINT('Ctrl Pts',(-2.29511360627042,2.26243694868658,36.0278626538892));
#35580=CARTESIAN_POINT('Ctrl Pts',(-2.290151462035,2.26745974510023,36.0274266337121));
#35581=CARTESIAN_POINT('Ctrl Pts',(-2.27540346167664,2.28229020923059,36.0261387796157));
#35582=CARTESIAN_POINT('Ctrl Pts',(-2.26557067601711,2.29205127353722,36.0252905607156));
#35583=CARTESIAN_POINT('Ctrl Pts',(-2.19153366999279,2.3646062912491,36.0189783980574));
#35584=CARTESIAN_POINT('Ctrl Pts',(-2.12478637581597,2.42476159288578,36.0137036131672));
#35585=CARTESIAN_POINT('Ctrl Pts',(-1.86643674046048,2.63872350758135,35.9943970810265));
#35586=CARTESIAN_POINT('Ctrl Pts',(-1.65997040785983,2.77325803802885,35.981053019721));
#35587=CARTESIAN_POINT('Ctrl Pts',(-1.35827624099663,2.92396860341079,35.961850542876));
#35588=CARTESIAN_POINT('Ctrl Pts',(-1.27463637834816,2.96138598143209,35.9565630524638));
#35589=CARTESIAN_POINT('Ctrl Pts',(-1.1375192048237,3.01584123027732,35.9478627399254));
#35590=CARTESIAN_POINT('Ctrl Pts',(-1.08499093539938,3.03513465362525,35.944522811462));
#35591=CARTESIAN_POINT('Ctrl Pts',(-1.0157326370007,3.05854528327568,35.9400987738295));
#35592=CARTESIAN_POINT('Ctrl Pts',(-0.999432527825012,3.06391035187438,
35.9390561348554));
#35593=CARTESIAN_POINT('Ctrl Pts',(-0.972759502201917,3.07245409982136,
35.9373473443108));
#35594=CARTESIAN_POINT('Ctrl Pts',(-0.962411873305188,3.07571107651609,
35.9366837842103));
#35595=CARTESIAN_POINT('Ctrl Pts',(-0.942414204529635,3.08189466328807,
35.9354000702273));
#35596=CARTESIAN_POINT('Ctrl Pts',(-0.932766472689344,3.08482835053112,
35.9347801579221));
#35597=CARTESIAN_POINT('Ctrl Pts',(-0.910548242818551,3.09147072288122,
35.9333510959763));
#35598=CARTESIAN_POINT('Ctrl Pts',(-0.897968636476481,3.09514808251229,
35.9325409304278));
#35599=CARTESIAN_POINT('Ctrl Pts',(-0.864270272341653,3.10477629925755,
35.9303676766413));
#35600=CARTESIAN_POINT('Ctrl Pts',(-0.84311287625281,3.11058830633781,35.9290000905431));
#35601=CARTESIAN_POINT('Ctrl Pts',(-0.661863218807286,3.15839317942911,
35.917255867631));
#35602=CARTESIAN_POINT('Ctrl Pts',(-0.498840065700016,3.18820543149673,
35.9064838119598));
#35603=CARTESIAN_POINT('Ctrl Pts',(-0.0775209154443138,3.23214251743292,
35.8782184628344));
#35604=CARTESIAN_POINT('Ctrl Pts',(0.181502930681532,3.22797267735349,35.8603879234517));
#35605=CARTESIAN_POINT('Ctrl Pts',(0.487863319199088,3.18601893455163,35.8402195684928));
#35606=CARTESIAN_POINT('Ctrl Pts',(0.538307763061424,3.17788494441735,35.8369327137392));
#35607=CARTESIAN_POINT('Ctrl Pts',(0.599688383849988,3.16648384856296,35.8329920686422));
#35608=CARTESIAN_POINT('Ctrl Pts',(0.610825264923671,3.1643543773893,35.8322794622434));
#35609=CARTESIAN_POINT('Ctrl Pts',(0.628263365765897,3.16092456329657,35.8311676523732));
#35610=CARTESIAN_POINT('Ctrl Pts',(0.634572195913244,3.15966407732031,35.8307662369272));
#35611=CARTESIAN_POINT('Ctrl Pts',(0.646357797563831,3.15727262567872,35.8300179358789));
#35612=CARTESIAN_POINT('Ctrl Pts',(0.651835339067373,3.15614630945402,35.8296708001458));
#35613=CARTESIAN_POINT('Ctrl Pts',(0.664341425809498,3.15354080655823,35.8288796893868));
#35614=CARTESIAN_POINT('Ctrl Pts',(0.671367963211146,3.15205238043466,35.8284362492664));
#35615=CARTESIAN_POINT('Ctrl Pts',(0.692987271204733,3.14739720691011,35.8270749245637));
#35616=CARTESIAN_POINT('Ctrl Pts',(0.707563300445875,3.1441524663894,35.8261613932797));
#35617=CARTESIAN_POINT('Ctrl Pts',(0.850396354165353,3.11131309319946,35.8172470247137));
#35618=CARTESIAN_POINT('Ctrl Pts',(0.976765664063272,3.07398449267316,35.8096553219812));
#35619=CARTESIAN_POINT('Ctrl Pts',(1.28116377243312,2.96339000666203,35.7913234671513));
#35620=CARTESIAN_POINT('Ctrl Pts',(1.45558247647445,2.88172568056682,35.780760304734));
#35621=CARTESIAN_POINT('Ctrl Pts',(1.70654800596999,2.73559036088559,35.7642735856097));
#35622=CARTESIAN_POINT('Ctrl Pts',(1.78910043840985,2.68232698899493,35.7586216402397));
#35623=CARTESIAN_POINT('Ctrl Pts',(1.91698293481149,2.59128356765466,35.7493783783071));
#35624=CARTESIAN_POINT('Ctrl Pts',(1.9639329974732,2.55588353055802,35.745872467841));
#35625=CARTESIAN_POINT('Ctrl Pts',(2.02353954300244,2.508328195338,35.7412594877645));
#35626=CARTESIAN_POINT('Ctrl Pts',(2.03710357511151,2.49732489340492,35.7401985238074));
#35627=CARTESIAN_POINT('Ctrl Pts',(2.05899814435663,2.47926669655605,35.7384672422277));
#35628=CARTESIAN_POINT('Ctrl Pts',(2.06738357303326,2.47227867936313,35.7377996490559));
#35629=CARTESIAN_POINT('Ctrl Pts',(2.0834294887869,2.45876805592077,35.7365133556708));
#35630=CARTESIAN_POINT('Ctrl Pts',(2.09109526081211,2.45225190266198,35.7358949252326));
#35631=CARTESIAN_POINT('Ctrl Pts',(2.10856282331383,2.43726245061999,35.7344766745273));
#35632=CARTESIAN_POINT('Ctrl Pts',(2.11834423121709,2.42876576541529,35.7336758885155));
#35633=CARTESIAN_POINT('Ctrl Pts',(2.14416746548818,2.40605957695487,35.7315440229543));
#35634=CARTESIAN_POINT('Ctrl Pts',(2.16011903659429,2.39174884129328,35.7302087106815));
#35635=CARTESIAN_POINT('Ctrl Pts',(2.28178596952608,2.28038701143607,35.7198793175012));
#35636=CARTESIAN_POINT('Ctrl Pts',(2.38104065298987,2.17654485412815,35.7105913832565));
#35637=CARTESIAN_POINT('Ctrl Pts',(2.60610116272965,1.9072020843764,35.6873192778303));
#35638=CARTESIAN_POINT('Ctrl Pts',(2.72346917200883,1.73547943336091,35.6731209344519));
#35639=CARTESIAN_POINT('Ctrl Pts',(2.86327716762166,1.48140730809603,35.6536685706928));
#35640=CARTESIAN_POINT('Ctrl Pts',(2.90026300488421,1.40762216183968,35.6481915085174));
#35641=CARTESIAN_POINT('Ctrl Pts',(2.95217899339544,1.29329433477463,35.6400426875703));
#35642=CARTESIAN_POINT('Ctrl Pts',(2.96919330260592,1.25373944989675,35.6372828773444));
#35643=CARTESIAN_POINT('Ctrl Pts',(2.9894558456152,1.20390474923328,35.6338900495056));
#35644=CARTESIAN_POINT('Ctrl Pts',(2.99345118547411,1.19393588856406,35.6332155142094));
#35645=CARTESIAN_POINT('Ctrl Pts',(2.99971151516166,1.17808662315959,35.6321498891079));
#35646=CARTESIAN_POINT('Ctrl Pts',(3.00200917756625,1.17221933326814,35.6317568749454));
#35647=CARTESIAN_POINT('Ctrl Pts',(3.00632254169706,1.16110890536614,35.6310154895963));
#35648=CARTESIAN_POINT('Ctrl Pts',(3.00834171820475,1.15586730284646,35.6306669200337));
#35649=CARTESIAN_POINT('Ctrl Pts',(3.01294585228916,1.14382158984963,35.6298685788811));
#35650=CARTESIAN_POINT('Ctrl Pts',(3.01552146961116,1.13701398715773,35.629419370794));
#35651=CARTESIAN_POINT('Ctrl Pts',(3.02233856552016,1.11880964888251,35.6282232474624));
#35652=CARTESIAN_POINT('Ctrl Pts',(3.02653868850251,1.10739740513477,35.6274787377006));
#35653=CARTESIAN_POINT('Ctrl Pts',(3.0568196732153,1.0236610669434,35.6220530591413));
#35654=CARTESIAN_POINT('Ctrl Pts',(3.08037192600609,0.95044167935542,35.6175107525742));
#35655=CARTESIAN_POINT('Ctrl Pts',(3.11097997869764,0.842135496686508,35.6109890728551));
#35656=CARTESIAN_POINT('Ctrl Pts',(3.12010599606352,0.807667834496542,35.6089422944302));
#35657=CARTESIAN_POINT('Ctrl Pts',(3.19099536871426,0.520768915049164,35.5920907939819));
#35658=CARTESIAN_POINT('Ctrl Pts',(3.22258956834844,0.26187146746877,35.5779830578411));
#35659=CARTESIAN_POINT('Ctrl Pts',(3.22277045874783,-0.0322773699741125,
35.5610272103996));
#35660=CARTESIAN_POINT('Ctrl Pts',(3.22224523984713,-0.066533945178146,
35.5590399266099));
#35661=CARTESIAN_POINT('Ctrl Pts',(3.21890748730524,-0.173222058847471,
35.5528027301262));
#35662=CARTESIAN_POINT('Ctrl Pts',(3.21419767276895,-0.245567538508346,
35.5485036776561));
#35663=CARTESIAN_POINT('Ctrl Pts',(3.20514311002084,-0.33697288876932,35.5429577596319));
#35664=CARTESIAN_POINT('Ctrl Pts',(3.20305899040129,-0.356238911551028,
35.541782396898));
#35665=CARTESIAN_POINT('Ctrl Pts',(3.19946716450695,-0.386857263082903,
35.5399037846077));
#35666=CARTESIAN_POINT('Ctrl Pts',(3.1980724597936,-0.398222570088934,35.5392041122974));
#35667=CARTESIAN_POINT('Ctrl Pts',(3.19535127629391,-0.419460375111782,
35.537892182604));
#35668=CARTESIAN_POINT('Ctrl Pts',(3.19403953329945,-0.429334649629104,
35.5372803993823));
#35669=CARTESIAN_POINT('Ctrl Pts',(3.19101107114512,-0.451349357235508,
35.5359123039807));
#35670=CARTESIAN_POINT('Ctrl Pts',(3.18927080993015,-0.463486345758742,
35.5351552527041));
#35671=CARTESIAN_POINT('Ctrl Pts',(3.18396657084568,-0.499034276468238,
35.5329295583531));
#35672=CARTESIAN_POINT('Ctrl Pts',(3.18021382781233,-0.52241582519382,35.5314549444777));
#35673=CARTESIAN_POINT('Ctrl Pts',(3.14448045485697,-0.730378754707215,
35.5182414144364));
#35674=CARTESIAN_POINT('Ctrl Pts',(3.09672586591152,-0.911854036969413,
35.505990195684));
#35675=CARTESIAN_POINT('Ctrl Pts',(2.9656460481618,-1.27727914256669,35.4799597309547));
#35676=CARTESIAN_POINT('Ctrl Pts',(2.88025696302375,-1.45966344587103,35.466189726902));
#35677=CARTESIAN_POINT('Ctrl Pts',(2.73622269328183,-1.70474207114958,35.4473403881831));
#35678=CARTESIAN_POINT('Ctrl Pts',(2.69123067814493,-1.77491978094744,35.4419040066358));
#35679=CARTESIAN_POINT('Ctrl Pts',(2.63578119894601,-1.85444337392499,35.4357656432674));
#35680=CARTESIAN_POINT('Ctrl Pts',(2.62792686323624,-1.86555706765961,35.4349083201578));
#35681=CARTESIAN_POINT('Ctrl Pts',(2.61592162305662,-1.88231791459035,35.4336165957597));
#35682=CARTESIAN_POINT('Ctrl Pts',(2.6118224261631,-1.88800166471346,35.4331787764034));
#35683=CARTESIAN_POINT('Ctrl Pts',(2.6044269530751,-1.89818569295259,35.4323947565128));
#35684=CARTESIAN_POINT('Ctrl Pts',(2.60113751873638,-1.90269080224331,35.4320480952229));
#35685=CARTESIAN_POINT('Ctrl Pts',(2.59395485720042,-1.91247451749451,35.4312956204062));
#35686=CARTESIAN_POINT('Ctrl Pts',(2.5900572199996,-1.91774976996398,35.4308901207858));
#35687=CARTESIAN_POINT('Ctrl Pts',(2.579034956004,-1.93257294270851,35.4297512096261));
#35688=CARTESIAN_POINT('Ctrl Pts',(2.57187336579427,-1.94209342818767,35.4290203320154));
#35689=CARTESIAN_POINT('Ctrl Pts',(2.52804589648987,-1.99968924852045,35.4246010107285));
#35690=CARTESIAN_POINT('Ctrl Pts',(2.49008323391232,-2.04676811675291,35.4209981831955));
#35691=CARTESIAN_POINT('Ctrl Pts',(2.28489354975244,-2.28706488110814,35.40249454867));
#35692=CARTESIAN_POINT('Ctrl Pts',(2.09643850884567,-2.46097052873984,35.3886395806164));
#35693=CARTESIAN_POINT('Ctrl Pts',(1.76143196867848,-2.70341046135735,35.3652458027176));
#35694=CARTESIAN_POINT('Ctrl Pts',(1.62684207387483,-2.78647554838319,35.356126270503));
#35695=CARTESIAN_POINT('Ctrl Pts',(1.467387265963,-2.86938439405468,35.3453154817556));
#35696=CARTESIAN_POINT('Ctrl Pts',(1.44795700712991,-2.87923820809416,35.3439983244115));
#35697=CARTESIAN_POINT('Ctrl Pts',(1.41672087715647,-2.89468307490204,35.3418804623409));
#35698=CARTESIAN_POINT('Ctrl Pts',(1.40497811468858,-2.90040077183462,35.3410841959532));
#35699=CARTESIAN_POINT('Ctrl Pts',(1.38411443619748,-2.91040312218429,35.339669150958));
#35700=CARTESIAN_POINT('Ctrl Pts',(1.37500751912376,-2.91471669717657,35.3390513897142));
#35701=CARTESIAN_POINT('Ctrl Pts',(1.3560369876221,-2.92359357021239,35.3377642617047));
#35702=CARTESIAN_POINT('Ctrl Pts',(1.34617023405761,-2.92814982060188,35.3370946603137));
#35703=CARTESIAN_POINT('Ctrl Pts',(1.32058308736153,-2.93980874357326,35.3353577093626));
#35704=CARTESIAN_POINT('Ctrl Pts',(1.30482853168874,-2.94683518773189,35.3342877496162));
#35705=CARTESIAN_POINT('Ctrl Pts',(1.23698173352815,-2.9764437312877,35.3296773755474));
#35706=CARTESIAN_POINT('Ctrl Pts',(1.18435676770846,-2.99777241964207,35.3260945593449));
#35707=CARTESIAN_POINT('Ctrl Pts',(1.04366031753545,-3.05051313782734,35.3164915764213));
#35708=CARTESIAN_POINT('Ctrl Pts',(0.954743117662606,-3.07949999194473,
35.3103969897814));
#35709=CARTESIAN_POINT('Ctrl Pts',(0.656845778650454,-3.16247139270354,
35.2899247795844));
#35710=CARTESIAN_POINT('Ctrl Pts',(0.443710345811826,-3.199340739048,35.2751505480742));
#35711=CARTESIAN_POINT('Ctrl Pts',(0.113232386153195,-3.22283315364041,
35.2529448366808));
#35712=CARTESIAN_POINT('Ctrl Pts',(-0.00242276030634944,-3.22482174519131,
35.2453152469946));
#35713=CARTESIAN_POINT('Ctrl Pts',(-0.132683918455096,-3.2200512461733,
35.2370526009332));
#35714=CARTESIAN_POINT('Ctrl Pts',(-0.147417957322412,-3.21941035215556,
35.2361228164553));
#35715=CARTESIAN_POINT('Ctrl Pts',(-0.169284399981222,-3.21830878263779,
35.2347506128558));
#35716=CARTESIAN_POINT('Ctrl Pts',(-0.176420262156259,-3.21792549974631,
35.2343040230992));
#35717=CARTESIAN_POINT('Ctrl Pts',(-0.189134577961852,-3.21720016603975,
35.2335105456669));
#35718=CARTESIAN_POINT('Ctrl Pts',(-0.194713460213433,-3.21686733749034,
35.2331631481637));
#35719=CARTESIAN_POINT('Ctrl Pts',(-0.206736929684483,-3.21611864022215,
35.2324161189759));
#35720=CARTESIAN_POINT('Ctrl Pts',(-0.213181122619191,-3.2156979144143,
35.2320167632884));
#35721=CARTESIAN_POINT('Ctrl Pts',(-0.23104695915257,-3.21447755572762,
35.2309123357424));
#35722=CARTESIAN_POINT('Ctrl Pts',(-0.242465805131233,-3.21363641318313,
35.2302095577113));
#35723=CARTESIAN_POINT('Ctrl Pts',(-0.30647150506476,-3.20857848651103,
35.2262865344371));
#35724=CARTESIAN_POINT('Ctrl Pts',(-0.358956472586155,-3.20313154328421,
35.2231311068008));
#35725=CARTESIAN_POINT('Ctrl Pts',(-0.665949292365562,-3.16363011399075,
35.2049125407654));
#35726=CARTESIAN_POINT('Ctrl Pts',(-0.915807722760667,-3.10054341059219,
35.1909852445635));
#35727=CARTESIAN_POINT('Ctrl Pts',(-1.2646773558253,-2.96654253713258,35.1698817324028));
#35728=CARTESIAN_POINT('Ctrl Pts',(-1.37140074843424,-2.91873648247267,
35.1631909462925));
#35729=CARTESIAN_POINT('Ctrl Pts',(-1.4752555264658,-2.86526415782771,35.1563175586878));
#35730=CARTESIAN_POINT('Origin',(0.,0.,4.68922655072688));
#35731=CARTESIAN_POINT('',(3.22274857165764,-0.00244669484556194,35.3125278845694));
#35732=CARTESIAN_POINT('Ctrl Pts',(3.22274907127793,-0.00244664611808667,
35.3125270209625));
#35733=CARTESIAN_POINT('Ctrl Pts',(3.222822198994,0.0938779826516697,35.3180030298239));
#35734=CARTESIAN_POINT('Ctrl Pts',(3.2185767818221,0.190152796939803,35.3235561489518));
#35735=CARTESIAN_POINT('Ctrl Pts',(3.20588205807585,0.332591966317148,35.3319873302714));
#35736=CARTESIAN_POINT('Ctrl Pts',(3.20072779093437,0.378996656346596,35.3347679097327));
#35737=CARTESIAN_POINT('Ctrl Pts',(3.19245693920111,0.441125918843006,35.3385432245935));
#35738=CARTESIAN_POINT('Ctrl Pts',(3.19022835540884,0.456964343398726,35.3395102459607));
#35739=CARTESIAN_POINT('Ctrl Pts',(3.18626032428469,0.483719859681448,35.3411518760625));
#35740=CARTESIAN_POINT('Ctrl Pts',(3.18458242116393,0.494645888305743,35.3418245401713));
#35741=CARTESIAN_POINT('Ctrl Pts',(3.18138073222578,0.514802606888697,35.343069798848));
#35742=CARTESIAN_POINT('Ctrl Pts',(3.17987289518586,0.524035738267946,35.3436418822315));
#35743=CARTESIAN_POINT('Ctrl Pts',(3.17667380192803,0.543102830753287,35.3448267903223));
#35744=CARTESIAN_POINT('Ctrl Pts',(3.17497703570969,0.552935753749137,35.3454397847159));
#35745=CARTESIAN_POINT('Ctrl Pts',(3.17104917621089,0.575083752271063,35.3468249504617));
#35746=CARTESIAN_POINT('Ctrl Pts',(3.16879196380773,0.587393976037243,35.347597947873));
#35747=CARTESIAN_POINT('Ctrl Pts',(3.16283206722838,0.61886319151895,35.3495820765352));
#35748=CARTESIAN_POINT('Ctrl Pts',(3.15902701529105,0.63800205714112,35.3507964632919));
#35749=CARTESIAN_POINT('Ctrl Pts',(3.13493297705785,0.753688096794359,35.3581845259994));
#35750=CARTESIAN_POINT('Ctrl Pts',(3.11039519341025,0.849287276382102,35.3644936335693));
#35751=CARTESIAN_POINT('Ctrl Pts',(3.06261102411507,1.00533551957057,35.3751383797574));
#35752=CARTESIAN_POINT('Ctrl Pts',(3.0418578526508,1.06648292520211,35.379399773773));
#35753=CARTESIAN_POINT('Ctrl Pts',(2.94398912463826,1.32868619866432,35.3980416007017));
#35754=CARTESIAN_POINT('Ctrl Pts',(2.84867416605034,1.52234281914099,35.4128122584179));
#35755=CARTESIAN_POINT('Ctrl Pts',(2.68796576556024,1.78010743066332,35.4330477547681));
#35756=CARTESIAN_POINT('Ctrl Pts',(2.63809033463233,1.85322009616731,35.4388531537061));
#35757=CARTESIAN_POINT('Ctrl Pts',(2.5738869008461,1.93948110285755,35.4457007292539));
#35758=CARTESIAN_POINT('Ctrl Pts',(2.5623729990046,1.9546675885902,35.4469061530209));
#35759=CARTESIAN_POINT('Ctrl Pts',(2.54587837315102,1.97602726308972,35.4486003580822));
#35760=CARTESIAN_POINT('Ctrl Pts',(2.54100879890514,1.98228522730869,35.449096577208));
#35761=CARTESIAN_POINT('Ctrl Pts',(2.53260068933571,1.99300872320809,35.4499465348641));
#35762=CARTESIAN_POINT('Ctrl Pts',(2.5290733341092,1.99748293987475,35.4503010600482));
#35763=CARTESIAN_POINT('Ctrl Pts',(2.52222693279569,2.00611993793479,35.4509851924609));
#35764=CARTESIAN_POINT('Ctrl Pts',(2.51890943473924,2.01028385221078,35.4513149097283));
#35765=CARTESIAN_POINT('Ctrl Pts',(2.50996017443316,2.02145946404088,35.4521996216935));
#35766=CARTESIAN_POINT('Ctrl Pts',(2.50430930530922,2.02845590286812,35.4527532546306));
#35767=CARTESIAN_POINT('Ctrl Pts',(2.4833899848165,2.05413581198401,35.454784834301));
#35768=CARTESIAN_POINT('Ctrl Pts',(2.46794069348604,2.07267184186707,35.4562502916358));
#35769=CARTESIAN_POINT('Ctrl Pts',(2.32053141693219,2.24554782791318,35.469927795437));
#35770=CARTESIAN_POINT('Ctrl Pts',(2.17445047837928,2.38728703534737,35.4812353044151));
#35771=CARTESIAN_POINT('Ctrl Pts',(1.88435771502452,2.61988086240072,35.5020094141611));
#35772=CARTESIAN_POINT('Ctrl Pts',(1.74465664835936,2.71491207884529,35.5114319292465));
#35773=CARTESIAN_POINT('Ctrl Pts',(1.5464281871252,2.82811377439754,35.5246682146053));
#35774=CARTESIAN_POINT('Ctrl Pts',(1.4938808924124,2.85621898990891,35.5281632300493));
#35775=CARTESIAN_POINT('Ctrl Pts',(1.41606868102879,2.89510246998893,35.5333379420563));
#35776=CARTESIAN_POINT('Ctrl Pts',(1.3913956644315,2.90704091091488,35.5349786056314));
#35777=CARTESIAN_POINT('Ctrl Pts',(1.34675667191248,2.92794174274711,35.5379484416452));
#35778=CARTESIAN_POINT('Ctrl Pts',(1.32684582374589,2.93701830193329,35.5392736405939));
#35779=CARTESIAN_POINT('Ctrl Pts',(1.29603469935726,2.95068660944577,35.541325790494));
#35780=CARTESIAN_POINT('Ctrl Pts',(1.28519874229726,2.9554224056854,35.5420477859514));
#35781=CARTESIAN_POINT('Ctrl Pts',(1.26608673208441,2.96365022108519,35.5433217974865));
#35782=CARTESIAN_POINT('Ctrl Pts',(1.25782164012358,2.96716749866542,35.5438729422159));
#35783=CARTESIAN_POINT('Ctrl Pts',(1.23917063255296,2.97501265594226,35.5451171384687));
#35784=CARTESIAN_POINT('Ctrl Pts',(1.22877657943962,2.97932077364512,35.5458108548017));
#35785=CARTESIAN_POINT('Ctrl Pts',(1.20077530730874,2.9907552592962,35.5476807175804));
#35786=CARTESIAN_POINT('Ctrl Pts',(1.18312750074961,2.99778045421981,35.5488602712433));
#35787=CARTESIAN_POINT('Ctrl Pts',(1.10360230784894,3.02862604087624,35.5541811551656));
#35788=CARTESIAN_POINT('Ctrl Pts',(1.0410645080087,3.05068801941584,35.5583808882861));
#35789=CARTESIAN_POINT('Ctrl Pts',(0.670324953753376,3.16874962926328,35.5833851699237));
#35790=CARTESIAN_POINT('Ctrl Pts',(0.349804969398493,3.21991791190272,35.6056886694998));
#35791=CARTESIAN_POINT('Ctrl Pts',(-0.0350210707554559,3.22315930273634,
35.6312791652481));
#35792=CARTESIAN_POINT('Ctrl Pts',(-0.0971925808733141,3.22188406580124,
35.6353675708624));
#35793=CARTESIAN_POINT('Ctrl Pts',(-0.182893561452371,3.21764291224097,
35.6409071917649));
#35794=CARTESIAN_POINT('Ctrl Pts',(-0.206482432798357,3.21621532886052,
35.6424218546974));
#35795=CARTESIAN_POINT('Ctrl Pts',(-0.247231118304599,3.21329906704435,
35.6450184917643));
#35796=CARTESIAN_POINT('Ctrl Pts',(-0.264398353381229,3.21193207610899,
35.646106333131));
#35797=CARTESIAN_POINT('Ctrl Pts',(-0.289135386438601,3.20976264022414,
35.6476642406725));
#35798=CARTESIAN_POINT('Ctrl Pts',(-0.296714242463301,3.20907091529585,
35.6481402449312));
#35799=CARTESIAN_POINT('Ctrl Pts',(-0.309910016238329,3.20781938479212,
35.6489666766877));
#35800=CARTESIAN_POINT('Ctrl Pts',(-0.31552801204594,3.2072716597146,35.6493177779765));
#35801=CARTESIAN_POINT('Ctrl Pts',(-0.327307768498945,3.20609194379902,
35.6500523711005));
#35802=CARTESIAN_POINT('Ctrl Pts',(-0.333469149909224,3.20545694948554,
35.6504356918027));
#35803=CARTESIAN_POINT('Ctrl Pts',(-0.349836035200082,3.20372247086048,
35.6514516121746));
#35804=CARTESIAN_POINT('Ctrl Pts',(-0.360038282121318,3.20259197586956,
35.6520824847972));
#35805=CARTESIAN_POINT('Ctrl Pts',(-0.40367289845304,3.19754574518788,35.6547711014066));
#35806=CARTESIAN_POINT('Ctrl Pts',(-0.437049586291402,3.19315493961492,
35.6568035218393));
#35807=CARTESIAN_POINT('Ctrl Pts',(-0.476615547774752,3.18731787825588,
35.6591906079939));
#35808=CARTESIAN_POINT('Ctrl Pts',(-0.482875551191465,3.1863755021517,35.6595676223802));
#35809=CARTESIAN_POINT('Ctrl Pts',(-0.78807014476277,3.13951168803674,35.6779176620613));
#35810=CARTESIAN_POINT('Ctrl Pts',(-1.07909311969837,3.05175323564138,35.6941078273691));
#35811=CARTESIAN_POINT('Ctrl Pts',(-1.43660826328232,2.88628354462794,35.7165410559189));
#35812=CARTESIAN_POINT('Ctrl Pts',(-1.51789998880267,2.84437228964257,35.7218192810321));
#35813=CARTESIAN_POINT('Ctrl Pts',(-1.64582570326363,2.77137102702872,35.7305055138283));
#35814=CARTESIAN_POINT('Ctrl Pts',(-1.69362443773071,2.74242143171488,35.7338409247734));
#35815=CARTESIAN_POINT('Ctrl Pts',(-1.7550761634918,2.70298340343429,35.7382595874149));
#35816=CARTESIAN_POINT('Ctrl Pts',(-1.76943349387717,2.69360663645655,35.7393014896748));
#35817=CARTESIAN_POINT('Ctrl Pts',(-1.79274581969509,2.67811455287119,35.7410092249677));
#35818=CARTESIAN_POINT('Ctrl Pts',(-1.80174611087036,2.67206775358597,35.7416724710425));
#35819=CARTESIAN_POINT('Ctrl Pts',(-1.81905491081398,2.66031171451251,35.7429556837871));
#35820=CARTESIAN_POINT('Ctrl Pts',(-1.82736749378812,2.65460867660189,35.7435754096296));
#35821=CARTESIAN_POINT('Ctrl Pts',(-1.8464241598826,2.64140249025563,35.745004193069));
#35822=CARTESIAN_POINT('Ctrl Pts',(-1.85714945377346,2.63387266053652,35.7458142669076));
#35823=CARTESIAN_POINT('Ctrl Pts',(-1.88571089358673,2.6135595504263,35.7479876068367));
#35824=CARTESIAN_POINT('Ctrl Pts',(-1.90346265497794,2.60065933571649,35.7493553731951));
#35825=CARTESIAN_POINT('Ctrl Pts',(-2.05259145839286,2.48994252587534,35.7609923150584));
#35826=CARTESIAN_POINT('Ctrl Pts',(-2.17644666712245,2.38243797731905,35.7716483608506));
#35827=CARTESIAN_POINT('Ctrl Pts',(-2.47009394478667,2.0854759631843,35.7995028679659));
#35828=CARTESIAN_POINT('Ctrl Pts',(-2.62663991601537,1.8844978151653,35.8170272932151));
#35829=CARTESIAN_POINT('Ctrl Pts',(-2.78717237984905,1.61894177903155,35.8373288032252));
#35830=CARTESIAN_POINT('Ctrl Pts',(-2.81509616944046,1.56988433892823,35.8409682944937));
#35831=CARTESIAN_POINT('Ctrl Pts',(-2.84722706337797,1.50981852463014,35.8452700206613));
#35832=CARTESIAN_POINT('Ctrl Pts',(-2.8526792567236,1.49949157912259,35.8460041995074));
#35833=CARTESIAN_POINT('Ctrl Pts',(-2.86108165915521,1.48336496995739,35.8471420350367));
#35834=CARTESIAN_POINT('Ctrl Pts',(-2.86407057471238,1.47758574685005,35.8475480744458));
#35835=CARTESIAN_POINT('Ctrl Pts',(-2.86959073405829,1.46683254934182,35.8483003279048));
#35836=CARTESIAN_POINT('Ctrl Pts',(-2.87212653543665,1.46186109940702,35.8486468205337));
#35837=CARTESIAN_POINT('Ctrl Pts',(-2.87784626086216,1.45057521985763,35.8494305058163));
#35838=CARTESIAN_POINT('Ctrl Pts',(-2.88102231595407,1.44425689780227,35.8498672014981));
#35839=CARTESIAN_POINT('Ctrl Pts',(-2.89038546486611,1.42547641484685,35.8511593211402));
#35840=CARTESIAN_POINT('Ctrl Pts',(-2.89651277506788,1.41298439653568,35.8520110931471));
#35841=CARTESIAN_POINT('Ctrl Pts',(-2.94236488448253,1.31795195014025,35.8584356891103));
#35842=CARTESIAN_POINT('Ctrl Pts',(-2.97863920195295,1.23378293082401,35.8638116284189));
#35843=CARTESIAN_POINT('Ctrl Pts',(-3.09796907748042,0.920820293972021,
35.8830722180209));
#35844=CARTESIAN_POINT('Ctrl Pts',(-3.15863409748303,0.684372923629414,
35.896298481329));
#35845=CARTESIAN_POINT('Ctrl Pts',(-3.20474754755038,0.352348715279247,
35.9153828810517));
#35846=CARTESIAN_POINT('Ctrl Pts',(-3.21348774603249,0.260865942913228,
35.9206853786294));
#35847=CARTESIAN_POINT('Ctrl Pts',(-3.22125103730935,0.113149652394659,
35.9294079034964));
#35848=CARTESIAN_POINT('Ctrl Pts',(-3.22273185991701,0.0570952960618219,
35.9327545369201));
#35849=CARTESIAN_POINT('Ctrl Pts',(-3.22275533909513,-0.0161359277741507,
35.9371859942254));
#35850=CARTESIAN_POINT('Ctrl Pts',(-3.22262364041845,-0.0333046288324061,
35.9382291637872));
#35851=CARTESIAN_POINT('Ctrl Pts',(-3.22218487970022,-0.0613174874208513,
35.9399384538424));
#35852=CARTESIAN_POINT('Ctrl Pts',(-3.22196023686762,-0.0721627377965504,
35.9406019782694));
#35853=CARTESIAN_POINT('Ctrl Pts',(-3.22142124196038,-0.0930824086395146,
35.9418853624112));
#35854=CARTESIAN_POINT('Ctrl Pts',(-3.2211143726453,-0.10315690769907,35.9425049793255));
#35855=CARTESIAN_POINT('Ctrl Pts',(-3.22030020351147,-0.126315525354007,
35.9439329850104));
#35856=CARTESIAN_POINT('Ctrl Pts',(-3.21976041510896,-0.139398256247839,
35.9447423864189));
#35857=CARTESIAN_POINT('Ctrl Pts',(-3.21810443471131,-0.174359777866476,
35.9469127498439));
#35858=CARTESIAN_POINT('Ctrl Pts',(-3.21684487112074,-0.196230786862113,
35.948278192795));
#35859=CARTESIAN_POINT('Ctrl Pts',(-3.20426121056356,-0.381757946721685,
35.9599284392866));
#35860=CARTESIAN_POINT('Ctrl Pts',(-3.18068132286312,-0.544316657537262,
35.9706014164879));
#35861=CARTESIAN_POINT('Ctrl Pts',(-3.0892667155855,-0.952469482132061,
35.998499587124));
#35862=CARTESIAN_POINT('Ctrl Pts',(-3.00453278854938,-1.19312402986472,
36.0160512963132));
#35863=CARTESIAN_POINT('Ctrl Pts',(-2.86773749741407,-1.47150484730143,
36.0363383813135));
#35864=CARTESIAN_POINT('Ctrl Pts',(-2.84177029808648,-1.52104810623624,
36.0399440790494));
#35865=CARTESIAN_POINT('Ctrl Pts',(-2.80885164644733,-1.58006507235858,
36.0442113504063));
#35866=CARTESIAN_POINT('Ctrl Pts',(-2.8031230808684,-1.59020571245238,36.0449435571804));
#35867=CARTESIAN_POINT('Ctrl Pts',(-2.79411210041919,-1.60595684151635,
36.0460790076063));
#35868=CARTESIAN_POINT('Ctrl Pts',(-2.7908675420878,-1.61158871019074,36.0464846181944));
#35869=CARTESIAN_POINT('Ctrl Pts',(-2.78480502505577,-1.62203874467475,
36.0472364846307));
#35870=CARTESIAN_POINT('Ctrl Pts',(-2.78199161484652,-1.62685935852861,
36.0475830165017));
#35871=CARTESIAN_POINT('Ctrl Pts',(-2.77558059952186,-1.63777899505023,
36.0483673095912));
#35872=CARTESIAN_POINT('Ctrl Pts',(-2.77197541752484,-1.64387347079022,
36.0488045706096));
#35873=CARTESIAN_POINT('Ctrl Pts',(-2.76120457265491,-1.66194514565416,
36.0500999161951));
#35874=CARTESIAN_POINT('Ctrl Pts',(-2.75398105038895,-1.67388791430352,
36.050954321706));
#35875=CARTESIAN_POINT('Ctrl Pts',(-2.69807807434776,-1.76497171935793,
36.0574610713057));
#35876=CARTESIAN_POINT('Ctrl Pts',(-2.64606923707545,-1.84202919295389,
36.0629107944885));
#35877=CARTESIAN_POINT('Ctrl Pts',(-2.44705131726415,-2.11103574983077,
36.0821409989197));
#35878=CARTESIAN_POINT('Ctrl Pts',(-2.28190073615814,-2.28855277342994,
36.0952837718125));
#35879=CARTESIAN_POINT('Ctrl Pts',(-2.02860552848562,-2.50586217024917,
36.1142829562129));
#35880=CARTESIAN_POINT('Ctrl Pts',(-1.95623474136634,-2.56275814472599,
36.119594215877));
#35881=CARTESIAN_POINT('Ctrl Pts',(-1.83595694390226,-2.6492510166241,36.1283298372918));
#35882=CARTESIAN_POINT('Ctrl Pts',(-1.78953488430647,-2.68082695623838,
36.1316805162257));
#35883=CARTESIAN_POINT('Ctrl Pts',(-1.72786376367948,-2.72045941322018,
36.1361165850886));
#35884=CARTESIAN_POINT('Ctrl Pts',(-1.71333981160578,-2.7296298791251,36.1371602105065));
#35885=CARTESIAN_POINT('Ctrl Pts',(-1.68952376613095,-2.74440243281156,
36.1388700598438));
#35886=CARTESIAN_POINT('Ctrl Pts',(-1.68027534400173,-2.75007455050425,
36.1395336844176));
#35887=CARTESIAN_POINT('Ctrl Pts',(-1.66238055990656,-2.7609255721317,36.140817130465));
#35888=CARTESIAN_POINT('Ctrl Pts',(-1.65373818681447,-2.76611083411253,
36.1414367084293));
#35889=CARTESIAN_POINT('Ctrl Pts',(-1.63381552198751,-2.77793731968781,
36.1428644354347));
#35890=CARTESIAN_POINT('Ctrl Pts',(-1.62251886347597,-2.784550491828,36.1436735958224));
#35891=CARTESIAN_POINT('Ctrl Pts',(-1.59222088829513,-2.80204024783262,
36.145842892712));
#35892=CARTESIAN_POINT('Ctrl Pts',(-1.57314875726316,-2.81279218160706,
36.1472075032309));
#35893=CARTESIAN_POINT('Ctrl Pts',(-1.52791931900792,-2.83768642883583,
36.1504420200467));
#35894=CARTESIAN_POINT('Ctrl Pts',(-1.50167885936097,-2.85165942216976,
36.1523172954271));
#35895=CARTESIAN_POINT('Ctrl Pts',(-1.47525533429856,-2.86526425676998,
36.1542047394732));
#35896=CARTESIAN_POINT('',(-0.0206799398372109,-3.22268774565723,34.9999898625471));
#35897=CARTESIAN_POINT('Ctrl Pts',(-0.0206996961560602,-3.22268352232717,
34.9999891441435));
#35898=CARTESIAN_POINT('Ctrl Pts',(0.119331606346545,-3.22358296075917,
35.0094451984274));
#35899=CARTESIAN_POINT('Ctrl Pts',(0.25936552548738,-3.21535540382481,35.0189818957179));
#35900=CARTESIAN_POINT('Ctrl Pts',(0.418350219005723,-3.19554380295184,
35.0296712679666));
#35901=CARTESIAN_POINT('Ctrl Pts',(0.438162186753174,-3.19288756849992,
35.0310006946464));
#35902=CARTESIAN_POINT('Ctrl Pts',(0.538410711821889,-3.17849635255725,
35.0377104753343));
#35903=CARTESIAN_POINT('Ctrl Pts',(0.618415001021133,-3.16390431477802,
35.0430099104089));
#35904=CARTESIAN_POINT('Ctrl Pts',(0.710989412689877,-3.14337310041445,
35.0490132261124));
#35905=CARTESIAN_POINT('Ctrl Pts',(0.724171874476634,-3.14036232060865,
35.0498649965779));
#35906=CARTESIAN_POINT('Ctrl Pts',(0.744137358248051,-3.1356699409744,35.0511499399372));
#35907=CARTESIAN_POINT('Ctrl Pts',(0.750934309816619,-3.13404914626411,
35.0515864797157));
#35908=CARTESIAN_POINT('Ctrl Pts',(0.763144882370624,-3.13109542068199,
35.0523690271339));
#35909=CARTESIAN_POINT('Ctrl Pts',(0.768560335508649,-3.12977054383343,
35.0527154888963));
#35910=CARTESIAN_POINT('Ctrl Pts',(0.780350562240213,-3.12685364745952,
35.0534684685532));
#35911=CARTESIAN_POINT('Ctrl Pts',(0.786723894018734,-3.12525618934163,
35.0538746676402));
#35912=CARTESIAN_POINT('Ctrl Pts',(0.80469689099108,-3.12069284333201,35.0550179272153));
#35913=CARTESIAN_POINT('Ctrl Pts',(0.816285121816515,-3.11768175398948,
35.0557524216429));
#35914=CARTESIAN_POINT('Ctrl Pts',(0.887394488285968,-3.09878101651963,
35.060244858625));
#35915=CARTESIAN_POINT('Ctrl Pts',(0.946471035216613,-3.0812508002563,35.063913850737));
#35916=CARTESIAN_POINT('Ctrl Pts',(1.25864133498492,-2.97879114230051,35.0831396542036));
#35917=CARTESIAN_POINT('Ctrl Pts',(1.50096483369849,-2.86435117756486,35.0975670168958));
#35918=CARTESIAN_POINT('Ctrl Pts',(1.84950045737443,-2.64323899408243,35.120997180681));
#35919=CARTESIAN_POINT('Ctrl Pts',(1.96713019752114,-2.55690344213947,35.1294438775362));
#35920=CARTESIAN_POINT('Ctrl Pts',(2.09496623624399,-2.44901979951021,35.1395081131937));
#35921=CARTESIAN_POINT('Ctrl Pts',(2.11128724137151,-2.43496358479719,35.1408105703398));
#35922=CARTESIAN_POINT('Ctrl Pts',(2.13722039559061,-2.41217229639306,35.1429091243416));
#35923=CARTESIAN_POINT('Ctrl Pts',(2.14692294891978,-2.40354073201732,35.1437009098924));
#35924=CARTESIAN_POINT('Ctrl Pts',(2.16405060814628,-2.38811720508672,35.1451106139376));
#35925=CARTESIAN_POINT('Ctrl Pts',(2.1714966111556,-2.38134862713143,35.1457275392704));
#35926=CARTESIAN_POINT('Ctrl Pts',(2.18577929560792,-2.36824266797561,35.14691885616));
#35927=CARTESIAN_POINT('Ctrl Pts',(2.19262042788094,-2.36191026921959,35.1474930313998));
#35928=CARTESIAN_POINT('Ctrl Pts',(2.21046113508075,-2.34525195816643,35.1489998132359));
#35929=CARTESIAN_POINT('Ctrl Pts',(2.22141574557196,-2.33487842292567,35.1499344685525));
#35930=CARTESIAN_POINT('Ctrl Pts',(2.26262368632985,-2.29530380858307,35.1534867380244));
#35931=CARTESIAN_POINT('Ctrl Pts',(2.29237629209639,-2.2655895888391,35.1561267090831));
#35932=CARTESIAN_POINT('Ctrl Pts',(2.36498724047232,-2.19017740471364,35.1627633713943));
#35933=CARTESIAN_POINT('Ctrl Pts',(2.40710902354072,-2.14379733402282,35.1667898613596));
#35934=CARTESIAN_POINT('Ctrl Pts',(2.52683000432368,-2.00399387390788,35.1787689156205));
#35935=CARTESIAN_POINT('Ctrl Pts',(2.60052735404878,-1.9073841069181,35.1868540777386));
#35936=CARTESIAN_POINT('Ctrl Pts',(2.80829628852151,-1.60052450429051,35.2118120830906));
#35937=CARTESIAN_POINT('Ctrl Pts',(2.92360460029175,-1.37867950457497,35.2289539029287));
#35938=CARTESIAN_POINT('Ctrl Pts',(3.01975798738673,-1.12589116364772,35.2462198111673));
#35939=CARTESIAN_POINT('Ctrl Pts',(3.02711712655888,-1.1059526089785,35.2475666645863));
#35940=CARTESIAN_POINT('Ctrl Pts',(3.03715400392429,-1.07790812734312,35.2494387003354));
#35941=CARTESIAN_POINT('Ctrl Pts',(3.03999741382545,-1.06986265586188,35.2499731902159));
#35942=CARTESIAN_POINT('Ctrl Pts',(3.04453383113319,-1.05686267995059,35.250832584171));
#35943=CARTESIAN_POINT('Ctrl Pts',(3.04624675537791,-1.05191524348307,35.2511586578931));
#35944=CARTESIAN_POINT('Ctrl Pts',(3.0498223232361,-1.04150595757504,35.2518426002686));
#35945=CARTESIAN_POINT('Ctrl Pts',(3.05168236362497,-1.03604324970668,35.2522003070227));
#35946=CARTESIAN_POINT('Ctrl Pts',(3.05618729722679,-1.02269542692598,35.2530714324032));
#35947=CARTESIAN_POINT('Ctrl Pts',(3.05881638239471,-1.01480494401201,35.2535839185662));
#35948=CARTESIAN_POINT('Ctrl Pts',(3.06812182888641,-0.98651245021176,35.2554129612008));
#35949=CARTESIAN_POINT('Ctrl Pts',(3.07462502953678,-0.966053495529832,
35.2567196951894));
#35950=CARTESIAN_POINT('Ctrl Pts',(3.11354420921741,-0.839238949451706,
35.264730398011));
#35951=CARTESIAN_POINT('Ctrl Pts',(3.14064605225898,-0.73131878439612,35.2711631847051));
#35952=CARTESIAN_POINT('Ctrl Pts',(3.20228605224234,-0.418056310754366,
35.2892997880465));
#35953=CARTESIAN_POINT('Ctrl Pts',(3.22259086965953,-0.210506202816104,
35.3006989395904));
#35954=CARTESIAN_POINT('Ctrl Pts',(3.2227490683711,-0.00245047203661506,
35.3125268034609));
#35955=CARTESIAN_POINT('Origin',(0.,0.,35.));
#35956=CARTESIAN_POINT('Origin',(0.,0.,32.));
#35957=CARTESIAN_POINT('Ctrl Pts',(3.9378436511043,0.00226769081060172,
37.4041617293967));
#35958=CARTESIAN_POINT('Ctrl Pts',(3.92969352726255,-1.17026837568043,37.3446443126903));
#35959=CARTESIAN_POINT('Ctrl Pts',(2.75095850512379,-3.66336727924014,37.2188159165294));
#35960=CARTESIAN_POINT('Ctrl Pts',(-1.49285278529501,-4.40632793330521,
37.026676540914));
#35961=CARTESIAN_POINT('Ctrl Pts',(-4.51432818846032,-1.12480055766829,
36.8277436025506));
#35962=CARTESIAN_POINT('Ctrl Pts',(-3.38576122948677,3.19076106622442,36.6288106641873));
#35963=CARTESIAN_POINT('Ctrl Pts',(0.855351370873146,4.57304158308359,36.4298777258236));
#35964=CARTESIAN_POINT('Ctrl Pts',(3.60300821559048,2.32885918759836,36.2716625040733));
#35965=CARTESIAN_POINT('Ctrl Pts',(3.93054449524549,0.509825557930273,36.1797582617771));
#35966=CARTESIAN_POINT('Ctrl Pts',(3.92785313095816,0.00233337176097839,
36.1541649989355));
#35967=CARTESIAN_POINT('Ctrl Pts',(-2.28358776666034,3.20569428094324,6.5881335146371));
#35968=CARTESIAN_POINT('Ctrl Pts',(-3.35286492248133,2.44407649255814,6.65448899198165));
#35969=CARTESIAN_POINT('Ctrl Pts',(-4.64957922564859,-0.219617924792526,
6.78715544878067));
#35970=CARTESIAN_POINT('Ctrl Pts',(-2.32229699647965,-4.03879127370882,
6.98613288503415));
#35971=CARTESIAN_POINT('Ctrl Pts',(2.14152197144423,-4.13253673306908,7.18506582339759));
#35972=CARTESIAN_POINT('Ctrl Pts',(4.6354962344389,-0.433054729749735,7.38399876176103));
#35973=CARTESIAN_POINT('Ctrl Pts',(2.86863005376323,3.66754880853003,7.58293170012447));
#35974=CARTESIAN_POINT('Ctrl Pts',(-1.53568971473972,4.39499028421212,7.7818646384879));
#35975=CARTESIAN_POINT('Ctrl Pts',(-4.52808181481838,1.08291459320159,7.98079757685135));
#35976=CARTESIAN_POINT('Ctrl Pts',(-3.35787183100746,-3.22511561142074,
8.17973051521478));
#35977=CARTESIAN_POINT('Ctrl Pts',(0.899288778474051,-4.56806013476469,
8.37866345357823));
#35978=CARTESIAN_POINT('Ctrl Pts',(4.32970627742076,-1.7116822031998,8.57759639194166));
#35979=CARTESIAN_POINT('Ctrl Pts',(3.77981709720475,2.71831339521054,8.77652933030509));
#35980=CARTESIAN_POINT('Ctrl Pts',(-0.244881287865563,4.64931963845551,
8.97546226866854));
#35981=CARTESIAN_POINT('Ctrl Pts',(-4.04445595226873,2.30620171359066,9.17439520703196));
#35982=CARTESIAN_POINT('Ctrl Pts',(-4.12594562258144,-2.15702647441609,
9.37332814539542));
#35983=CARTESIAN_POINT('Ctrl Pts',(-0.414433902178747,-4.63728597633392,
9.57226108375884));
#35984=CARTESIAN_POINT('Ctrl Pts',(3.6780683225737,-2.85446979798575,9.77119402212229));
#35985=CARTESIAN_POINT('Ctrl Pts',(4.38930591019076,1.55247461807464,9.97012696048572));
#35986=CARTESIAN_POINT('Ctrl Pts',(1.06543455816436,4.53222144777138,10.1690598988492));
#35987=CARTESIAN_POINT('Ctrl Pts',(-3.23789554621589,3.34547689252468,10.3679928372126));
#35988=CARTESIAN_POINT('Ctrl Pts',(-4.56461363563294,-0.916779903504382,
10.566925775576));
#35989=CARTESIAN_POINT('Ctrl Pts',(-1.69506170633405,-4.33623668960493,
10.7658587139395));
#35990=CARTESIAN_POINT('Ctrl Pts',(2.73276812195122,-3.76937148311671,10.9647916523029));
#35991=CARTESIAN_POINT('Ctrl Pts',(4.64835183630865,0.262694034166192,11.1637245906663));
#35992=CARTESIAN_POINT('Ctrl Pts',(2.29068463981999,4.05326372260543,11.3626575290298));
#35993=CARTESIAN_POINT('Ctrl Pts',(-2.17281932557235,4.11764970909905,11.5615904673932));
#35994=CARTESIAN_POINT('Ctrl Pts',(-4.63884063895772,0.396661654349383,
11.7605234057567));
#35995=CARTESIAN_POINT('Ctrl Pts',(-2.84035473048496,-3.68897925500734,
11.9594563441201));
#35996=CARTESIAN_POINT('Ctrl Pts',(1.56928215333904,-4.38332481861607,12.1583892824835));
#35997=CARTESIAN_POINT('Ctrl Pts',(4.53627084208731,-1.04806001180736,12.357322220847));
#35998=CARTESIAN_POINT('Ctrl Pts',(3.33304518836854,3.25069111315414,12.5562551592104));
#35999=CARTESIAN_POINT('Ctrl Pts',(-0.934264011548026,4.56106716657885,
12.7551880975738));
#36000=CARTESIAN_POINT('Ctrl Pts',(-4.34270007180307,1.67843350404123,12.9541210359373));
#36001=CARTESIAN_POINT('Ctrl Pts',(-3.75887227597289,-2.74719168498093,
13.1530539743007));
#36002=CARTESIAN_POINT('Ctrl Pts',(0.280503837458128,-4.6473111084089,13.3519869126642));
#36003=CARTESIAN_POINT('Ctrl Pts',(4.0620115019401,-2.27513636937342,13.5509198510276));
#36004=CARTESIAN_POINT('Ctrl Pts',(4.10929358463094,2.18858154439125,13.749852789391));
#36005=CARTESIAN_POINT('Ctrl Pts',(0.378883452643525,4.64032652627596,13.9487857277545));
#36006=CARTESIAN_POINT('Ctrl Pts',(-3.6998359543678,2.82619830371296,14.1477186661179));
#36007=CARTESIAN_POINT('Ctrl Pts',(-4.37727940176434,-1.5860668271018,14.3466516044813));
#36008=CARTESIAN_POINT('Ctrl Pts',(-1.03067005834432,-4.54025353608988,
14.5455845428448));
#36009=CARTESIAN_POINT('Ctrl Pts',(3.26343894045982,-3.32056459401619,14.7445174812082));
#36010=CARTESIAN_POINT('Ctrl Pts',(4.55745373218093,0.951734427334463,14.9434504195717));
#36011=CARTESIAN_POINT('Ctrl Pts',(1.66178065462684,4.34909967660568,15.1423833579351));
#36012=CARTESIAN_POINT('Ctrl Pts',(-2.7615749095149,3.74831788410233,15.3413162962985));
#36013=CARTESIAN_POINT('Ctrl Pts',(-4.64620214454805,-0.298309525729033,
15.540249234662));
#36014=CARTESIAN_POINT('Ctrl Pts',(-2.25955469263049,-4.07069963669087,
15.7391821730254));
#36015=CARTESIAN_POINT('Ctrl Pts',(2.20431162797926,-4.10087712421368,15.9381151113889));
#36016=CARTESIAN_POINT('Ctrl Pts',(4.64174427957893,-0.361099687260673,
16.1370480497523));
#36017=CARTESIAN_POINT('Ctrl Pts',(2.81200037969602,3.71063832860775,16.3359809881157));
#36018=CARTESIAN_POINT('Ctrl Pts',(-1.60282821254903,4.37116971326904,16.5349139264792));
#36019=CARTESIAN_POINT('Ctrl Pts',(-4.54416956536685,1.01326497143505,16.7338468648426));
#36020=CARTESIAN_POINT('Ctrl Pts',(-3.30803524366227,-3.27613885051165,
16.932779803206));
#36021=CARTESIAN_POINT('Ctrl Pts',(0.969190868759014,-4.55377338051179,
17.1317127415695));
#36022=CARTESIAN_POINT('Ctrl Pts',(4.35543542339085,-1.6451034052046,17.3306456799329));
#36023=CARTESIAN_POINT('Ctrl Pts',(3.73770845551644,2.77591758571908,17.5295786182963));
#36024=CARTESIAN_POINT('Ctrl Pts',(-0.316110833907594,4.64502496030214,
17.7285115566598));
#36025=CARTESIAN_POINT('Ctrl Pts',(-4.07932800118232,2.24393983874646,17.9274444950232));
#36026=CARTESIAN_POINT('Ctrl Pts',(-4.09240045043936,-2.22000934556306,
18.1263774333867));
#36027=CARTESIAN_POINT('Ctrl Pts',(-0.343310619835542,-4.64309387794946,
18.3253103717501));
#36028=CARTESIAN_POINT('Ctrl Pts',(3.72138621938403,-2.79776116695515,18.5242433101136));
#36029=CARTESIAN_POINT('Ctrl Pts',(4.36499584269893,1.61956606359996,18.723176248477));
#36030=CARTESIAN_POINT('Ctrl Pts',(0.995845006712163,4.54801887240478,18.9221091868404));
#36031=CARTESIAN_POINT('Ctrl Pts',(-3.28879065687452,3.29545732128312,19.1210421252039));
#36032=CARTESIAN_POINT('Ctrl Pts',(-4.55002616559029,-0.986633079511998,
19.3199750635673));
#36033=CARTESIAN_POINT('Ctrl Pts',(-1.62840200065756,-4.36170721912855,
19.5189080019307));
#36034=CARTESIAN_POINT('Ctrl Pts',(2.79021950300484,-3.72704414599493,19.7178409402942));
#36035=CARTESIAN_POINT('Ctrl Pts',(4.64377957295296,0.333907500617121,19.9167738786576));
#36036=CARTESIAN_POINT('Ctrl Pts',(2.22829203699626,4.08789646872357,20.115706817021));
#36037=CARTESIAN_POINT('Ctrl Pts',(-2.23567446665327,4.08386368777145,20.3146397553845));
#36038=CARTESIAN_POINT('Ctrl Pts',(-4.6443753015709,0.325516511565617,20.5135726937479));
#36039=CARTESIAN_POINT('Ctrl Pts',(-2.78348087456552,-3.73207946888481,
20.7125056321114));
#36040=CARTESIAN_POINT('Ctrl Pts',(1.63628013449202,-4.35875788070528,20.9114385704748));
#36041=CARTESIAN_POINT('Ctrl Pts',(4.55180140068407,-0.978410419953773,
21.1103715088382));
#36042=CARTESIAN_POINT('Ctrl Pts',(3.28283101156097,3.30139417378129,21.3093044472017));
#36043=CARTESIAN_POINT('Ctrl Pts',(-1.00406080348858,4.54621214243697,21.5082373855651));
#36044=CARTESIAN_POINT('Ctrl Pts',(-4.36791497172966,1.61167668621328,21.7071703239285));
#36045=CARTESIAN_POINT('Ctrl Pts',(-3.71632511212236,-2.80448045137639,
21.906103262292));
#36046=CARTESIAN_POINT('Ctrl Pts',(0.351699264548243,-4.64246600078663,
22.1050362006554));
#36047=CARTESIAN_POINT('Ctrl Pts',(4.0964049135034,-2.21261151713735,22.3039691390189));
#36048=CARTESIAN_POINT('Ctrl Pts',(4.07526696155566,2.25130676123813,22.5029020773823));
#36049=CARTESIAN_POINT('Ctrl Pts',(0.307717623722685,4.64558853162805,22.7018350157458));
#36050=CARTESIAN_POINT('Ctrl Pts',(-3.74271792010062,2.76915971220537,22.9007679541091));
#36051=CARTESIAN_POINT('Ctrl Pts',(-4.35245591888036,-1.65297017981175,
23.0997008924726));
#36052=CARTESIAN_POINT('Ctrl Pts',(-0.96096146715276,-4.55551709466568,
23.298633830836));
#36053=CARTESIAN_POINT('Ctrl Pts',(3.31394921617401,-3.27015649988854,23.4975667691995));
#36054=CARTESIAN_POINT('Ctrl Pts',(4.54233136705332,1.02147378479679,23.6964997075629));
#36055=CARTESIAN_POINT('Ctrl Pts',(1.59492770745015,4.37405859004556,23.8954326459263));
#36056=CARTESIAN_POINT('Ctrl Pts',(-2.8187002214397,3.70555151128673,24.0943655842898));
#36057=CARTESIAN_POINT('Ctrl Pts',(-4.64108426309036,-0.369485864463859,
24.2932985226532));
#36058=CARTESIAN_POINT('Ctrl Pts',(-2.19689850940736,-4.10485321059198,
24.4922314610167));
#36059=CARTESIAN_POINT('Ctrl Pts',(2.26690599978809,-4.06661039801803,24.6911643993801));
#36060=CARTESIAN_POINT('Ctrl Pts',(4.64673355030702,-0.289914217648445,
24.8900973377435));
#36061=CARTESIAN_POINT('Ctrl Pts',(2.75479789015282,3.75330141682668,25.089030276107));
#36062=CARTESIAN_POINT('Ctrl Pts',(-1.66963595449858,4.34609004975612,25.2879632144704));
#36063=CARTESIAN_POINT('Ctrl Pts',(-4.55916589979193,0.943498404512721,
25.4868961528339));
#36064=CARTESIAN_POINT('Ctrl Pts',(-3.25743397236614,-3.32645559970645,
25.6858290911973));
#36065=CARTESIAN_POINT('Ctrl Pts',(1.03887176776102,-4.5383838964209,25.8847620295608));
#36066=CARTESIAN_POINT('Ctrl Pts',(4.38013798386919,-1.57815531029427,26.0836949679242));
#36067=CARTESIAN_POINT('Ctrl Pts',(3.69472350167733,2.8328786044052,26.2826279062876));
#36068=CARTESIAN_POINT('Ctrl Pts',(-0.387267039202406,4.63963438015227,
26.4815608446511));
#36069=CARTESIAN_POINT('Ctrl Pts',(-4.11324123594255,2.18115324452121,26.6804937830145));
#36070=CARTESIAN_POINT('Ctrl Pts',(-4.05789412426333,-2.28247195325872,
26.8794267213779));
#36071=CARTESIAN_POINT('Ctrl Pts',(-0.272106554751227,-4.64781034079544,
27.0783596597414));
#36072=CARTESIAN_POINT('Ctrl Pts',(3.76382980366497,-2.74039561928326,27.2772925981048));
#36073=CARTESIAN_POINT('Ctrl Pts',(4.33966036680293,1.68627721384812,27.4762255364683));
#36074=CARTESIAN_POINT('Ctrl Pts',(0.926021488444692,4.56274776248724,27.6751584748317));
#36075=CARTESIAN_POINT('Ctrl Pts',(-3.33891314074683,3.24466361579928,27.8740914131951));
#36076=CARTESIAN_POINT('Ctrl Pts',(-4.53436978850062,-1.056254496926,28.0730243515586));
#36077=CARTESIAN_POINT('Ctrl Pts',(-1.56135974101536,-4.38615306393655,
28.271957289922));
#36078=CARTESIAN_POINT('Ctrl Pts',(2.84701539209114,-3.68384124228226,28.4708902282854));
#36079=CARTESIAN_POINT('Ctrl Pts',(4.63811637326107,0.405042527682263,28.6698231666489));
#36080=CARTESIAN_POINT('Ctrl Pts',(2.16537595366717,4.12156886639343,28.8687561050123));
#36081=CARTESIAN_POINT('Ctrl Pts',(-2.29800439309459,4.04911826827293,29.0676890433758));
#36082=CARTESIAN_POINT('Ctrl Pts',(-4.64881888728275,0.254294896501576,
29.2666219817392));
#36083=CARTESIAN_POINT('Ctrl Pts',(-2.72595311106574,-3.77430292602682,
29.4655549201026));
#36084=CARTESIAN_POINT('Ctrl Pts',(1.70289371351612,-4.33316696442807,29.6644878584661));
#36085=CARTESIAN_POINT('Ctrl Pts',(4.56626263015895,-0.908530975562921,
29.8634207968295));
#36086=CARTESIAN_POINT('Ctrl Pts',(3.23184561769564,3.35132165638052,30.0623537351929));
#36087=CARTESIAN_POINT('Ctrl Pts',(-1.07362171706024,4.53028910223179,30.2612866735564));
#36088=CARTESIAN_POINT('Ctrl Pts',(-4.39210374192795,1.54454124622366,30.4602196119198));
#36089=CARTESIAN_POINT('Ctrl Pts',(-3.67290489288628,-2.86111037692635,
30.6591525502832));
#36090=CARTESIAN_POINT('Ctrl Pts',(0.422812068905003,-4.63653026470569,
30.8580854886467));
#36091=CARTESIAN_POINT('Ctrl Pts',(4.12983597966957,-2.14956686850405,31.0570184270101));
#36092=CARTESIAN_POINT('Ctrl Pts',(4.04028295890316,2.31350309123207,31.2559513653736));
#36093=CARTESIAN_POINT('Ctrl Pts',(0.236479504429024,4.64975917496042,31.454884303737));
#36094=CARTESIAN_POINT('Ctrl Pts',(-3.78472063013482,2.71147057756036,31.6538172421005));
#36095=CARTESIAN_POINT('Ctrl Pts',(-4.32660993797449,-1.71948520952171,
31.8527501804639));
#36096=CARTESIAN_POINT('Ctrl Pts',(-0.891027122681378,-4.56971045119814,
32.0516831188273));
#36097=CARTESIAN_POINT('Ctrl Pts',(3.36368096441276,-3.21898016626241,32.2506160571907));
#36098=CARTESIAN_POINT('Ctrl Pts',(4.5261418975313,1.09097317316021,32.4495489955542));
#36099=CARTESIAN_POINT('Ctrl Pts',(1.52770007286572,4.39798993046933,32.6484819339176));
#36100=CARTESIAN_POINT('Ctrl Pts',(-2.87516335195365,3.66191461406821,32.8474148722811));
#36101=CARTESIAN_POINT('Ctrl Pts',(-4.63487607777506,-0.4405754019598,33.0463478106445));
#36102=CARTESIAN_POINT('Ctrl Pts',(-2.13372622115719,-4.13804245438466,
33.245280749008));
#36103=CARTESIAN_POINT('Ctrl Pts',(2.3289678201032,-4.03138832588321,33.4442136873714));
#36104=CARTESIAN_POINT('Ctrl Pts',(4.65063119002216,-0.218660640117578,
33.6431466257348));
#36105=CARTESIAN_POINT('Ctrl Pts',(2.69694823141472,3.79508276302539,33.8420795640982));
#36106=CARTESIAN_POINT('Ctrl Pts',(-1.73605145825132,4.31998938371931,34.0410125024617));
#36107=CARTESIAN_POINT('Ctrl Pts',(-4.57309117498029,0.873510186809756,
34.2399454408251));
#36108=CARTESIAN_POINT('Ctrl Pts',(-3.20606745040362,-3.37599088337116,
34.4388783791886));
#36109=CARTESIAN_POINT('Ctrl Pts',(1.10830861045392,-4.52192823529311,34.637811317552));
#36110=CARTESIAN_POINT('Ctrl Pts',(4.4038115431333,-1.51083646822047,34.8367442559154));
#36111=CARTESIAN_POINT('Ctrl Pts',(3.65087056719927,2.88917411083122,35.0356771942789));
#36112=CARTESIAN_POINT('Ctrl Pts',(-0.458332266027874,4.63315383676036,
35.2346101326423));
#36113=CARTESIAN_POINT('Ctrl Pts',(-4.1461881700408,2.11785424421031,35.4335430710058));
#36114=CARTESIAN_POINT('Ctrl Pts',(-4.02243449981698,-2.3443983526288,35.6324760093692));
#36115=CARTESIAN_POINT('Ctrl Pts',(-0.200838565195405,-4.65143491968315,
35.8314089477326));
#36116=CARTESIAN_POINT('Ctrl Pts',(3.80538917253758,-2.68238628582457,36.0303418860961));
#36117=CARTESIAN_POINT('Ctrl Pts',(4.313305398898,1.75259221639213,36.2292748244595));
#36118=CARTESIAN_POINT('Ctrl Pts',(0.855980425100957,4.57640475199999,36.428207762823));
#36119=CARTESIAN_POINT('Ctrl Pts',(-3.3882512324144,3.19310765946044,36.6271407011864));
#36120=CARTESIAN_POINT('Ctrl Pts',(-4.51764817756711,-1.1256277739117,36.8260736395498));
#36121=CARTESIAN_POINT('Ctrl Pts',(-1.49395067955099,-4.40956849538517,
37.0250065779133));
#36122=CARTESIAN_POINT('Ctrl Pts',(2.90314244717482,-3.63977291262905,37.2239395162767));
#36123=CARTESIAN_POINT('Ctrl Pts',(4.63136356822164,0.476082396912402,37.4228724546401));
#36124=CARTESIAN_POINT('Ctrl Pts',(2.10195116827292,4.15427301369114,37.6218053930036));
#36125=CARTESIAN_POINT('Ctrl Pts',(-2.35979445756394,4.01342159940947,37.820738331367));
#36126=CARTESIAN_POINT('Ctrl Pts',(-4.6521703611112,0.183013565819844,38.0196712697305));
#36127=CARTESIAN_POINT('Ctrl Pts',(-2.66778493740627,-3.81563975427051,
38.2186042080939));
#36128=CARTESIAN_POINT('Ctrl Pts',(1.76910720810075,-4.30655799166989,38.4175371464573));
#36129=CARTESIAN_POINT('Ctrl Pts',(4.57965119683031,-0.838438267478442,
38.6164700848208));
#36130=CARTESIAN_POINT('Ctrl Pts',(3.18010086249031,3.40046216234224,38.8154030231842));
#36131=CARTESIAN_POINT('Ctrl Pts',(-1.14293017678358,4.51330115287866,39.0143359615477));
#36132=CARTESIAN_POINT('Ctrl Pts',(-4.4152611484038,1.47704417104799,39.2132688999111));
#36133=CARTESIAN_POINT('Ctrl Pts',(-3.6286209586944,-2.91707048796121,39.4122018382745));
#36134=CARTESIAN_POINT('Ctrl Pts',(0.493823895339948,-4.62950082687821,
39.6111347766379));
#36135=CARTESIAN_POINT('Ctrl Pts',(4.16230000860224,-2.08602580072547,39.8100677150015));
#36136=CARTESIAN_POINT('Ctrl Pts',(4.00434373250677,2.37517234857208,40.0090006533648));
#36137=CARTESIAN_POINT('Ctrl Pts',(0.16519745519922,4.6528059816321,40.2079335917283));
#36138=CARTESIAN_POINT('Ctrl Pts',(-3.82585650677666,2.65320484133016,40.4068665300917));
#36139=CARTESIAN_POINT('Ctrl Pts',(-4.29970479193952,-1.78571208206424,
40.6057994684551));
#36140=CARTESIAN_POINT('Ctrl Pts',(-0.820965403692237,-4.58260824249866,
40.8047324068186));
#36141=CARTESIAN_POINT('Ctrl Pts',(3.41277964200003,-3.16747340374845,41.003665345182));
#36142=CARTESIAN_POINT('Ctrl Pts',(4.50858774680517,1.16103327592888,41.2025982835454));
#36143=CARTESIAN_POINT('Ctrl Pts',(1.46069211445911,4.41931609540443,41.4015312219089));
#36144=CARTESIAN_POINT('Ctrl Pts',(-2.93206675809147,3.62048102032587,41.6004641602723));
#36145=CARTESIAN_POINT('Ctrl Pts',(-4.62538118106894,-0.517884424352666,
41.7993970986358));
#36146=CARTESIAN_POINT('Ctrl Pts',(-2.92506802252003,-2.94215747695014,
41.9320190575447));
#36147=CARTESIAN_POINT('Ctrl Pts',(-1.74998052418886,-3.52545282590189,
41.9983300369992));
#36148=CARTESIAN_POINT('Ctrl Pts',(-2.14454317821952,3.01050386677641,6.72649619915742));
#36149=CARTESIAN_POINT('Ctrl Pts',(-3.14871348584711,2.29525996140177,6.79285167650196));
#36150=CARTESIAN_POINT('Ctrl Pts',(-4.36647259874689,-0.206245684665433,
6.92551813330099));
#36151=CARTESIAN_POINT('Ctrl Pts',(-2.18089545508631,-3.7928747038927,7.12449556955447));
#36152=CARTESIAN_POINT('Ctrl Pts',(2.01112757824255,-3.88091212828921,7.32342850791792));
#36153=CARTESIAN_POINT('Ctrl Pts',(4.35324710193498,-0.406686609570857,
7.52236144628135));
#36154=CARTESIAN_POINT('Ctrl Pts',(2.69396302714936,3.44423669322017,7.7212943846448));
#36155=CARTESIAN_POINT('Ctrl Pts',(-1.44218363300452,4.12738523561646,7.92022732300823));
#36156=CARTESIAN_POINT('Ctrl Pts',(-4.25237300188823,1.01697737978396,8.11916026137167));
#36157=CARTESIAN_POINT('Ctrl Pts',(-3.15341553044576,-3.02874265855638,
8.31809319973511));
#36158=CARTESIAN_POINT('Ctrl Pts',(0.844532293999059,-4.28991709569067,
8.51702613809854));
#36159=CARTESIAN_POINT('Ctrl Pts',(4.06607628421319,-1.60746017549409,8.71595907646199));
#36160=CARTESIAN_POINT('Ctrl Pts',(3.54966911676128,2.55279894780965,8.91489201482541));
#36161=CARTESIAN_POINT('Ctrl Pts',(-0.229970795531832,4.36622881746894,
9.11382495318887));
#36162=CARTESIAN_POINT('Ctrl Pts',(-3.79819446779221,2.16578019232958,9.31275789155229));
#36163=CARTESIAN_POINT('Ctrl Pts',(-3.87472234165631,-2.02568803287688,
9.51169082991574));
#36164=CARTESIAN_POINT('Ctrl Pts',(-0.389199579151803,-4.35492786885263,
9.71062376827917));
#36165=CARTESIAN_POINT('Ctrl Pts',(3.45411568819898,-2.6806649703053,9.90955670664261));
#36166=CARTESIAN_POINT('Ctrl Pts',(4.12204697548566,1.45794652614552,10.1084896450061));
#36167=CARTESIAN_POINT('Ctrl Pts',(1.00056168057528,4.25626057815718,10.3074225833695));
#36168=CARTESIAN_POINT('Ctrl Pts',(-3.04074444030663,3.14177530310008,10.5063555217329));
#36169=CARTESIAN_POINT('Ctrl Pts',(-4.28668044925664,-0.860958407946073,
10.7052884600964));
#36170=CARTESIAN_POINT('Ctrl Pts',(-1.59185167833342,-4.07220906838072,
10.9042213984598));
#36171=CARTESIAN_POINT('Ctrl Pts',(2.56637354567592,-3.53985952206916,11.1031543368232));
#36172=CARTESIAN_POINT('Ctrl Pts',(4.36531994349343,0.246698947662476,11.3020872751867));
#36173=CARTESIAN_POINT('Ctrl Pts',(2.15120793231547,3.80646594483665,11.5010202135501));
#36174=CARTESIAN_POINT('Ctrl Pts',(-2.04051927856241,3.86693155519059,11.6999531519136));
#36175=CARTESIAN_POINT('Ctrl Pts',(-4.35638787015977,0.372509459594964,
11.898886090277));
#36176=CARTESIAN_POINT('Ctrl Pts',(-2.66740935028452,-3.46436226862834,
12.0978190286404));
#36177=CARTESIAN_POINT('Ctrl Pts',(1.47373067318826,-4.11643006453438,12.2967519670039));
#36178=CARTESIAN_POINT('Ctrl Pts',(4.2600634102983,-0.984245046982922,12.4956849053673));
#36179=CARTESIAN_POINT('Ctrl Pts',(3.13010054869347,3.05276090237982,12.6946178437308));
#36180=CARTESIAN_POINT('Ctrl Pts',(-0.877377932161288,4.28334991993443,
12.8935507820942));
#36181=CARTESIAN_POINT('Ctrl Pts',(-4.07827890392793,1.57623594491877,13.0924837204576));
#36182=CARTESIAN_POINT('Ctrl Pts',(-3.52999959753036,-2.57991887734767,
13.2914166588211));
#36183=CARTESIAN_POINT('Ctrl Pts',(0.263424335980266,-4.36434258411605,
13.4903495971845));
#36184=CARTESIAN_POINT('Ctrl Pts',(3.8146810836505,-2.1366063751491,13.6892825355479));
#36185=CARTESIAN_POINT('Ctrl Pts',(3.85908422390511,2.05532175707241,13.8882154739114));
#36186=CARTESIAN_POINT('Ctrl Pts',(0.355813748685168,4.35778328379722,14.0871484122748));
#36187=CARTESIAN_POINT('Ctrl Pts',(-3.47455791816341,2.65411488930297,14.2860813506383));
#36188=CARTESIAN_POINT('Ctrl Pts',(-4.11075274498564,-1.48949335073545,
14.4850142890017));
#36189=CARTESIAN_POINT('Ctrl Pts',(-0.967913944402505,-4.26380360341846,
14.6839472273652));
#36190=CARTESIAN_POINT('Ctrl Pts',(3.06473253162247,-3.11837988094897,14.8828801657286));
#36191=CARTESIAN_POINT('Ctrl Pts',(4.27995650269812,0.893784597822432,15.081813104092));
#36192=CARTESIAN_POINT('Ctrl Pts',(1.56059706511263,4.08428884539946,15.2807460424554));
#36193=CARTESIAN_POINT('Ctrl Pts',(-2.59342632668046,3.52008784838862,15.4796789808189));
#36194=CARTESIAN_POINT('Ctrl Pts',(-4.3633011435735,-0.280145859835127,
15.6786119191823));
#36195=CARTESIAN_POINT('Ctrl Pts',(-2.12197344575085,-3.82284020955897,
15.8775448575457));
#36196=CARTESIAN_POINT('Ctrl Pts',(2.0700940570225,-3.8511802304453,16.0764777959092));
#36197=CARTESIAN_POINT('Ctrl Pts',(4.35911471200799,-0.339112812863191,
16.2754107342726));
#36198=CARTESIAN_POINT('Ctrl Pts',(2.6407814577879,3.48470255036153,16.4743436726361));
#36199=CARTESIAN_POINT('Ctrl Pts',(-1.50523415796133,4.10501506720731,16.6732766109995));
#36200=CARTESIAN_POINT('Ctrl Pts',(-4.26748119093852,0.951568629831059,
16.8722095493629));
#36201=CARTESIAN_POINT('Ctrl Pts',(-3.10661342589027,-3.07665916122845,
17.0711424877264));
#36202=CARTESIAN_POINT('Ctrl Pts',(0.910178140001792,-4.27650024269325,
17.2700754260898));
#36203=CARTESIAN_POINT('Ctrl Pts',(4.09023881708235,-1.54493527098234,17.4690083644533));
#36204=CARTESIAN_POINT('Ctrl Pts',(3.51012441364316,2.60689569661673,17.6679413028167));
#36205=CARTESIAN_POINT('Ctrl Pts',(-0.296863270295577,4.36219563649339,
17.8668742411801));
#36206=CARTESIAN_POINT('Ctrl Pts',(-3.83094320453884,2.10730935932299,18.0658071795436));
#36207=CARTESIAN_POINT('Ctrl Pts',(-3.84321968993877,-2.08483596169087,
18.264740117907));
#36208=CARTESIAN_POINT('Ctrl Pts',(-0.322406897833154,-4.3603821351485,
18.4636730562704));
#36209=CARTESIAN_POINT('Ctrl Pts',(3.4947960165208,-2.62740925156378,18.6626059946339));
#36210=CARTESIAN_POINT('Ctrl Pts',(4.09921711531441,1.52095286376864,18.8615389329973));
#36211=CARTESIAN_POINT('Ctrl Pts',(0.935209343336036,4.27109611884696,19.0604718713608));
#36212=CARTESIAN_POINT('Ctrl Pts',(-3.08854061611436,3.09480135629163,19.2594048097242));
#36213=CARTESIAN_POINT('Ctrl Pts',(-4.27298119064957,-0.926558317996034,
19.4583377480876));
#36214=CARTESIAN_POINT('Ctrl Pts',(-1.52925079250028,-4.09612873161108,
19.6572706864511));
#36215=CARTESIAN_POINT('Ctrl Pts',(2.62032678939031,-3.50010943958843,19.8562036248145));
#36216=CARTESIAN_POINT('Ctrl Pts',(4.36102607910528,0.313576321899792,20.055136563178));
#36217=CARTESIAN_POINT('Ctrl Pts',(2.09261433118024,3.83898994961327,20.2540695015414));
#36218=CARTESIAN_POINT('Ctrl Pts',(-2.09954725462231,3.83520271927058,20.4530024399048));
#36219=CARTESIAN_POINT('Ctrl Pts',(-4.36158553460872,0.30569624888859,20.6519353782683));
#36220=CARTESIAN_POINT('Ctrl Pts',(-2.61399846697548,-3.50483816843836,
20.8508683166317));
#36221=CARTESIAN_POINT('Ctrl Pts',(1.53664923735901,-4.09335897443855,21.0498012549951));
#36222=CARTESIAN_POINT('Ctrl Pts',(4.27464833406557,-0.918836325121606,
21.2487341933586));
#36223=CARTESIAN_POINT('Ctrl Pts',(3.08294384559025,3.10037672182424,21.447667131722));
#36224=CARTESIAN_POINT('Ctrl Pts',(-0.942924891294206,4.26939939823746,
21.6466000700854));
#36225=CARTESIAN_POINT('Ctrl Pts',(-4.10195850250371,1.51354385996249,21.8455330084489));
#36226=CARTESIAN_POINT('Ctrl Pts',(-3.49004307327481,-2.63371940779178,
22.0444659468123));
#36227=CARTESIAN_POINT('Ctrl Pts',(0.330284769249194,-4.35979248858183,
22.2433988851758));
#36228=CARTESIAN_POINT('Ctrl Pts',(3.84698032663149,-2.07788857709042,22.4423318235392));
#36229=CARTESIAN_POINT('Ctrl Pts',(3.82712943615432,2.11422771981017,22.6412647619026));
#36230=CARTESIAN_POINT('Ctrl Pts',(0.288981111392786,4.36272489271909,22.8401977002661));
#36231=CARTESIAN_POINT('Ctrl Pts',(-3.51482885866484,2.6005493009342,23.0391306386295));
#36232=CARTESIAN_POINT('Ctrl Pts',(-4.08744073059509,-1.5523230482618,23.238063576993));
#36233=CARTESIAN_POINT('Ctrl Pts',(-0.902449815593572,-4.27813778443702,
23.4369965153564));
#36234=CARTESIAN_POINT('Ctrl Pts',(3.11216730456806,-3.07104106789052,23.6359294537198));
#36235=CARTESIAN_POINT('Ctrl Pts',(4.26575491804855,0.959277619585273,23.8348623920833));
#36236=CARTESIAN_POINT('Ctrl Pts',(1.4978147039944,4.10772804416148,24.0337953304467));
#36237=CARTESIAN_POINT('Ctrl Pts',(-2.64707335517684,3.47992546250712,24.2327282688101));
#36238=CARTESIAN_POINT('Ctrl Pts',(-4.35849488303591,-0.346988367013049,
24.4316612071736));
#36239=CARTESIAN_POINT('Ctrl Pts',(-2.06313231327231,-3.85491421827051,
24.630594145537));
#36240=CARTESIAN_POINT('Ctrl Pts',(2.12887714170064,-3.81899995913029,24.8295270839005));
#36241=CARTESIAN_POINT('Ctrl Pts',(4.36380019275037,-0.272261730774709,
25.0284600222639));
#36242=CARTESIAN_POINT('Ctrl Pts',(2.58706195091454,3.52476794050656,25.2273929606274));
#36243=CARTESIAN_POINT('Ctrl Pts',(-1.56797406633792,4.08146247068183,25.4263258989908));
#36244=CARTESIAN_POINT('Ctrl Pts',(-4.28156441872558,0.886050055355632,
25.6252588373542));
#36245=CARTESIAN_POINT('Ctrl Pts',(-3.05909319796137,-3.12391219122417,
25.8241917757177));
#36246=CARTESIAN_POINT('Ctrl Pts',(0.975616262761357,-4.2620478035949,26.0231247140811));
#36247=CARTESIAN_POINT('Ctrl Pts',(4.11343727186996,-1.48206355554802,26.2220576524445));
#36248=CARTESIAN_POINT('Ctrl Pts',(3.46975675584276,2.6603884354688,26.4209905908079));
#36249=CARTESIAN_POINT('Ctrl Pts',(-0.363686869931574,4.35713328152031,
26.6199235291714));
#36250=CARTESIAN_POINT('Ctrl Pts',(-3.86279150803662,2.0483457563929,26.8188564675348));
#36251=CARTESIAN_POINT('Ctrl Pts',(-3.810814407564,-2.14349530519553,27.0177894058983));
#36252=CARTESIAN_POINT('Ctrl Pts',(-0.255538352525876,-4.36481141891387,
27.2167223442617));
#36253=CARTESIAN_POINT('Ctrl Pts',(3.53465526802747,-2.57353661495193,27.4156552826252));
#36254=CARTESIAN_POINT('Ctrl Pts',(4.07542428247787,1.58360206178266,27.6145882209886));
#36255=CARTESIAN_POINT('Ctrl Pts',(0.869637285206309,4.28492818661779,27.813521159352));
#36256=CARTESIAN_POINT('Ctrl Pts',(-3.13561120934189,3.04710041123396,28.0124540977155));
#36257=CARTESIAN_POINT('Ctrl Pts',(-4.25827810930823,-0.99194058092151,
28.2113870360789));
#36258=CARTESIAN_POINT('Ctrl Pts',(-1.46629064589802,-4.11908610180032,
28.4103199744424));
#36259=CARTESIAN_POINT('Ctrl Pts',(2.67366445316185,-3.4595371025892,28.6092529128058));
#36260=CARTESIAN_POINT('Ctrl Pts',(4.35570770402749,0.380380032820054,28.8081858511692));
#36261=CARTESIAN_POINT('Ctrl Pts',(2.03352912356371,3.87061208026725,29.0071187895327));
#36262=CARTESIAN_POINT('Ctrl Pts',(-2.15808199565578,3.80257290164423,29.2060517278961));
#36263=CARTESIAN_POINT('Ctrl Pts',(-4.36575855636173,0.238811222196252,
29.4049846662595));
#36264=CARTESIAN_POINT('Ctrl Pts',(-2.55997349163937,-3.5444906960516,29.603917604623));
#36265=CARTESIAN_POINT('Ctrl Pts',(1.59920680512957,-4.06932625464213,29.8028505429864));
#36266=CARTESIAN_POINT('Ctrl Pts',(4.2882290387233,-0.853211746134946,30.0017834813498));
#36267=CARTESIAN_POINT('Ctrl Pts',(3.03506288379887,3.14726418714398,30.2007164197133));
#36268=CARTESIAN_POINT('Ctrl Pts',(-1.00825033437494,4.25444589053914,30.3996493580767));
#36269=CARTESIAN_POINT('Ctrl Pts',(-4.12467445101052,1.45049620663885,30.5985822964402));
#36270=CARTESIAN_POINT('Ctrl Pts',(-3.44926665280217,-2.68690121332354,
30.7975152348036));
#36271=CARTESIAN_POINT('Ctrl Pts',(0.397067610571902,-4.35421817148927,
30.996448173167));
#36272=CARTESIAN_POINT('Ctrl Pts',(3.87837582013254,-2.01868263233817,31.1953811115305));
#36273=CARTESIAN_POINT('Ctrl Pts',(3.7942755623814,2.17263699890429,31.3943140498939));
#36274=CARTESIAN_POINT('Ctrl Pts',(0.222080585391179,4.36664159118708,31.5932469882574));
#36275=CARTESIAN_POINT('Ctrl Pts',(-3.55427408016482,2.54637278012491,31.7921799266208));
#36276=CARTESIAN_POINT('Ctrl Pts',(-4.06316847671228,-1.61478806725346,
31.9911128649843));
#36277=CARTESIAN_POINT('Ctrl Pts',(-0.836773679318462,-4.2914669265756,
32.1900458033476));
#36278=CARTESIAN_POINT('Ctrl Pts',(3.15887095352933,-3.02298079240363,32.3889787417111));
#36279=CARTESIAN_POINT('Ctrl Pts',(4.25055120355625,1.02454528364496,32.5879116800745));
#36280=CARTESIAN_POINT('Ctrl Pts',(1.43468046968086,4.1302022374466,32.786844618438));
#36281=CARTESIAN_POINT('Ctrl Pts',(-2.70009852159804,3.43894555728302,32.9857775568014));
#36282=CARTESIAN_POINT('Ctrl Pts',(-4.3526647057765,-0.413749358162806,
33.1847104951649));
#36283=CARTESIAN_POINT('Ctrl Pts',(-2.00380650070783,-3.88608261363723,
33.3836434335282));
#36284=CARTESIAN_POINT('Ctrl Pts',(2.18716010122942,-3.7859225116057,33.5825763718918));
#36285=CARTESIAN_POINT('Ctrl Pts',(4.36746051042428,-0.205346687767176,
33.7815093102551));
#36286=CARTESIAN_POINT('Ctrl Pts',(2.53273468010832,3.56400527671735,33.9804422486186));
#36287=CARTESIAN_POINT('Ctrl Pts',(-1.63034561937406,4.05695103910325,34.179375186982));
#36288=CARTESIAN_POINT('Ctrl Pts',(-4.29464180263262,0.820323326117568,
34.3783081253455));
#36289=CARTESIAN_POINT('Ctrl Pts',(-3.01085431445013,-3.17043133807512,
34.5772410637089));
#36290=CARTESIAN_POINT('Ctrl Pts',(1.04082518947229,-4.24659410554575,34.7761740020724));
#36291=CARTESIAN_POINT('Ctrl Pts',(4.1356693799436,-1.41884366724649,34.9751069404358));
#36292=CARTESIAN_POINT('Ctrl Pts',(3.42857396757734,2.7132561842074,35.1740398787992));
#36293=CARTESIAN_POINT('Ctrl Pts',(-0.43042503065489,4.35104732970134,35.3729728171627));
#36294=CARTESIAN_POINT('Ctrl Pts',(-3.89373234762037,1.98890094709468,35.5719057555261));
#36295=CARTESIAN_POINT('Ctrl Pts',(-3.77751387196871,-2.2016510893785,35.7708386938896));
#36296=CARTESIAN_POINT('Ctrl Pts',(-0.188609775022207,-4.36821530206696,
35.969771632253));
#36297=CARTESIAN_POINT('Ctrl Pts',(3.57368414281305,-2.51905939180415,36.1687045706164));
#36298=CARTESIAN_POINT('Ctrl Pts',(4.05067403312995,1.64587923299354,36.3676375089799));
#36299=CARTESIAN_POINT('Ctrl Pts',(0.803860928027483,4.29775362040325,36.5665704473433));
#36300=CARTESIAN_POINT('Ctrl Pts',(-3.18194517095124,2.99868362775086,36.7655033857068));
#36301=CARTESIAN_POINT('Ctrl Pts',(-4.24257465477942,-1.05708981235569,
36.9644363240701));
#36302=CARTESIAN_POINT('Ctrl Pts',(-1.40298603154328,-4.14107579911404,
37.1633692624336));
#36303=CARTESIAN_POINT('Ctrl Pts',(2.72637400733384,-3.41815203427124,37.362302200797));
#36304=CARTESIAN_POINT('Ctrl Pts',(4.34936606820663,0.447094379937924,37.5612351391605));
#36305=CARTESIAN_POINT('Ctrl Pts',(1.97396618806673,3.90132491601227,37.7601680775239));
#36306=CARTESIAN_POINT('Ctrl Pts',(-2.21610974618682,3.76904975494763,37.9591010158874));
#36307=CARTESIAN_POINT('Ctrl Pts',(-4.3689059634554,0.17187011588989,38.1580339542508));
#36308=CARTESIAN_POINT('Ctrl Pts',(-2.50534709985704,-3.5833105804079,38.3569668926142));
#36309=CARTESIAN_POINT('Ctrl Pts',(1.66138864906423,-4.04433746645492,38.5558998309777));
#36310=CARTESIAN_POINT('Ctrl Pts',(4.30080239357324,-0.787386888794196,
38.7548327693411));
#36311=CARTESIAN_POINT('Ctrl Pts',(2.98646879715839,3.19341259377544,38.9537657077046));
#36312=CARTESIAN_POINT('Ctrl Pts',(-1.07333869518271,4.23849231457894,39.152698646068));
#36313=CARTESIAN_POINT('Ctrl Pts',(-4.14642183414512,1.38710893760937,39.3516315844314));
#36314=CARTESIAN_POINT('Ctrl Pts',(-3.40767910781596,-2.73945398844537,
39.5505645227949));
#36315=CARTESIAN_POINT('Ctrl Pts',(0.46375562238267,-4.34761674667882,39.7494974611583));
#36316=CARTESIAN_POINT('Ctrl Pts',(3.90886315799689,-1.9590104947349,39.9484303995218));
#36317=CARTESIAN_POINT('Ctrl Pts',(3.76052462715392,2.23055129808965,40.1473633378851));
#36318=CARTESIAN_POINT('Ctrl Pts',(0.155138804288171,4.36950288189749,40.3462962762487));
#36319=CARTESIAN_POINT('Ctrl Pts',(-3.59290524859212,2.49165476622559,40.545229214612));
#36320=CARTESIAN_POINT('Ctrl Pts',(-4.03790154884084,-1.67698247458014,
40.7441621529755));
#36321=CARTESIAN_POINT('Ctrl Pts',(-0.770977924188701,-4.3035793887071,
40.943095091339));
#36322=CARTESIAN_POINT('Ctrl Pts',(3.20498007865981,-2.97461020739956,41.1420280297023));
#36323=CARTESIAN_POINT('Ctrl Pts',(4.23406590146329,1.09033952096375,41.3409609680659));
#36324=CARTESIAN_POINT('Ctrl Pts',(1.37175253575807,4.15022988087543,41.5398939064291));
#36325=CARTESIAN_POINT('Ctrl Pts',(-2.75353715585242,3.40003479934917,41.7388268447928));
#36326=CARTESIAN_POINT('Ctrl Pts',(-4.34374794056332,-0.486351138137266,
41.9377597831561));
#36327=CARTESIAN_POINT('Ctrl Pts',(-2.74696456387898,-2.76301346440847,
42.0703817420651));
#36328=CARTESIAN_POINT('Ctrl Pts',(-1.64342656321671,-3.3107927439021,42.1366927215196));
#36329=CARTESIAN_POINT('Ctrl Pts',(-2.0054985897787,2.81531345260957,6.86485888367774));
#36330=CARTESIAN_POINT('Ctrl Pts',(-2.94456204921288,2.14644343024538,6.93121436102229));
#36331=CARTESIAN_POINT('Ctrl Pts',(-4.08336597184518,-0.19287344453834,
7.06388081782131));
#36332=CARTESIAN_POINT('Ctrl Pts',(-2.03949391369296,-3.54695813407657,
7.26285825407481));
#36333=CARTESIAN_POINT('Ctrl Pts',(1.88073318504086,-3.62928752350934,7.46179119243823));
#36334=CARTESIAN_POINT('Ctrl Pts',(4.07099796943106,-0.380318489391973,
7.66072413080168));
#36335=CARTESIAN_POINT('Ctrl Pts',(2.51929600053549,3.2209245779103,7.8596570691651));
#36336=CARTESIAN_POINT('Ctrl Pts',(-1.34867755126933,3.85978018702081,8.05859000752856));
#36337=CARTESIAN_POINT('Ctrl Pts',(-3.97666418895809,0.951040166366322,
8.25752294589198));
#36338=CARTESIAN_POINT('Ctrl Pts',(-2.94895922988404,-2.83236970569201,
8.45645588425543));
#36339=CARTESIAN_POINT('Ctrl Pts',(0.789775809524059,-4.01177405661665,
8.65538882261886));
#36340=CARTESIAN_POINT('Ctrl Pts',(3.80244629100563,-1.50323814778838,8.85432176098231));
#36341=CARTESIAN_POINT('Ctrl Pts',(3.31952113631781,2.38728450040875,9.05325469934573));
#36342=CARTESIAN_POINT('Ctrl Pts',(-0.2150603031981,4.08313799648236,9.25218763770918));
#36343=CARTESIAN_POINT('Ctrl Pts',(-3.5519329833157,2.02535867106851,9.45112057607261));
#36344=CARTESIAN_POINT('Ctrl Pts',(-3.62349906073116,-1.89434959133768,
9.65005351443604));
#36345=CARTESIAN_POINT('Ctrl Pts',(-0.363965256124856,-4.07256976137133,
9.84898645279951));
#36346=CARTESIAN_POINT('Ctrl Pts',(3.23016305382427,-2.50686014262486,10.0479193911629));
#36347=CARTESIAN_POINT('Ctrl Pts',(3.85478804078057,1.36341843421643,10.2468523295264));
#36348=CARTESIAN_POINT('Ctrl Pts',(0.93568880298618,3.98029970854296,10.4457852678898));
#36349=CARTESIAN_POINT('Ctrl Pts',(-2.84359333439737,2.9380737136755,10.6447182062533));
#36350=CARTESIAN_POINT('Ctrl Pts',(-4.00874726288035,-0.805136912387771,
10.8436511446167));
#36351=CARTESIAN_POINT('Ctrl Pts',(-1.48864165033278,-3.8081814471565,11.0425840829802));
#36352=CARTESIAN_POINT('Ctrl Pts',(2.39997896940062,-3.31034756102161,11.2415170213436));
#36353=CARTESIAN_POINT('Ctrl Pts',(4.0822880506782,0.23070386115876,11.440449959707));
#36354=CARTESIAN_POINT('Ctrl Pts',(2.01173122481096,3.55966816706786,11.6393828980705));
#36355=CARTESIAN_POINT('Ctrl Pts',(-1.90821923155247,3.61621340128212,11.8383158364339));
#36356=CARTESIAN_POINT('Ctrl Pts',(-4.07393510136182,0.34835726484055,12.0372487747973));
#36357=CARTESIAN_POINT('Ctrl Pts',(-2.49446397008411,-3.23974528224934,
12.2361817131608));
#36358=CARTESIAN_POINT('Ctrl Pts',(1.3781791930375,-3.84953531045267,12.4351146515242));
#36359=CARTESIAN_POINT('Ctrl Pts',(3.98385597850928,-0.920430082158486,
12.6340475898877));
#36360=CARTESIAN_POINT('Ctrl Pts',(2.92715590901843,2.8548306916055,12.8329805282511));
#36361=CARTESIAN_POINT('Ctrl Pts',(-0.820491852774556,4.00563267329001,
13.0319134666145));
#36362=CARTESIAN_POINT('Ctrl Pts',(-3.81385773605278,1.47403838579632,13.230846404978));
#36363=CARTESIAN_POINT('Ctrl Pts',(-3.30112691908783,-2.41264606971442,
13.4297793433414));
#36364=CARTESIAN_POINT('Ctrl Pts',(0.246344834502405,-4.0813740598232,13.6287122817048));
#36365=CARTESIAN_POINT('Ctrl Pts',(3.56735066536092,-1.99807638092479,13.8276452200683));
#36366=CARTESIAN_POINT('Ctrl Pts',(3.60887486317929,1.92206196975356,14.0265781584317));
#36367=CARTESIAN_POINT('Ctrl Pts',(0.332744044726809,4.07524004131849,14.2255110967952));
#36368=CARTESIAN_POINT('Ctrl Pts',(-3.24927988195903,2.48203147489298,14.4244440351586));
#36369=CARTESIAN_POINT('Ctrl Pts',(-3.84422608820695,-1.39291987436911,
14.623376973522));
#36370=CARTESIAN_POINT('Ctrl Pts',(-0.905157830460687,-3.98735367074704,
14.8223099118855));
#36371=CARTESIAN_POINT('Ctrl Pts',(2.86602612278512,-2.91619516788176,15.0212428502489));
#36372=CARTESIAN_POINT('Ctrl Pts',(4.00245927321531,0.835834768310396,15.2201757886123));
#36373=CARTESIAN_POINT('Ctrl Pts',(1.45941347559844,3.81947801419324,15.4191087269758));
#36374=CARTESIAN_POINT('Ctrl Pts',(-2.42527774384603,3.29185781267492,15.6180416653392));
#36375=CARTESIAN_POINT('Ctrl Pts',(-4.08040014259896,-0.261982193941216,
15.8169746037027));
#36376=CARTESIAN_POINT('Ctrl Pts',(-1.98439219887121,-3.57498078242707,
16.0159075420661));
#36377=CARTESIAN_POINT('Ctrl Pts',(1.93587648606574,-3.60148333667693,16.2148404804295));
#36378=CARTESIAN_POINT('Ctrl Pts',(4.07648514443705,-0.317125938465704,
16.413773418793));
#36379=CARTESIAN_POINT('Ctrl Pts',(2.46956253587978,3.25876677211529,16.6127063571564));
#36380=CARTESIAN_POINT('Ctrl Pts',(-1.40764010337363,3.8388604211456,16.8116392955199));
#36381=CARTESIAN_POINT('Ctrl Pts',(-3.99079281651019,0.889872288227052,
17.0105722338833));
#36382=CARTESIAN_POINT('Ctrl Pts',(-2.90519160811827,-2.87717947194522,
17.2095051722467));
#36383=CARTESIAN_POINT('Ctrl Pts',(0.851165411244564,-3.99922710487472,
17.4084381106102));
#36384=CARTESIAN_POINT('Ctrl Pts',(3.82504221077387,-1.44476713676006,17.6073710489736));
#36385=CARTESIAN_POINT('Ctrl Pts',(3.28254037176988,2.43787380751438,17.806303987337));
#36386=CARTESIAN_POINT('Ctrl Pts',(-0.277615706683554,4.07936631268466,
18.0052369257005));
#36387=CARTESIAN_POINT('Ctrl Pts',(-3.58255840789535,1.97067887989953,18.2041698640639));
#36388=CARTESIAN_POINT('Ctrl Pts',(-3.59403892943819,-1.94966257781868,
18.4031028024274));
#36389=CARTESIAN_POINT('Ctrl Pts',(-0.301503175830768,-4.07767039234755,
18.6020357407908));
#36390=CARTESIAN_POINT('Ctrl Pts',(3.26820581365757,-2.45705733617242,18.8009686791542));
#36391=CARTESIAN_POINT('Ctrl Pts',(3.83343838792988,1.42233966393734,18.9999016175177));
#36392=CARTESIAN_POINT('Ctrl Pts',(0.874573679959915,3.99417336528914,19.1988345558811));
#36393=CARTESIAN_POINT('Ctrl Pts',(-2.88829057535421,2.89414539130014,19.3977674942445));
#36394=CARTESIAN_POINT('Ctrl Pts',(-3.99593621570884,-0.866483556480068,
19.596700432608));
#36395=CARTESIAN_POINT('Ctrl Pts',(-1.43009958434302,-3.83055024409362,
19.7956333709714));
#36396=CARTESIAN_POINT('Ctrl Pts',(2.45043407577578,-3.27317473318194,19.9945663093349));
#36397=CARTESIAN_POINT('Ctrl Pts',(4.07827258525759,0.293245143182466,20.1934992476983));
#36398=CARTESIAN_POINT('Ctrl Pts',(1.95693662536422,3.59008343050296,20.3924321860618));
#36399=CARTESIAN_POINT('Ctrl Pts',(-1.96342004259136,3.58654175076973,20.5913651244252));
#36400=CARTESIAN_POINT('Ctrl Pts',(-4.07879576764655,0.285875986211559,
20.7902980627886));
#36401=CARTESIAN_POINT('Ctrl Pts',(-2.44451605938545,-3.27759686799192,
20.989231001152));
#36402=CARTESIAN_POINT('Ctrl Pts',(1.43701834022598,-3.82796006817182,21.1881639395155));
#36403=CARTESIAN_POINT('Ctrl Pts',(3.99749526744709,-0.85926223028944,21.3870968778789));
#36404=CARTESIAN_POINT('Ctrl Pts',(2.88305667961953,2.89935926986721,21.5860298162423));
#36405=CARTESIAN_POINT('Ctrl Pts',(-0.881788979099839,3.99258665403793,
21.7849627546059));
#36406=CARTESIAN_POINT('Ctrl Pts',(-3.83600203327774,1.41541103371171,21.9838956929692));
#36407=CARTESIAN_POINT('Ctrl Pts',(-3.26376103442727,-2.46295836420717,
22.1828286313327));
#36408=CARTESIAN_POINT('Ctrl Pts',(0.30887027395015,-4.07711897637704,22.3817615696961));
#36409=CARTESIAN_POINT('Ctrl Pts',(3.59755573975958,-1.94316563704349,22.5806945080596));
#36410=CARTESIAN_POINT('Ctrl Pts',(3.57899191075299,1.97714867838221,22.779627446423));
#36411=CARTESIAN_POINT('Ctrl Pts',(0.270244599062885,4.07986125381013,22.9785603847864));
#36412=CARTESIAN_POINT('Ctrl Pts',(-3.28693979722906,2.43193888966304,23.1774933231499));
#36413=CARTESIAN_POINT('Ctrl Pts',(-3.82242554230984,-1.45167591671186,
23.3764262615133));
#36414=CARTESIAN_POINT('Ctrl Pts',(-0.843938164034378,-4.00075847420837,
23.5753591998767));
#36415=CARTESIAN_POINT('Ctrl Pts',(2.91038539296211,-2.87192563589251,23.7742921382402));
#36416=CARTESIAN_POINT('Ctrl Pts',(3.98917846904379,0.897081454373756,23.9732250766036));
#36417=CARTESIAN_POINT('Ctrl Pts',(1.40070170053866,3.8413974982774,24.1721580149671));
#36418=CARTESIAN_POINT('Ctrl Pts',(-2.47544648891397,3.25429941372752,24.3710909533305));
#36419=CARTESIAN_POINT('Ctrl Pts',(-4.07590550298146,-0.324490869562239,
24.5700238916939));
#36420=CARTESIAN_POINT('Ctrl Pts',(-1.92936611713726,-3.60497522594906,
24.7689568300574));
#36421=CARTESIAN_POINT('Ctrl Pts',(1.9908482836132,-3.57138952024253,24.9678897684208));
#36422=CARTESIAN_POINT('Ctrl Pts',(4.08086683519371,-0.254609243900974,
25.1668227067842));
#36423=CARTESIAN_POINT('Ctrl Pts',(2.41932601167626,3.29623446418644,25.3657556451477));
#36424=CARTESIAN_POINT('Ctrl Pts',(-1.46631217817726,3.81683489160756,25.5646885835111));
#36425=CARTESIAN_POINT('Ctrl Pts',(-4.00396293765922,0.828601706198546,
25.7636215218746));
#36426=CARTESIAN_POINT('Ctrl Pts',(-2.86075242355659,-2.92136878274188,
25.962554460238));
#36427=CARTESIAN_POINT('Ctrl Pts',(0.912360757761685,-3.98571171076888,
26.1614873986014));
#36428=CARTESIAN_POINT('Ctrl Pts',(3.84673655987073,-1.38597180080177,26.3604203369649));
#36429=CARTESIAN_POINT('Ctrl Pts',(3.24479001000817,2.4878982665324,26.5593532753283));
#36430=CARTESIAN_POINT('Ctrl Pts',(-0.340106700660735,4.07463218288835,
26.7582862136918));
#36431=CARTESIAN_POINT('Ctrl Pts',(-3.61234178013069,1.91553826826458,26.9572191520552));
#36432=CARTESIAN_POINT('Ctrl Pts',(-3.56373469086466,-2.00451865713232,
27.1561520904186));
#36433=CARTESIAN_POINT('Ctrl Pts',(-0.238970150300533,-4.0818124970323,
27.355085028782));
#36434=CARTESIAN_POINT('Ctrl Pts',(3.30548073238998,-2.4066776106206,27.5540179671455));
#36435=CARTESIAN_POINT('Ctrl Pts',(3.81118819815281,1.4809269097172,27.7529509055089));
#36436=CARTESIAN_POINT('Ctrl Pts',(0.813253081967926,4.00710861074834,27.9518838438724));
#36437=CARTESIAN_POINT('Ctrl Pts',(-2.93230927793693,2.84953720666863,28.1508167822358));
#36438=CARTESIAN_POINT('Ctrl Pts',(-3.98218643011584,-0.927626664917013,
28.3497497205993));
#36439=CARTESIAN_POINT('Ctrl Pts',(-1.37122155078066,-3.85201913966408,
28.5486826589627));
#36440=CARTESIAN_POINT('Ctrl Pts',(2.50031351423257,-3.23523296289614,28.7476155973261));
#36441=CARTESIAN_POINT('Ctrl Pts',(4.07329903479392,0.355717537957839,28.9465485356896));
#36442=CARTESIAN_POINT('Ctrl Pts',(1.90168229346025,3.61965529414108,29.145481474053));
#36443=CARTESIAN_POINT('Ctrl Pts',(-2.01815959821697,3.55602753501551,29.3444144124164));
#36444=CARTESIAN_POINT('Ctrl Pts',(-4.08269822544072,0.223327547890934,
29.5433473507799));
#36445=CARTESIAN_POINT('Ctrl Pts',(-2.393993872213,-3.31467846607637,29.7422802891433));
#36446=CARTESIAN_POINT('Ctrl Pts',(1.49551989674303,-3.80548554485619,29.9412132275068));
#36447=CARTESIAN_POINT('Ctrl Pts',(4.01019544728766,-0.797892516706975,
30.1401461658702));
#36448=CARTESIAN_POINT('Ctrl Pts',(2.8382801499021,2.94320671790745,30.3390791042336));
#36449=CARTESIAN_POINT('Ctrl Pts',(-0.942878951689648,3.97860267884648,
30.5380120425971));
#36450=CARTESIAN_POINT('Ctrl Pts',(-3.85724516009308,1.35645116705405,30.7369449809605));
#36451=CARTESIAN_POINT('Ctrl Pts',(-3.22562841271805,-2.51269204972075,
30.935877919324));
#36452=CARTESIAN_POINT('Ctrl Pts',(0.371323152238799,-4.07190607827283,
31.1348108576874));
#36453=CARTESIAN_POINT('Ctrl Pts',(3.62691566059552,-1.88779839617231,31.3337437960508));
#36454=CARTESIAN_POINT('Ctrl Pts',(3.54826816585965,2.03177090657653,31.5326767344143));
#36455=CARTESIAN_POINT('Ctrl Pts',(0.207681666353341,4.08352400741375,31.7316096727777));
#36456=CARTESIAN_POINT('Ctrl Pts',(-3.32382753019483,2.38127498268946,31.9305426111411));
#36457=CARTESIAN_POINT('Ctrl Pts',(-3.79972701545007,-1.51009092498523,
32.1294755495046));
#36458=CARTESIAN_POINT('Ctrl Pts',(-0.782520235955546,-4.01322340195306,
32.328408487868));
#36459=CARTESIAN_POINT('Ctrl Pts',(2.9540609426459,-2.82698141854484,32.5273414262314));
#36460=CARTESIAN_POINT('Ctrl Pts',(3.97496050958118,0.958117394129718,32.7262743645949));
#36461=CARTESIAN_POINT('Ctrl Pts',(1.34166086649601,3.86241454442386,32.9252073029583));
#36462=CARTESIAN_POINT('Ctrl Pts',(-2.52503369124243,3.21597650049785,33.1241402413218));
#36463=CARTESIAN_POINT('Ctrl Pts',(-4.07045333377795,-0.38692331436581,
33.3230731796852));
#36464=CARTESIAN_POINT('Ctrl Pts',(-1.87388678025847,-3.63412277288981,
33.5220061180486));
#36465=CARTESIAN_POINT('Ctrl Pts',(2.04535238235562,-3.54045669732818,33.720939056412));
#36466=CARTESIAN_POINT('Ctrl Pts',(4.08428983082642,-0.192032735416775,
33.9198719947756));
#36467=CARTESIAN_POINT('Ctrl Pts',(2.36852112880191,3.3329277904093,34.1188049331389));
#36468=CARTESIAN_POINT('Ctrl Pts',(-1.5246397804968,3.79391269448716,34.3177378715024));
#36469=CARTESIAN_POINT('Ctrl Pts',(-4.01619243028494,0.767136465425386,
34.5166708098658));
#36470=CARTESIAN_POINT('Ctrl Pts',(-2.81564117849665,-2.96487179277909,
34.7156037482293));
#36471=CARTESIAN_POINT('Ctrl Pts',(0.973341768490662,-3.97125997579838,
34.9145366865927));
#36472=CARTESIAN_POINT('Ctrl Pts',(3.8675272167539,-1.32685086627251,35.1134696249562));
#36473=CARTESIAN_POINT('Ctrl Pts',(3.20627736795542,2.53733825758359,35.3124025633196));
#36474=CARTESIAN_POINT('Ctrl Pts',(-0.402517795281907,4.06894082264232,
35.511335501683));
#36475=CARTESIAN_POINT('Ctrl Pts',(-3.64127652519993,1.85994764997906,35.7102684400464));
#36476=CARTESIAN_POINT('Ctrl Pts',(-3.53259324412043,-2.0589038261282,35.9092013784099));
#36477=CARTESIAN_POINT('Ctrl Pts',(-0.176380984849015,-4.08499568445078,
36.1081343167733));
#36478=CARTESIAN_POINT('Ctrl Pts',(3.34197911308852,-2.35573249778373,36.3070672551368));
#36479=CARTESIAN_POINT('Ctrl Pts',(3.78804266736189,1.53916624959495,36.5060001935002));
#36480=CARTESIAN_POINT('Ctrl Pts',(0.751741430954012,4.0191024888065,36.7049331318636));
#36481=CARTESIAN_POINT('Ctrl Pts',(-2.97563910948809,2.80425959604127,36.9038660702271));
#36482=CARTESIAN_POINT('Ctrl Pts',(-3.96750113199172,-0.988551850799671,
37.1027990085905));
#36483=CARTESIAN_POINT('Ctrl Pts',(-1.31202138353558,-3.87258310284293,
37.301731946954));
#36484=CARTESIAN_POINT('Ctrl Pts',(2.54960556749285,-3.19653115591342,37.5006648853174));
#36485=CARTESIAN_POINT('Ctrl Pts',(4.06736856819161,0.418106362963447,37.6995978236809));
#36486=CARTESIAN_POINT('Ctrl Pts',(1.84598120786055,3.64837681833342,37.8985307620442));
#36487=CARTESIAN_POINT('Ctrl Pts',(-2.07242503480969,3.52467791048579,38.0974637004078));
#36488=CARTESIAN_POINT('Ctrl Pts',(-4.0856415657996,0.160726665959935,38.2963966387711));
#36489=CARTESIAN_POINT('Ctrl Pts',(-2.34290926230782,-3.3509814065453,38.4953295771346));
#36490=CARTESIAN_POINT('Ctrl Pts',(1.5536700900277,-3.78211694123996,38.694262515498));
#36491=CARTESIAN_POINT('Ctrl Pts',(4.02195359031618,-0.736335510109945,
38.8931954538615));
#36492=CARTESIAN_POINT('Ctrl Pts',(2.79283673182646,2.98636302520864,39.0921283922249));
#36493=CARTESIAN_POINT('Ctrl Pts',(-1.00374721358184,3.96368347627922,39.2910613305884));
#36494=CARTESIAN_POINT('Ctrl Pts',(-3.87758251988644,1.29717370417073,39.4899942689517));
#36495=CARTESIAN_POINT('Ctrl Pts',(-3.18673725693753,-2.56183748892951,
39.6889272073153));
#36496=CARTESIAN_POINT('Ctrl Pts',(0.433687349425391,-4.06573266647945,
39.8878601456786));
#36497=CARTESIAN_POINT('Ctrl Pts',(3.65542630739156,-1.83199518874432,40.0867930840421));
#36498=CARTESIAN_POINT('Ctrl Pts',(3.51670552180105,2.08593024760723,40.2857260224055));
#36499=CARTESIAN_POINT('Ctrl Pts',(0.145080153377126,4.08619978216286,40.484658960769));
#36500=CARTESIAN_POINT('Ctrl Pts',(-3.35995399040756,2.33010469112103,40.6835918991324));
#36501=CARTESIAN_POINT('Ctrl Pts',(-3.77609830574217,-1.56825286709605,
40.8825248374958));
#36502=CARTESIAN_POINT('Ctrl Pts',(-0.720990444685169,-4.02455053491554,
41.0814577758593));
#36503=CARTESIAN_POINT('Ctrl Pts',(2.99718051531959,-2.78174701105068,41.2803907142227));
#36504=CARTESIAN_POINT('Ctrl Pts',(3.9595440561214,1.01964576599861,41.4793236525862));
#36505=CARTESIAN_POINT('Ctrl Pts',(1.28281295705702,3.88114366634645,41.6782565909495));
#36506=CARTESIAN_POINT('Ctrl Pts',(-2.57500755361336,3.17958857837247,41.8771895293131));
#36507=CARTESIAN_POINT('Ctrl Pts',(-4.0621147000577,-0.454817851921865,
42.0761224676764));
#36508=CARTESIAN_POINT('Ctrl Pts',(-2.56886110523792,-2.5838694518668,42.2087444265854));
#36509=CARTESIAN_POINT('Ctrl Pts',(-1.53687260224456,-3.09613266190232,
42.2750554060399));
#36510=CARTESIAN_POINT('Ctrl Pts',(-1.86645400133787,2.62012303844274,7.00322156819806));
#36511=CARTESIAN_POINT('Ctrl Pts',(-2.74041061257865,1.997626899089,7.0695770455426));
#36512=CARTESIAN_POINT('Ctrl Pts',(-3.80025934494349,-0.179501204411249,
7.20224350234162));
#36513=CARTESIAN_POINT('Ctrl Pts',(-1.89809237229961,-3.30104156426044,
7.40122093859512));
#36514=CARTESIAN_POINT('Ctrl Pts',(1.75033879183918,-3.37766291872948,7.60015387695855));
#36515=CARTESIAN_POINT('Ctrl Pts',(3.78874883692714,-0.353950369213094,
7.79908681532199));
#36516=CARTESIAN_POINT('Ctrl Pts',(2.34462897392162,2.99761246260044,7.99801975368543));
#36517=CARTESIAN_POINT('Ctrl Pts',(-1.25517146953415,3.59217513842517,8.19695269204886));
#36518=CARTESIAN_POINT('Ctrl Pts',(-3.70095537602795,0.885102952948687,
8.39588563041231));
#36519=CARTESIAN_POINT('Ctrl Pts',(-2.74450292932235,-2.63599675282763,
8.59481856877575));
#36520=CARTESIAN_POINT('Ctrl Pts',(0.735019325049069,-3.73363101754262,
8.79375150713918));
#36521=CARTESIAN_POINT('Ctrl Pts',(3.53881629779805,-1.39901612008267,8.99268444550262));
#36522=CARTESIAN_POINT('Ctrl Pts',(3.08937315587434,2.22177005300786,9.19161738386606));
#36523=CARTESIAN_POINT('Ctrl Pts',(-0.200149810864368,3.80004717549578,
9.3905503222295));
#36524=CARTESIAN_POINT('Ctrl Pts',(-3.30567149883918,1.88493714980744,9.58948326059294));
#36525=CARTESIAN_POINT('Ctrl Pts',(-3.37227577980602,-1.76301114979847,
9.78841619895636));
#36526=CARTESIAN_POINT('Ctrl Pts',(-0.338730933097911,-3.79021165389004,
9.98734913731983));
#36527=CARTESIAN_POINT('Ctrl Pts',(3.00621041944956,-2.33305531494441,10.1862820756832));
#36528=CARTESIAN_POINT('Ctrl Pts',(3.58752910607548,1.26889034228732,10.3852150140467));
#36529=CARTESIAN_POINT('Ctrl Pts',(0.870815925397089,3.70433883892876,10.5841479524101));
#36530=CARTESIAN_POINT('Ctrl Pts',(-2.64644222848811,2.73437212425091,10.7830808907735));
#36531=CARTESIAN_POINT('Ctrl Pts',(-3.73081407650405,-0.749315416829459,
10.9820138291369));
#36532=CARTESIAN_POINT('Ctrl Pts',(-1.38543162233216,-3.54415382593228,
11.1809467675004));
#36533=CARTESIAN_POINT('Ctrl Pts',(2.23358439312533,-3.08083559997405,11.3798797058638));
#36534=CARTESIAN_POINT('Ctrl Pts',(3.79925615786297,0.214708774655039,11.5788126442273));
#36535=CARTESIAN_POINT('Ctrl Pts',(1.87225451730644,3.31287038929909,11.7777455825907));
#36536=CARTESIAN_POINT('Ctrl Pts',(-1.77591918454253,3.36549524737367,11.9766785209541));
#36537=CARTESIAN_POINT('Ctrl Pts',(-3.79148233256386,0.32420507008613,12.1756114593176));
#36538=CARTESIAN_POINT('Ctrl Pts',(-2.32151858988368,-3.01512829587034,
12.374544397681));
#36539=CARTESIAN_POINT('Ctrl Pts',(1.28262771288672,-3.58264055637097,12.5734773360444));
#36540=CARTESIAN_POINT('Ctrl Pts',(3.70764854672028,-0.85661511733405,12.7724102744079));
#36541=CARTESIAN_POINT('Ctrl Pts',(2.72421126934337,2.65690048083118,12.9713432127713));
#36542=CARTESIAN_POINT('Ctrl Pts',(-0.763605773387818,3.72791542664558,
13.1702761511348));
#36543=CARTESIAN_POINT('Ctrl Pts',(-3.54943656817764,1.37184082667385,13.3692090894982));
#36544=CARTESIAN_POINT('Ctrl Pts',(-3.0722542406453,-2.24537326208117,13.5681420278616));
#36545=CARTESIAN_POINT('Ctrl Pts',(0.229265333024543,-3.79840553553036,
13.7670749662251));
#36546=CARTESIAN_POINT('Ctrl Pts',(3.32002024707132,-1.85954638670049,13.9660079045885));
#36547=CARTESIAN_POINT('Ctrl Pts',(3.35866550245346,1.78880218243472,14.164940842952));
#36548=CARTESIAN_POINT('Ctrl Pts',(0.309674340768458,3.79269679883976,14.3638737813154));
#36549=CARTESIAN_POINT('Ctrl Pts',(-3.02400184575466,2.30994806048298,14.5628067196789));
#36550=CARTESIAN_POINT('Ctrl Pts',(-3.57769943142826,-1.29634639800277,
14.7617396580423));
#36551=CARTESIAN_POINT('Ctrl Pts',(-0.842401716518874,-3.71090373807563,
14.9606725964057));
#36552=CARTESIAN_POINT('Ctrl Pts',(2.66731971394778,-2.71401045481454,15.1596055347691));
#36553=CARTESIAN_POINT('Ctrl Pts',(3.72496204373251,0.777884938798361,15.3585384731326));
#36554=CARTESIAN_POINT('Ctrl Pts',(1.35822988608424,3.55466718298702,15.557471411496));
#36555=CARTESIAN_POINT('Ctrl Pts',(-2.25712916101158,3.06362777696122,15.7564043498595));
#36556=CARTESIAN_POINT('Ctrl Pts',(-3.7974991416244,-0.243818528047306,
15.9553372882229));
#36557=CARTESIAN_POINT('Ctrl Pts',(-1.84681095199157,-3.32712135529518,
16.1542702265864));
#36558=CARTESIAN_POINT('Ctrl Pts',(1.80165891510899,-3.35178644290854,16.3532031649498));
#36559=CARTESIAN_POINT('Ctrl Pts',(3.79385557686611,-0.295139064068223,
16.5521361033133));
#36560=CARTESIAN_POINT('Ctrl Pts',(2.29834361397166,3.03283099386907,16.7510690416766));
#36561=CARTESIAN_POINT('Ctrl Pts',(-1.31004604878593,3.57270577508387,16.9500019800401));
#36562=CARTESIAN_POINT('Ctrl Pts',(-3.71410444208186,0.828175946623051,
17.1489349184035));
#36563=CARTESIAN_POINT('Ctrl Pts',(-2.70376979034626,-2.677699782662,17.347867856767));
#36564=CARTESIAN_POINT('Ctrl Pts',(0.792152682487336,-3.7219539670562,17.5468007951304));
#36565=CARTESIAN_POINT('Ctrl Pts',(3.55984560446539,-1.3445990025378,17.7457337334939));
#36566=CARTESIAN_POINT('Ctrl Pts',(3.05495632989659,2.26885191841203,17.9446666718573));
#36567=CARTESIAN_POINT('Ctrl Pts',(-0.25836814307153,3.79653698887591,18.1435996102207));
#36568=CARTESIAN_POINT('Ctrl Pts',(-3.33417361125188,1.83404840047608,18.3425325485842));
#36569=CARTESIAN_POINT('Ctrl Pts',(-3.34485816893761,-1.8144891939465,18.5414654869476));
#36570=CARTESIAN_POINT('Ctrl Pts',(-0.280599453828384,-3.79495864954658,
18.740398425311));
#36571=CARTESIAN_POINT('Ctrl Pts',(3.04161561079433,-2.28670542078106,18.9393313636745));
#36572=CARTESIAN_POINT('Ctrl Pts',(3.56765966054535,1.32372646410603,19.1382643020379));
#36573=CARTESIAN_POINT('Ctrl Pts',(0.813938016583792,3.71725061173132,19.3371972404014));
#36574=CARTESIAN_POINT('Ctrl Pts',(-2.68804053459405,2.69348942630865,19.5361301787648));
#36575=CARTESIAN_POINT('Ctrl Pts',(-3.71889124076811,-0.8064087949641,19.7350631171283));
#36576=CARTESIAN_POINT('Ctrl Pts',(-1.33094837618574,-3.56497175657617,
19.9339960554916));
#36577=CARTESIAN_POINT('Ctrl Pts',(2.28054136216125,-3.04624002677545,20.1329289938551));
#36578=CARTESIAN_POINT('Ctrl Pts',(3.79551909140992,0.272913964465135,20.3318619322185));
#36579=CARTESIAN_POINT('Ctrl Pts',(1.8212589195482,3.34117691139266,20.530794870582));
#36580=CARTESIAN_POINT('Ctrl Pts',(-1.8272928305604,3.33788078226886,20.7297278089454));
#36581=CARTESIAN_POINT('Ctrl Pts',(-3.79600600068437,0.266055723534535,
20.9286607473089));
#36582=CARTESIAN_POINT('Ctrl Pts',(-2.27503365179541,-3.05035556754547,
21.1275936856723));
#36583=CARTESIAN_POINT('Ctrl Pts',(1.33738744309295,-3.56256116190508,21.3265266240357));
#36584=CARTESIAN_POINT('Ctrl Pts',(3.72034220082859,-0.799688135457281,
21.5254595623992));
#36585=CARTESIAN_POINT('Ctrl Pts',(2.6831695136488,2.69834181791016,21.7243925007626));
#36586=CARTESIAN_POINT('Ctrl Pts',(-0.820653066905469,3.7157739098384,21.923325439126));
#36587=CARTESIAN_POINT('Ctrl Pts',(-3.57004556405178,1.31727820746093,22.1222583774895));
#36588=CARTESIAN_POINT('Ctrl Pts',(-3.03747899557971,-2.29219732062257,
22.3211913158529));
#36589=CARTESIAN_POINT('Ctrl Pts',(0.287455778651096,-3.79444546417224,
22.5201242542163));
#36590=CARTESIAN_POINT('Ctrl Pts',(3.34813115288769,-1.80844269699657,22.7190571925798));
#36591=CARTESIAN_POINT('Ctrl Pts',(3.33085438535164,1.84006963695426,22.9179901309432));
#36592=CARTESIAN_POINT('Ctrl Pts',(0.251508086732996,3.79699761490117,23.1169230693067));
#36593=CARTESIAN_POINT('Ctrl Pts',(-3.0590507357933,2.26332847839188,23.3158560076701));
#36594=CARTESIAN_POINT('Ctrl Pts',(-3.55741035402456,-1.35102878516191,
23.5147889460336));
#36595=CARTESIAN_POINT('Ctrl Pts',(-0.785426512475196,-3.72337916397971,
23.7137218843969));
#36596=CARTESIAN_POINT('Ctrl Pts',(2.70860348135616,-2.67281020389449,23.9126548227604));
#36597=CARTESIAN_POINT('Ctrl Pts',(3.71260202003901,0.83488528916224,24.1115877611238));
#36598=CARTESIAN_POINT('Ctrl Pts',(1.30358869708293,3.57506695239331,24.3105206994873));
#36599=CARTESIAN_POINT('Ctrl Pts',(-2.3038196226511,3.02867336494793,24.5094536378507));
#36600=CARTESIAN_POINT('Ctrl Pts',(-3.79331612292701,-0.301993372111428,
24.7083865762142));
#36601=CARTESIAN_POINT('Ctrl Pts',(-1.7955999210022,-3.35503623362761,24.9073195145776));
#36602=CARTESIAN_POINT('Ctrl Pts',(1.85281942552575,-3.32377908135478,25.1062524529411));
#36603=CARTESIAN_POINT('Ctrl Pts',(3.79793347763706,-0.23695675702724,25.3051853913045));
#36604=CARTESIAN_POINT('Ctrl Pts',(2.25159007243797,3.06770098786632,25.5041183296679));
#36605=CARTESIAN_POINT('Ctrl Pts',(-1.36465029001659,3.55220731253327,25.7030512680313));
#36606=CARTESIAN_POINT('Ctrl Pts',(-3.72636145659287,0.771153357041461,
25.9019842063948));
#36607=CARTESIAN_POINT('Ctrl Pts',(-2.66241164915182,-2.7188253742596,26.1009171447582));
#36608=CARTESIAN_POINT('Ctrl Pts',(0.849105252762015,-3.70937561794287,
26.2998500831217));
#36609=CARTESIAN_POINT('Ctrl Pts',(3.58003584787151,-1.28988004605551,26.4987830214851));
#36610=CARTESIAN_POINT('Ctrl Pts',(3.01982326417359,2.31540809759601,26.6977159598485));
#36611=CARTESIAN_POINT('Ctrl Pts',(-0.316526531389901,3.79213108425639,
26.896648898212));
#36612=CARTESIAN_POINT('Ctrl Pts',(-3.36189205222476,1.78273078013626,27.0955818365754));
#36613=CARTESIAN_POINT('Ctrl Pts',(-3.31665497416533,-1.86554200906911,
27.294514774939));
#36614=CARTESIAN_POINT('Ctrl Pts',(-0.222401948075185,-3.79881357515075,
27.4934477133024));
#36615=CARTESIAN_POINT('Ctrl Pts',(3.07630619675248,-2.23981860628926,27.6923806516658));
#36616=CARTESIAN_POINT('Ctrl Pts',(3.54695211382774,1.37825175765173,27.8913135900291));
#36617=CARTESIAN_POINT('Ctrl Pts',(0.756868878729541,3.72928903487889,28.0902465283926));
#36618=CARTESIAN_POINT('Ctrl Pts',(-2.72900734653197,2.65197400210329,28.2891794667561));
#36619=CARTESIAN_POINT('Ctrl Pts',(-3.70609475092345,-0.863312748912513,
28.4881124051195));
#36620=CARTESIAN_POINT('Ctrl Pts',(-1.27615245566332,-3.58495217752786,
28.6870453434829));
#36621=CARTESIAN_POINT('Ctrl Pts',(2.32696257530329,-3.01092882320308,28.8859782818464));
#36622=CARTESIAN_POINT('Ctrl Pts',(3.79089036556033,0.331055043095624,29.0849112202098));
#36623=CARTESIAN_POINT('Ctrl Pts',(1.7698354633568,3.36869850801491,29.2838441585732));
#36624=CARTESIAN_POINT('Ctrl Pts',(-1.87823720077816,3.3094821683868,29.4827770969367));
#36625=CARTESIAN_POINT('Ctrl Pts',(-3.79963789451971,0.207843873585611,
29.6817100353001));
#36626=CARTESIAN_POINT('Ctrl Pts',(-2.22801425278663,-3.08486623610115,
29.8806429736635));
#36627=CARTESIAN_POINT('Ctrl Pts',(1.39183298835648,-3.54164483507025,30.079575912027));
#36628=CARTESIAN_POINT('Ctrl Pts',(3.73216185585201,-0.742573287279,30.2785088503904));
#36629=CARTESIAN_POINT('Ctrl Pts',(2.64149741600532,2.73914924867091,30.4774417887539));
#36630=CARTESIAN_POINT('Ctrl Pts',(-0.877507569004345,3.70275946715383,
30.6763747271173));
#36631=CARTESIAN_POINT('Ctrl Pts',(-3.58981586917566,1.26240612746925,30.8753076654808));
#36632=CARTESIAN_POINT('Ctrl Pts',(-3.00199017263393,-2.33848288611794,
31.0742406038442));
#36633=CARTESIAN_POINT('Ctrl Pts',(0.345578693905692,-3.78959398505641,
31.2731735422076));
#36634=CARTESIAN_POINT('Ctrl Pts',(3.37545550105851,-1.75691416000643,31.4721064805712));
#36635=CARTESIAN_POINT('Ctrl Pts',(3.3022607693379,1.89090481424875,31.6710394189345));
#36636=CARTESIAN_POINT('Ctrl Pts',(0.193282747315501,3.80040642364043,31.8699723572979));
#36637=CARTESIAN_POINT('Ctrl Pts',(-3.09338098022485,2.216177185254,32.0689052956615));
#36638=CARTESIAN_POINT('Ctrl Pts',(-3.53628555418785,-1.40539378271698,
32.2678382340249));
#36639=CARTESIAN_POINT('Ctrl Pts',(-0.728266792592632,-3.73497987733052,
32.4667711723883));
#36640=CARTESIAN_POINT('Ctrl Pts',(2.74925093176247,-2.63098204468606,32.6657041107517));
#36641=CARTESIAN_POINT('Ctrl Pts',(3.69936981560612,0.891689504614469,32.8646370491151));
#36642=CARTESIAN_POINT('Ctrl Pts',(1.24864126331116,3.59462685140112,33.0635699874787));
#36643=CARTESIAN_POINT('Ctrl Pts',(-2.34996886088683,2.99300744371268,33.262502925842));
#36644=CARTESIAN_POINT('Ctrl Pts',(-3.78824196177939,-0.360097270568816,
33.4614358642054));
#36645=CARTESIAN_POINT('Ctrl Pts',(-1.74396705980911,-3.38216293214238,
33.660368802569));
#36646=CARTESIAN_POINT('Ctrl Pts',(1.90354466348184,-3.29499088305067,33.8593017409324));
#36647=CARTESIAN_POINT('Ctrl Pts',(3.80111915122855,-0.17871878306637,34.0582346792959));
#36648=CARTESIAN_POINT('Ctrl Pts',(2.20430757749551,3.10185030410124,34.2571676176593));
#36649=CARTESIAN_POINT('Ctrl Pts',(-1.41893394161954,3.5308743498711,34.4561005560226));
#36650=CARTESIAN_POINT('Ctrl Pts',(-3.73774305793726,0.713949604733199,
34.6550334943861));
#36651=CARTESIAN_POINT('Ctrl Pts',(-2.62042804254318,-2.75931224748304,
34.8539664327496));
#36652=CARTESIAN_POINT('Ctrl Pts',(0.90585834750904,-3.69592584605102,35.052899371113));
#36653=CARTESIAN_POINT('Ctrl Pts',(3.59938505356419,-1.23485806529853,35.2518323094765));
#36654=CARTESIAN_POINT('Ctrl Pts',(2.98398076833351,2.36142033095977,35.4507652478398));
#36655=CARTESIAN_POINT('Ctrl Pts',(-0.374610559908926,3.7868343155833,35.6496981862033));
#36656=CARTESIAN_POINT('Ctrl Pts',(-3.3888207027795,1.73099435286343,35.8486311245668));
#36657=CARTESIAN_POINT('Ctrl Pts',(-3.28767261627215,-1.91615656287791,
36.0475640629301));
#36658=CARTESIAN_POINT('Ctrl Pts',(-0.164152194675816,-3.80177606683461,
36.2464970012937));
#36659=CARTESIAN_POINT('Ctrl Pts',(3.11027408336399,-2.1924056037633,36.445429939657));
#36660=CARTESIAN_POINT('Ctrl Pts',(3.52541130159383,1.43245326619635,36.6443628780206));
#36661=CARTESIAN_POINT('Ctrl Pts',(0.699621933880535,3.74045135720976,36.843295816384));
#36662=CARTESIAN_POINT('Ctrl Pts',(-2.76933304802493,2.60983556433168,37.0422287547475));
#36663=CARTESIAN_POINT('Ctrl Pts',(-3.69242760920404,-0.920013889243654,
37.2411616931107));
#36664=CARTESIAN_POINT('Ctrl Pts',(-1.22105673552787,-3.60409040657181,
37.4400946314743));
#36665=CARTESIAN_POINT('Ctrl Pts',(2.37283712765188,-2.9749102775556,37.6390275698377));
#36666=CARTESIAN_POINT('Ctrl Pts',(3.7853710681766,0.389118345988962,37.8379605082012));
#36667=CARTESIAN_POINT('Ctrl Pts',(1.71799622765437,3.39542872065456,38.0368934465646));
#36668=CARTESIAN_POINT('Ctrl Pts',(-1.92874032343257,3.28030606602396,38.235826384928));
#36669=CARTESIAN_POINT('Ctrl Pts',(-3.80237716814379,0.149583216029986,
38.4347593232914));
#36670=CARTESIAN_POINT('Ctrl Pts',(-2.1804714247586,-3.1186522326827,38.633692261655));
#36671=CARTESIAN_POINT('Ctrl Pts',(1.44595153099118,-3.51989641602498,38.8326252000182));
#36672=CARTESIAN_POINT('Ctrl Pts',(3.74310478705912,-0.685284131425703,
39.0315581383817));
#36673=CARTESIAN_POINT('Ctrl Pts',(2.59920466649454,2.77931345664184,39.2304910767451));
#36674=CARTESIAN_POINT('Ctrl Pts',(-0.934155731980976,3.68887463797949,
39.4294240151087));
#36675=CARTESIAN_POINT('Ctrl Pts',(-3.60874320562774,1.20723847073212,39.628356953472));
#36676=CARTESIAN_POINT('Ctrl Pts',(-2.9657954060591,-2.38422098941366,39.8272898918356));
#36677=CARTESIAN_POINT('Ctrl Pts',(0.403619076468115,-3.78384858628005,
40.0262228301989));
#36678=CARTESIAN_POINT('Ctrl Pts',(3.40198945678621,-1.70497988275374,40.2251557685625));
#36679=CARTESIAN_POINT('Ctrl Pts',(3.27288641644818,1.9413091971248,40.4240887069258));
#36680=CARTESIAN_POINT('Ctrl Pts',(0.135021502466078,3.80289668242824,40.6230216452892));
#36681=CARTESIAN_POINT('Ctrl Pts',(-3.12700273222302,2.16855461601647,40.8219545836528));
#36682=CARTESIAN_POINT('Ctrl Pts',(-3.51429506264349,-1.45952325961196,
41.020887522016));
#36683=CARTESIAN_POINT('Ctrl Pts',(-0.671002965181634,-3.74552168112398,
41.2198204603797));
#36684=CARTESIAN_POINT('Ctrl Pts',(2.78938095197937,-2.58888381470178,41.418753398743));
#36685=CARTESIAN_POINT('Ctrl Pts',(3.68502221077952,0.948952011033468,41.6176863371064));
#36686=CARTESIAN_POINT('Ctrl Pts',(1.19387337835599,3.61205745181745,41.8166192754698));
#36687=CARTESIAN_POINT('Ctrl Pts',(-2.39647795137431,2.95914235739577,42.0155522138333));
#36688=CARTESIAN_POINT('Ctrl Pts',(-3.78048145955207,-0.423284565706465,
42.2144851521968));
#36689=CARTESIAN_POINT('Ctrl Pts',(-2.39075764659687,-2.40472543932513,
42.3471071111058));
#36690=CARTESIAN_POINT('Ctrl Pts',(-1.43031864127241,-2.88147257990253,
42.4134180905602));
#36691=CARTESIAN_POINT('Ctrl Pts',(-0.0207003078980803,-3.22266463217033,
35.));
#36692=CARTESIAN_POINT('Ctrl Pts',(0.390179082935768,-3.27339145921622,
35.));
#36693=CARTESIAN_POINT('Ctrl Pts',(0.778605604939595,-3.24434960842915,
35.));
#36694=CARTESIAN_POINT('Ctrl Pts',(1.56185674874276,-3.03916248926379,35.));
#36695=CARTESIAN_POINT('Ctrl Pts',(1.94872076465658,-2.8510360063766,35.));
#36696=CARTESIAN_POINT('Ctrl Pts',(2.68187385484571,-2.32275572829235,35.));
#36697=CARTESIAN_POINT('Ctrl Pts',(3.01817343547782,-1.96309141773522,35.));
#36698=CARTESIAN_POINT('Ctrl Pts',(3.49494789802835,-1.17980918440496,35.));
#36699=CARTESIAN_POINT('Ctrl Pts',(3.65560097307578,-0.759652858975631,
35.));
#36700=CARTESIAN_POINT('Ctrl Pts',(3.78646125695233,0.0823884449927741,
35.));
#36701=CARTESIAN_POINT('Ctrl Pts',(3.79123516462661,0.443182121773422,35.));
#36702=CARTESIAN_POINT('Ctrl Pts',(3.70863692495699,1.13742209958287,35.));
#36703=CARTESIAN_POINT('Ctrl Pts',(3.62486017046094,1.47282751573001,35.));
#36704=CARTESIAN_POINT('Ctrl Pts',(3.49931608640154,1.79133081339196,35.));
#36705=CARTESIAN_POINT('Ctrl Pts',(-3.8864130136037,0.610157723633211,38.));
#36706=CARTESIAN_POINT('Ctrl Pts',(-3.772631518137,1.05264935984635,38.));
#36707=CARTESIAN_POINT('Ctrl Pts',(-3.57839040445375,1.47494376323108,38.));
#36708=CARTESIAN_POINT('Ctrl Pts',(-3.03687080404268,2.26623247828738,38.));
#36709=CARTESIAN_POINT('Ctrl Pts',(-2.67423971095682,2.62879046566468,38.));
#36710=CARTESIAN_POINT('Ctrl Pts',(-1.89042756718785,3.13666861491962,38.));
#36711=CARTESIAN_POINT('Ctrl Pts',(-1.4826961685891,3.30719881404164,38.));
#36712=CARTESIAN_POINT('Ctrl Pts',(-0.560741755968393,3.47676848286895,
38.));
#36713=CARTESIAN_POINT('Ctrl Pts',(-0.0952693922769644,3.47380165091183,
38.));
#36714=CARTESIAN_POINT('Ctrl Pts',(0.654416143995199,3.32412025485652,38.));
#36715=CARTESIAN_POINT('Ctrl Pts',(0.949919393676216,3.22355758047029,38.));
#36716=CARTESIAN_POINT('Ctrl Pts',(1.41353731808283,2.98479081726645,38.));
#36717=CARTESIAN_POINT('Ctrl Pts',(1.66686279531448,2.83000589683937,38.));
#36718=CARTESIAN_POINT('Ctrl Pts',(1.92910760072171,2.58159390771144,38.));
#36719=CARTESIAN_POINT('Origin',(-9.5,-25.9558441227157,44.142135623731));
#36720=CARTESIAN_POINT('',(-9.5,-25.9558441227157,49.142135623731));
#36721=CARTESIAN_POINT('',(-10.,-25.9558441227157,49.642135623731));
#36722=CARTESIAN_POINT('Origin',(-9.5,-25.9558441227157,49.642135623731));
#36723=CARTESIAN_POINT('',(-10.,-22.0667568261897,48.031222920257));
#36724=CARTESIAN_POINT('Origin',(-10.,-25.9558441227157,44.142135623731));
#36725=CARTESIAN_POINT('',(-9.5,-22.420310216783,47.6776695296637));
#36726=CARTESIAN_POINT('Origin',(-9.5,-22.0667568261897,48.031222920257));
#36727=CARTESIAN_POINT('Origin',(-9.5,-25.9558441227157,44.142135623731));
#36728=CARTESIAN_POINT('Origin',(-9.5,-27.9350288425444,53.8994949366117));
#36729=CARTESIAN_POINT('',(-10.,-10.8535533905933,36.8180194846605));
#36730=CARTESIAN_POINT('',(-9.5,-11.2071067811866,36.4644660940673));
#36731=CARTESIAN_POINT('Origin',(-9.5,-10.8535533905933,36.8180194846605));
#36732=CARTESIAN_POINT('',(-9.5,-28.2885822331377,53.5459415460184));
#36733=CARTESIAN_POINT('',(-10.,-27.9350288425444,53.8994949366117));
#36734=CARTESIAN_POINT('Origin',(-9.5,-7.67157287525382,40.));
#36735=CARTESIAN_POINT('',(-10.,-7.67157287525382,35.5));
#36736=CARTESIAN_POINT('',(-9.5,-7.67157287525382,35.));
#36737=CARTESIAN_POINT('Origin',(-9.5,-7.67157287525382,35.5));
#36738=CARTESIAN_POINT('Origin',(-9.5,-7.67157287525382,40.));
#36739=CARTESIAN_POINT('Origin',(-10.,-7.67157287525382,40.));
#36740=CARTESIAN_POINT('Origin',(-9.5,-28.4068542494924,35.5));
#36741=CARTESIAN_POINT('',(-10.,0.499999999999998,35.5));
#36742=CARTESIAN_POINT('',(-9.5,0.499999999999998,35.));
#36743=CARTESIAN_POINT('Origin',(-9.5,0.499999999999998,35.5));
#36744=CARTESIAN_POINT('',(-9.5,-28.4068542494924,35.));
#36745=CARTESIAN_POINT('',(-10.,-28.4068542494924,35.5));
#36746=CARTESIAN_POINT('Origin',(-2.,0.499999999999998,35.5));
#36747=CARTESIAN_POINT('',(-2.,8.5,35.5));
#36748=CARTESIAN_POINT('',(-2.,8.,35.));
#36749=CARTESIAN_POINT('Origin',(-2.,8.,35.5));
#36750=CARTESIAN_POINT('Origin',(-2.,0.499999999999998,35.));
#36751=CARTESIAN_POINT('Origin',(-2.,0.499999999999998,35.5));
#36752=CARTESIAN_POINT('Origin',(0.,8.,35.5));
#36753=CARTESIAN_POINT('',(2.,8.5,35.5));
#36754=CARTESIAN_POINT('',(2.,8.,35.));
#36755=CARTESIAN_POINT('Origin',(2.,8.,35.5));
#36756=CARTESIAN_POINT('',(0.,8.,35.));
#36757=CARTESIAN_POINT('',(0.,8.5,35.5));
#36758=CARTESIAN_POINT('Origin',(2.,0.499999999999998,35.5));
#36759=CARTESIAN_POINT('',(10.,0.499999999999998,35.5));
#36760=CARTESIAN_POINT('',(9.5,0.499999999999998,35.));
#36761=CARTESIAN_POINT('Origin',(9.5,0.499999999999998,35.5));
#36762=CARTESIAN_POINT('Origin',(2.,0.499999999999998,35.));
#36763=CARTESIAN_POINT('Origin',(2.,0.499999999999998,35.5));
#36764=CARTESIAN_POINT('Origin',(9.5,-28.4068542494924,35.5));
#36765=CARTESIAN_POINT('',(10.,-7.67157287525382,35.5));
#36766=CARTESIAN_POINT('',(9.5,-7.67157287525382,35.));
#36767=CARTESIAN_POINT('Origin',(9.5,-7.67157287525382,35.5));
#36768=CARTESIAN_POINT('',(9.5,-28.4068542494924,35.));
#36769=CARTESIAN_POINT('',(10.,-28.4068542494924,35.5));
#36770=CARTESIAN_POINT('Origin',(9.5,-7.67157287525382,40.));
#36771=CARTESIAN_POINT('',(10.,-10.8535533905933,36.8180194846605));
#36772=CARTESIAN_POINT('',(9.5,-11.2071067811866,36.4644660940673));
#36773=CARTESIAN_POINT('Origin',(9.5,-10.8535533905933,36.8180194846605));
#36774=CARTESIAN_POINT('Origin',(9.5,-7.67157287525382,40.));
#36775=CARTESIAN_POINT('Origin',(10.,-7.67157287525382,40.));
#36776=CARTESIAN_POINT('Origin',(9.5,-27.9350288425444,53.8994949366117));
#36777=CARTESIAN_POINT('',(10.,-22.0667568261897,48.031222920257));
#36778=CARTESIAN_POINT('',(9.5,-22.420310216783,47.6776695296637));
#36779=CARTESIAN_POINT('Origin',(9.5,-22.0667568261897,48.031222920257));
#36780=CARTESIAN_POINT('',(9.5,-28.2885822331377,53.5459415460184));
#36781=CARTESIAN_POINT('',(10.,-27.9350288425444,53.8994949366117));
#36782=CARTESIAN_POINT('Origin',(9.5,-25.9558441227157,44.142135623731));
#36783=CARTESIAN_POINT('',(10.,-25.9558441227157,49.642135623731));
#36784=CARTESIAN_POINT('',(9.5,-25.9558441227157,49.142135623731));
#36785=CARTESIAN_POINT('Origin',(9.5,-25.9558441227157,49.642135623731));
#36786=CARTESIAN_POINT('Origin',(9.5,-25.9558441227157,44.142135623731));
#36787=CARTESIAN_POINT('Origin',(10.,-25.9558441227157,44.142135623731));
#36788=CARTESIAN_POINT('Origin',(9.5,-74.8566017177982,49.642135623731));
#36789=CARTESIAN_POINT('',(10.,-92.6421356237309,49.642135623731));
#36790=CARTESIAN_POINT('',(9.5,-92.6421356237309,49.142135623731));
#36791=CARTESIAN_POINT('Origin',(9.5,-92.6421356237309,49.642135623731));
#36792=CARTESIAN_POINT('',(9.5,-74.8566017177982,49.142135623731));
#36793=CARTESIAN_POINT('',(10.,-74.8566017177982,49.642135623731));
#36794=CARTESIAN_POINT('Origin',(0.,-92.6421356237309,49.642135623731));
#36795=CARTESIAN_POINT('',(-10.,-92.6421356237309,49.642135623731));
#36796=CARTESIAN_POINT('',(-9.5,-92.6421356237309,49.142135623731));
#36797=CARTESIAN_POINT('Origin',(-9.5,-92.6421356237309,49.642135623731));
#36798=CARTESIAN_POINT('Origin',(0.,-92.6421356237309,49.142135623731));
#36799=CARTESIAN_POINT('Origin',(0.,-92.6421356237309,49.642135623731));
#36800=CARTESIAN_POINT('Origin',(-9.5,-74.8566017177982,49.642135623731));
#36801=CARTESIAN_POINT('',(-10.,-74.8566017177982,49.642135623731));
#36802=CARTESIAN_POINT('',(-9.5,-74.8566017177982,49.142135623731));
#36803=CARTESIAN_POINT('Origin',(2.,0.499999999999998,39.2855339059327));
#36804=CARTESIAN_POINT('',(2.,8.5,37.5));
#36805=CARTESIAN_POINT('',(2.,8.5,39.2855339059327));
#36806=CARTESIAN_POINT('',(10.,0.499999999999998,37.5));
#36807=CARTESIAN_POINT('Origin',(2.,0.499999999999998,37.5));
#36808=CARTESIAN_POINT('',(10.,0.499999999999998,39.2855339059327));
#36809=CARTESIAN_POINT('Origin',(0.,8.5,35.));
#36810=CARTESIAN_POINT('',(-2.,8.5,37.5));
#36811=CARTESIAN_POINT('',(-2.,8.5,39.2855339059327));
#36812=CARTESIAN_POINT('',(0.,8.5,37.5));
#36813=CARTESIAN_POINT('Origin',(-2.,0.499999999999998,39.2855339059327));
#36814=CARTESIAN_POINT('',(-10.,0.499999999999998,37.5));
#36815=CARTESIAN_POINT('',(-10.,0.499999999999998,39.2855339059327));
#36816=CARTESIAN_POINT('Origin',(-2.,0.499999999999998,37.5));
#36817=CARTESIAN_POINT('Origin',(-10.,-47.0710678118655,43.5710678118655));
#36818=CARTESIAN_POINT('',(-10.,-92.6421356237309,51.642135623731));
#36819=CARTESIAN_POINT('',(-10.,-92.6421356237309,47.8566017177982));
#36820=CARTESIAN_POINT('',(-10.,-24.7132034355964,51.642135623731));
#36821=CARTESIAN_POINT('',(-10.,-34.8566017177982,51.642135623731));
#36822=CARTESIAN_POINT('',(-10.,-21.531222920257,50.3241161390704));
#36823=CARTESIAN_POINT('Origin',(-10.,-24.7132034355964,47.142135623731));
#36824=CARTESIAN_POINT('',(-10.,-10.3180194846605,39.110912703474));
#36825=CARTESIAN_POINT('',(-10.,-19.889087296526,48.6819805153395));
#36826=CARTESIAN_POINT('',(-10.,-6.42893218813451,37.5));
#36827=CARTESIAN_POINT('Origin',(-10.,-6.42893218813451,43.));
#36828=CARTESIAN_POINT('',(-10.,-19.2855339059327,37.5));
#36829=CARTESIAN_POINT('Origin',(0.,-102.642135623731,49.142135623731));
#36830=CARTESIAN_POINT('',(0.,-25.9558441227157,49.142135623731));
#36831=CARTESIAN_POINT('Origin',(0.,-7.67157287525382,40.));
#36832=CARTESIAN_POINT('',(0.,-11.2071067811866,36.4644660940673));
#36833=CARTESIAN_POINT('',(0.,-7.67157287525382,35.));
#36834=CARTESIAN_POINT('Origin',(0.,-23.8847763108502,49.142135623731));
#36835=CARTESIAN_POINT('',(0.,-22.420310216783,47.6776695296637));
#36836=CARTESIAN_POINT('Origin',(0.,-25.9558441227157,44.142135623731));
#36837=CARTESIAN_POINT('Origin',(9.5,-24.7132034355964,47.142135623731));
#36838=CARTESIAN_POINT('',(9.5,-24.7132034355964,52.142135623731));
#36839=CARTESIAN_POINT('',(10.,-24.7132034355964,51.642135623731));
#36840=CARTESIAN_POINT('Origin',(9.5,-24.7132034355964,51.642135623731));
#36841=CARTESIAN_POINT('',(10.,-21.531222920257,50.3241161390704));
#36842=CARTESIAN_POINT('Origin',(10.,-24.7132034355964,47.142135623731));
#36843=CARTESIAN_POINT('',(9.5,-21.1776695296637,50.6776695296637));
#36844=CARTESIAN_POINT('Origin',(9.5,-21.531222920257,50.3241161390704));
#36845=CARTESIAN_POINT('Origin',(9.5,-24.7132034355964,47.142135623731));
#36846=CARTESIAN_POINT('Origin',(9.5,-19.889087296526,48.6819805153395));
#36847=CARTESIAN_POINT('',(10.,-10.3180194846605,39.110912703474));
#36848=CARTESIAN_POINT('',(9.5,-9.96446609406726,39.4644660940673));
#36849=CARTESIAN_POINT('Origin',(9.5,-10.3180194846605,39.110912703474));
#36850=CARTESIAN_POINT('',(9.5,-19.5355339059327,49.0355339059327));
#36851=CARTESIAN_POINT('',(10.,-19.889087296526,48.6819805153395));
#36852=CARTESIAN_POINT('Origin',(9.5,-6.42893218813451,43.));
#36853=CARTESIAN_POINT('',(10.,-6.42893218813451,37.5));
#36854=CARTESIAN_POINT('',(9.5,-6.42893218813451,38.));
#36855=CARTESIAN_POINT('Origin',(9.5,-6.42893218813451,37.5));
#36856=CARTESIAN_POINT('Origin',(9.5,-6.42893218813451,43.));
#36857=CARTESIAN_POINT('Origin',(10.,-6.42893218813451,43.));
#36858=CARTESIAN_POINT('Origin',(9.5,-19.2855339059327,37.5));
#36859=CARTESIAN_POINT('',(9.5,0.499999999999998,38.));
#36860=CARTESIAN_POINT('Origin',(9.5,0.499999999999998,37.5));
#36861=CARTESIAN_POINT('',(9.5,-19.2855339059327,38.));
#36862=CARTESIAN_POINT('',(10.,-19.2855339059327,37.5));
#36863=CARTESIAN_POINT('Origin',(2.,0.499999999999998,37.5));
#36864=CARTESIAN_POINT('',(2.,8.,38.));
#36865=CARTESIAN_POINT('Origin',(2.,8.,37.5));
#36866=CARTESIAN_POINT('Origin',(2.,0.499999999999998,38.));
#36867=CARTESIAN_POINT('Origin',(0.,8.,37.5));
#36868=CARTESIAN_POINT('',(-2.,8.,38.));
#36869=CARTESIAN_POINT('Origin',(-2.,8.,37.5));
#36870=CARTESIAN_POINT('',(0.,8.,38.));
#36871=CARTESIAN_POINT('Origin',(-2.,0.499999999999998,37.5));
#36872=CARTESIAN_POINT('',(-9.5,0.499999999999998,38.));
#36873=CARTESIAN_POINT('Origin',(-9.5,0.499999999999998,37.5));
#36874=CARTESIAN_POINT('Origin',(-2.,0.499999999999998,38.));
#36875=CARTESIAN_POINT('Origin',(-9.5,-19.2855339059327,37.5));
#36876=CARTESIAN_POINT('',(-9.5,-6.42893218813451,38.));
#36877=CARTESIAN_POINT('Origin',(-9.5,-6.42893218813451,37.5));
#36878=CARTESIAN_POINT('',(-9.5,-19.2855339059327,38.));
#36879=CARTESIAN_POINT('Origin',(-9.5,-6.42893218813451,43.));
#36880=CARTESIAN_POINT('',(-9.5,-9.96446609406726,39.4644660940673));
#36881=CARTESIAN_POINT('Origin',(-9.5,-10.3180194846605,39.110912703474));
#36882=CARTESIAN_POINT('Origin',(-9.5,-6.42893218813451,43.));
#36883=CARTESIAN_POINT('Origin',(-9.5,-19.889087296526,48.6819805153395));
#36884=CARTESIAN_POINT('',(-9.5,-21.1776695296637,50.6776695296637));
#36885=CARTESIAN_POINT('Origin',(-9.5,-21.531222920257,50.3241161390704));
#36886=CARTESIAN_POINT('',(-9.5,-19.5355339059327,49.0355339059327));
#36887=CARTESIAN_POINT('Origin',(-9.5,-24.7132034355964,47.142135623731));
#36888=CARTESIAN_POINT('',(-9.5,-24.7132034355964,52.142135623731));
#36889=CARTESIAN_POINT('Origin',(-9.5,-24.7132034355964,51.642135623731));
#36890=CARTESIAN_POINT('Origin',(-9.5,-24.7132034355964,47.142135623731));
#36891=CARTESIAN_POINT('Origin',(-9.5,-34.8566017177982,51.642135623731));
#36892=CARTESIAN_POINT('',(-9.5,-92.6421356237309,52.142135623731));
#36893=CARTESIAN_POINT('Origin',(-9.5,-92.6421356237309,51.642135623731));
#36894=CARTESIAN_POINT('',(-9.5,-34.8566017177982,52.142135623731));
#36895=CARTESIAN_POINT('Origin',(0.,-92.6421356237309,51.642135623731));
#36896=CARTESIAN_POINT('',(10.,-92.6421356237309,51.642135623731));
#36897=CARTESIAN_POINT('',(9.5,-92.6421356237309,52.142135623731));
#36898=CARTESIAN_POINT('Origin',(9.5,-92.6421356237309,51.642135623731));
#36899=CARTESIAN_POINT('Origin',(0.,-92.6421356237309,52.142135623731));
#36900=CARTESIAN_POINT('Origin',(0.,-92.6421356237309,51.642135623731));
#36901=CARTESIAN_POINT('Origin',(9.5,-34.8566017177982,51.642135623731));
#36902=CARTESIAN_POINT('',(10.,-34.8566017177982,51.642135623731));
#36903=CARTESIAN_POINT('',(9.5,-34.8566017177982,52.142135623731));
#36904=CARTESIAN_POINT('Origin',(0.,-22.6421356237309,52.142135623731));
#36905=CARTESIAN_POINT('',(0.,-24.7132034355964,52.142135623731));
#36906=CARTESIAN_POINT('Origin',(0.,-6.42893218813451,43.));
#36907=CARTESIAN_POINT('',(0.,-9.96446609406726,39.4644660940673));
#36908=CARTESIAN_POINT('',(0.,-6.42893218813451,38.));
#36909=CARTESIAN_POINT('Origin',(0.,-8.5,38.));
#36910=CARTESIAN_POINT('',(0.,-21.1776695296637,50.6776695296637));
#36911=CARTESIAN_POINT('Origin',(0.,-24.7132034355964,47.142135623731));
#36912=CARTESIAN_POINT('Origin',(10.,-47.0710678118655,43.5710678118655));
#36913=CARTESIAN_POINT('',(10.,-92.6421356237309,47.8566017177982));
#36914=CARTESIAN_POINT('Origin',(0.,-92.6421356237309,47.8566017177982));
#36915=CARTESIAN_POINT('Origin',(0.,-9.74264068711929,35.));
#36916=CARTESIAN_POINT('Origin',(0.,8.5,38.));
#36917=CARTESIAN_POINT('',(0.,0.,0.));
#36918=CARTESIAN_POINT('Origin',(0.,-13.3748739960349,0.));
#36919=CARTESIAN_POINT('',(7.41225940988737,-39.6876842086708,-9.65703625032018));
#36920=CARTESIAN_POINT('',(7.4120723883382,-39.9374428050303,-9.6567920162102));
#36921=CARTESIAN_POINT('',(7.41272179941101,-13.3748739960349,-9.65763976210217));
#36922=CARTESIAN_POINT('',(8.61094305413662,-40.,-8.60639936142963));
#36923=CARTESIAN_POINT('Ctrl Pts',(7.4120723883382,-39.9374428050303,-9.6567920162102));
#36924=CARTESIAN_POINT('Ctrl Pts',(7.83414093874789,-39.9582952033535,-9.33338243380816));
#36925=CARTESIAN_POINT('Ctrl Pts',(8.23507438987139,-39.9791476016768,-8.98246646311764));
#36926=CARTESIAN_POINT('Ctrl Pts',(8.61094305413662,-40.,-8.60639936142963));
#36927=CARTESIAN_POINT('',(11.7598063682261,-40.,-3.15424737243508));
#36928=CARTESIAN_POINT('Origin',(0.,-40.,0.));
#36929=CARTESIAN_POINT('Ctrl Pts',(7.41225940988737,-39.6876842086708,-9.65703625032018));
#36930=CARTESIAN_POINT('Ctrl Pts',(8.0009299948616,-39.7167676583016,-9.20584367320952));
#36931=CARTESIAN_POINT('Ctrl Pts',(9.96140840545013,-39.820872922078,-7.4001799654877));
#36932=CARTESIAN_POINT('Ctrl Pts',(11.263434788298,-39.9249781858544,-5.00116413859683));
#36933=CARTESIAN_POINT('Ctrl Pts',(11.7598063682261,-40.,-3.15424737243508));
#36934=CARTESIAN_POINT('Origin',(0.,-13.3748739960349,0.));
#36935=CARTESIAN_POINT('',(7.41272179941099,-36.6876961535581,-9.65763976210219));
#36936=CARTESIAN_POINT('',(7.41272179941099,-36.9374484774433,-9.65763976210219));
#36937=CARTESIAN_POINT('',(7.41272179941101,-13.3748739960349,-9.65763976210217));
#36938=CARTESIAN_POINT('',(-12.1744916248676,-38.8748739948544,0.000309104184771874));
#36939=CARTESIAN_POINT('Ctrl Pts',(7.41272179941099,-36.9374484774433,-9.65763976210219));
#36940=CARTESIAN_POINT('Ctrl Pts',(7.63813777186494,-36.9485938361832,-9.48462172310865));
#36941=CARTESIAN_POINT('Ctrl Pts',(7.85751736927417,-36.959739194923,-9.3036899163584));
#36942=CARTESIAN_POINT('Ctrl Pts',(8.07031067017878,-36.9708845536629,-9.11529132484523));
#36943=CARTESIAN_POINT('Ctrl Pts',(8.28308082857198,-36.98202870028,-8.92691322277667));
#36944=CARTESIAN_POINT('Ctrl Pts',(8.48926592113985,-36.9931728468971,-8.73107013428625));
#36945=CARTESIAN_POINT('Ctrl Pts',(8.68835034828689,-37.0043169935143,-8.5282482653487));
#36946=CARTESIAN_POINT('Ctrl Pts',(8.89179157179527,-37.0157050204697,-8.3209878092587));
#36947=CARTESIAN_POINT('Ctrl Pts',(9.08781759960384,-37.027093047425,-8.10643984428187));
#36948=CARTESIAN_POINT('Ctrl Pts',(9.27591824460373,-37.0384810743804,-7.88516271039651));
#36949=CARTESIAN_POINT('Ctrl Pts',(9.46000106079451,-37.0496258531386,-7.66861205495211));
#36950=CARTESIAN_POINT('Ctrl Pts',(9.63649341936148,-37.0607706318969,-7.44561696503954));
#36951=CARTESIAN_POINT('Ctrl Pts',(9.80495738553523,-37.0719154106551,-7.21673478228473));
#36952=CARTESIAN_POINT('Ctrl Pts',(9.9789367446495,-37.083425061709,-6.98035915625153));
#36953=CARTESIAN_POINT('Ctrl Pts',(10.1443529947712,-37.094934712763,-6.73770471196109));
#36954=CARTESIAN_POINT('Ctrl Pts',(10.3007711278883,-37.106444363817,-6.48941942093926));
#36955=CARTESIAN_POINT('Ctrl Pts',(10.4571892610053,-37.1179540148709,-6.24113412991742));
#36956=CARTESIAN_POINT('Ctrl Pts',(10.6046091172304,-37.1294636659249,-5.98721826140925));
#36957=CARTESIAN_POINT('Ctrl Pts',(10.742646351938,-37.1409733169788,-5.72835051364639));
#36958=CARTESIAN_POINT('Ctrl Pts',(10.8763379661845,-37.1521206268483,-5.47763231324153));
#36959=CARTESIAN_POINT('Ctrl Pts',(11.0012686005856,-37.1632679367179,-5.22219436487314));
#36960=CARTESIAN_POINT('Ctrl Pts',(11.1171200677777,-37.1744152465874,-4.9626698105571));
#36961=CARTESIAN_POINT('Ctrl Pts',(11.2329518581578,-37.1855606631402,-4.70318933523264));
#36962=CARTESIAN_POINT('Ctrl Pts',(11.3397074513444,-37.196706079693,-4.43962388319863));
#36963=CARTESIAN_POINT('Ctrl Pts',(11.4371160292913,-37.2078514962458,-4.17262833026484));
#36964=CARTESIAN_POINT('Ctrl Pts',(11.5345137937413,-37.2189956755263,-3.90566241697496));
#36965=CARTESIAN_POINT('Ctrl Pts',(11.6225665235307,-37.2301398548069,-3.63526741367178));
#36966=CARTESIAN_POINT('Ctrl Pts',(11.7010522555776,-37.2412840340875,-3.3621163516812));
#36967=CARTESIAN_POINT('Ctrl Pts',(11.782009616388,-37.2527791596272,-3.08036336926517));
#36968=CARTESIAN_POINT('Ctrl Pts',(11.8527875672035,-37.2642742851669,-2.79567821335521));
#36969=CARTESIAN_POINT('Ctrl Pts',(11.9131983041429,-37.2757694107066,-2.50881573977965));
#36970=CARTESIAN_POINT('Ctrl Pts',(11.971767831112,-37.2869141856162,-2.23069631542371));
#36971=CARTESIAN_POINT('Ctrl Pts',(12.0205926768578,-37.2980589605257,-1.95053060259384));
#36972=CARTESIAN_POINT('Ctrl Pts',(12.0595535357516,-37.3092037354353,-1.6690173061836));
#36973=CARTESIAN_POINT('Ctrl Pts',(12.1003515732662,-37.3208740362901,-1.37422939970866));
#36974=CARTESIAN_POINT('Ctrl Pts',(12.1303329348627,-37.3325443371448,-1.07796407739402));
#36975=CARTESIAN_POINT('Ctrl Pts',(12.1494213968046,-37.3442146379996,-0.781031352038081));
#36976=CARTESIAN_POINT('Ctrl Pts',(12.1685098587465,-37.3558849388544,-0.484098626682174));
#36977=CARTESIAN_POINT('Ctrl Pts',(12.1767054082705,-37.3675552397091,-0.186498833656002));
#36978=CARTESIAN_POINT('Ctrl Pts',(12.1739943825377,-37.3792255405639,0.110955053691345));
#36979=CARTESIAN_POINT('Ctrl Pts',(12.1714048572777,-37.3903728116839,0.395077902726157));
#36980=CARTESIAN_POINT('Ctrl Pts',(12.1588640971083,-37.4015200828038,0.679152499465869));
#36981=CARTESIAN_POINT('Ctrl Pts',(12.1363956968827,-37.4126673539238,0.962470643026071));
#36982=CARTESIAN_POINT('Ctrl Pts',(12.1139311132748,-37.4238127315012,1.24574066046157));
#36983=CARTESIAN_POINT('Ctrl Pts',(12.0815422775253,-37.4349581090787,1.52825421544422));
#36984=CARTESIAN_POINT('Ctrl Pts',(12.0393047783483,-37.4461034866561,1.80930669153689));
#36985=CARTESIAN_POINT('Ctrl Pts',(11.9970719685101,-37.4572476268389,2.09032796430773));
#36986=CARTESIAN_POINT('Ctrl Pts',(11.9449927182814,-37.4683917670218,2.36988821838241));
#36987=CARTESIAN_POINT('Ctrl Pts',(11.8831942023772,-37.4795359072047,2.64729027471258));
#36988=CARTESIAN_POINT('Ctrl Pts',(11.8194491765883,-37.49103106195,2.93342985227278));
#36989=CARTESIAN_POINT('Ctrl Pts',(11.7453627483409,-37.5025262166954,3.21727278043161));
#36990=CARTESIAN_POINT('Ctrl Pts',(11.6611312464288,-37.5140213714408,3.49806636637472));
#36991=CARTESIAN_POINT('Ctrl Pts',(11.5794674609318,-37.525166107437,3.77030022960688));
#36992=CARTESIAN_POINT('Ctrl Pts',(11.4882680468647,-37.5363108434333,4.0396676423719));
#36993=CARTESIAN_POINT('Ctrl Pts',(11.387762605013,-37.5474555794296,4.30549800857771));
#36994=CARTESIAN_POINT('Ctrl Pts',(11.282516944386,-37.5591259435495,4.58386594558306));
#36995=CARTESIAN_POINT('Ctrl Pts',(11.1670664275532,-37.5707963076694,4.85835486815289));
#36996=CARTESIAN_POINT('Ctrl Pts',(11.0417317581506,-37.5824666717893,5.12821704211602));
#36997=CARTESIAN_POINT('Ctrl Pts',(10.916397088748,-37.5941370359092,5.39807921607914));
#36998=CARTESIAN_POINT('Ctrl Pts',(10.7811784160682,-37.6058074000291,5.66331434083362));
#36999=CARTESIAN_POINT('Ctrl Pts',(10.6364527948914,-37.617477764149,5.92320202188377));
#37000=CARTESIAN_POINT('Ctrl Pts',(10.4982123241924,-37.6286251796242,6.171444144219));
#37001=CARTESIAN_POINT('Ctrl Pts',(10.3512569086563,-37.6397725950994,6.41488166047602));
#37002=CARTESIAN_POINT('Ctrl Pts',(10.1959461834747,-37.6509200105746,6.65290400304169));
#37003=CARTESIAN_POINT('Ctrl Pts',(10.0406618319041,-37.6620655330859,6.89088592657842));
#37004=CARTESIAN_POINT('Ctrl Pts',(9.87702514909113,-37.6732110555971,7.12345428902473));
#37005=CARTESIAN_POINT('Ctrl Pts',(9.70543970866531,-37.6843565781084,7.35002655175222));
#37006=CARTESIAN_POINT('Ctrl Pts',(9.53387331491804,-37.6955008634215,7.57657366404126));
#37007=CARTESIAN_POINT('Ctrl Pts',(9.35436008645349,-37.7066451487347,7.79712579310562));
#37008=CARTESIAN_POINT('Ctrl Pts',(9.16734533347103,-37.7177894340478,8.0111316171242));
#37009=CARTESIAN_POINT('Ctrl Pts',(8.97444438432209,-37.7292844801883,8.23187316782131));
#37010=CARTESIAN_POINT('Ctrl Pts',(8.77356223729388,-37.7407795263289,8.44564942636426));
#37011=CARTESIAN_POINT('Ctrl Pts',(8.56523145482445,-37.7522745724694,8.65189345607572));
#37012=CARTESIAN_POINT('Ctrl Pts',(8.36324692134804,-37.7634194522824,8.85185480422493));
#37013=CARTESIAN_POINT('Ctrl Pts',(8.15426104066128,-37.7745643320955,9.04473583466629));
#37014=CARTESIAN_POINT('Ctrl Pts',(7.93879633762431,-37.7857092119086,9.23005758160386));
#37015=CARTESIAN_POINT('Ctrl Pts',(7.71317695122263,-37.7973793412128,9.42411339790046));
#37016=CARTESIAN_POINT('Ctrl Pts',(7.48045361358976,-37.8090494705171,9.60988006186248));
#37017=CARTESIAN_POINT('Ctrl Pts',(7.24126569578255,-37.8207195998213,9.78685451884735));
#37018=CARTESIAN_POINT('Ctrl Pts',(7.00207777797537,-37.8323897291256,9.96382897583221));
#37019=CARTESIAN_POINT('Ctrl Pts',(6.75642555486916,-37.8440598584298,10.1320110333703));
#37020=CARTESIAN_POINT('Ctrl Pts',(6.50498479025111,-37.8557299877341,10.2909486019804));
#37021=CARTESIAN_POINT('Ctrl Pts',(6.26481384489021,-37.8668770505095,10.4427624344129));
#37022=CARTESIAN_POINT('Ctrl Pts',(6.01929011209589,-37.8780241132849,10.5861875973639));
#37023=CARTESIAN_POINT('Ctrl Pts',(5.76902151508655,-37.8891711760602,10.7208600871604));
#37024=CARTESIAN_POINT('Ctrl Pts',(5.51879544336716,-37.9003163447423,10.8555096935958));
#37025=CARTESIAN_POINT('Ctrl Pts',(5.26382635192,-37.9114615134244,10.9814094697884));
#37026=CARTESIAN_POINT('Ctrl Pts',(5.0047473324093,-37.9226066821064,11.0982410493169));
#37027=CARTESIAN_POINT('Ctrl Pts',(4.74569707726916,-37.9337506133909,11.215059657564));
#37028=CARTESIAN_POINT('Ctrl Pts',(4.48253804836199,-37.9448945446753,11.3228119699299));
#37029=CARTESIAN_POINT('Ctrl Pts',(4.21592504663252,-37.9560384759598,11.4212270028739));
#37030=CARTESIAN_POINT('Ctrl Pts',(3.94090545364192,-37.9675337872397,11.5227451663875));
#37031=CARTESIAN_POINT('Ctrl Pts',(3.66221081418894,-37.9790290985197,11.6143275567594));
#37032=CARTESIAN_POINT('Ctrl Pts',(3.38058013274304,-37.9905244097996,11.6957311962999));
#37033=CARTESIAN_POINT('Ctrl Pts',(3.10754346510028,-38.0016689394698,11.774650788299));
#37034=CARTESIAN_POINT('Ctrl Pts',(2.83174755468966,-38.0128134691399,11.8440035547903));
#37035=CARTESIAN_POINT('Ctrl Pts',(2.55388037739943,-38.02395799881,11.9036189987724));
#37036=CARTESIAN_POINT('Ctrl Pts',(2.26289411406654,-38.0356287008949,11.9660490973915));
#37037=CARTESIAN_POINT('Ctrl Pts',(1.96963659936645,-38.0472994029797,12.0178001895381));
#37038=CARTESIAN_POINT('Ctrl Pts',(1.67491012193627,-38.0589701050646,12.0587365148027));
#37039=CARTESIAN_POINT('Ctrl Pts',(1.38018364450609,-38.0706408071495,12.0996728400673));
#37040=CARTESIAN_POINT('Ctrl Pts',(1.08398853798748,-38.0823115092343,12.1297943609895));
#37041=CARTESIAN_POINT('Ctrl Pts',(0.787134657080782,-38.0939822113192,
12.1490275035339));
#37042=CARTESIAN_POINT('Ctrl Pts',(0.503583140229768,-38.1051299358117,
12.1673987868252));
#37043=CARTESIAN_POINT('Ctrl Pts',(0.219345890921422,-38.1162776603042,
12.1758415742294));
#37044=CARTESIAN_POINT('Ctrl Pts',(-0.0648690228389137,-38.1274253847967,
12.1743271789399));
#37045=CARTESIAN_POINT('Ctrl Pts',(-0.349035688152791,-38.1385712168467,
12.1728130407349));
#37046=CARTESIAN_POINT('Ctrl Pts',(-0.633179758886583,-38.1497170488967,
12.1613450960154));
#37047=CARTESIAN_POINT('Ctrl Pts',(-0.916592908336909,-38.1608628809466,
12.1399467746109));
#37048=CARTESIAN_POINT('Ctrl Pts',(-1.19997459133722,-38.1720074755108,
12.1185508289933));
#37049=CARTESIAN_POINT('Ctrl Pts',(-1.48262524921969,-38.1831520700749,
12.0872267283601));
#37050=CARTESIAN_POINT('Ctrl Pts',(-1.76384016867791,-38.194296664639,12.0460498965162));
#37051=CARTESIAN_POINT('Ctrl Pts',(-2.05389228566501,-38.2057914788278,
12.0035790799957));
#37052=CARTESIAN_POINT('Ctrl Pts',(-2.34241667380791,-38.2172862930165,
11.9506263064734));
#37053=CARTESIAN_POINT('Ctrl Pts',(-2.62864831310905,-38.2287811072053,
11.8873318409132));
#37054=CARTESIAN_POINT('Ctrl Pts',(-2.90617384669823,-38.2399262917455,
11.8259625584302));
#37055=CARTESIAN_POINT('Ctrl Pts',(-3.18154377189134,-38.2510714762857,
11.7548714598031));
#37056=CARTESIAN_POINT('Ctrl Pts',(-3.45407233157046,-38.2622166608259,
11.6742380727086));
#37057=CARTESIAN_POINT('Ctrl Pts',(-3.73942491370659,-38.2738862898389,
11.5898104250489));
#37058=CARTESIAN_POINT('Ctrl Pts',(-4.02166199993082,-38.285555918852,11.4949209773659));
#37059=CARTESIAN_POINT('Ctrl Pts',(-4.30001441364412,-38.2972255478651,
11.3898343399916));
#37060=CARTESIAN_POINT('Ctrl Pts',(-4.57836682735739,-38.3088951768782,
11.2847477026174));
#37061=CARTESIAN_POINT('Ctrl Pts',(-4.85283425796642,-38.3205648058912,
11.1694640021579));
#37062=CARTESIAN_POINT('Ctrl Pts',(-5.12267062571763,-38.3322344349043,
11.0443060402367));
#37063=CARTESIAN_POINT('Ctrl Pts',(-5.38041794246529,-38.343381248029,10.9247553320664));
#37064=CARTESIAN_POINT('Ctrl Pts',(-5.63401694334377,-38.3545280611537,
10.796160008172));
#37065=CARTESIAN_POINT('Ctrl Pts',(-5.88283226064311,-38.3656748742783,
10.6588336530381));
#37066=CARTESIAN_POINT('Ctrl Pts',(-6.1316053072015,-38.376819793693,10.5215306280063));
#37067=CARTESIAN_POINT('Ctrl Pts',(-6.37559605922401,-38.3879647131077,
10.3754996620031));
#37068=CARTESIAN_POINT('Ctrl Pts',(-6.61419386041611,-38.3991096325224,
10.2211002258482));
#37069=CARTESIAN_POINT('Ctrl Pts',(-6.85276519254124,-38.4102533155651,
10.066717918137));
#37070=CARTESIAN_POINT('Ctrl Pts',(-7.08594454455926,-38.4213969986079,
9.90396913897554));
#37071=CARTESIAN_POINT('Ctrl Pts',(-7.31314931363975,-38.4325406816507,
9.7332572845071));
#37072=CARTESIAN_POINT('Ctrl Pts',(-7.54752711982908,-38.4440361797206,
9.55715591963368));
#37073=CARTESIAN_POINT('Ctrl Pts',(-7.77554672721654,-38.4555316777905,
9.37258068116194));
#37074=CARTESIAN_POINT('Ctrl Pts',(-7.99660336458607,-38.4670271758604,
9.18002096291129));
#37075=CARTESIAN_POINT('Ctrl Pts',(-8.21090626771047,-38.4781714628565,
8.99334433950392));
#37076=CARTESIAN_POINT('Ctrl Pts',(-8.41866514053532,-38.4893157498526,
8.79916406173953));
#37077=CARTESIAN_POINT('Ctrl Pts',(-8.61936384853658,-38.5004600368487,
8.59796586970085));
#37078=CARTESIAN_POINT('Ctrl Pts',(-8.82955005566236,-38.5121311404555,
8.38725656675452));
#37079=CARTESIAN_POINT('Ctrl Pts',(-9.03199227177261,-38.5238022440623,
8.16885006407581));
#37080=CARTESIAN_POINT('Ctrl Pts',(-9.22614151152845,-38.535473347669,7.94334709421989));
#37081=CARTESIAN_POINT('Ctrl Pts',(-9.42029075128428,-38.5471444512758,
7.71784412436397));
#37082=CARTESIAN_POINT('Ctrl Pts',(-9.60614680231032,-38.5588155548826,
7.4852449475224));
#37083=CARTESIAN_POINT('Ctrl Pts',(-9.78320885115772,-38.5704866584894,
7.24619036629795));
#37084=CARTESIAN_POINT('Ctrl Pts',(-9.95232519265855,-38.5816340181642,
7.01786342408272));
#37085=CARTESIAN_POINT('Ctrl Pts',(-10.1134700589456,-38.592781377839,6.78357934184873));
#37086=CARTESIAN_POINT('Ctrl Pts',(-10.2662355845482,-38.6039287375138,
6.54391757073364));
#37087=CARTESIAN_POINT('Ctrl Pts',(-10.4189751284731,-38.6150742012955,
6.30429656022115));
#37088=CARTESIAN_POINT('Ctrl Pts',(-10.5633380336435,-38.6262196650772,
6.05929991170006));
#37089=CARTESIAN_POINT('Ctrl Pts',(-10.6989600913802,-38.6373651288589,
5.80953554193913));
#37090=CARTESIAN_POINT('Ctrl Pts',(-10.8345670610239,-38.6485093526963,
5.55979895872045));
#37091=CARTESIAN_POINT('Ctrl Pts',(-10.9614349977632,-38.6596535765337,
5.30529594776737));
#37092=CARTESIAN_POINT('Ctrl Pts',(-11.0792453455692,-38.6707978003711,
5.04665957071439));
#37093=CARTESIAN_POINT('Ctrl Pts',(-11.20076485087,-38.682292890513,4.77988024973298));
#37094=CARTESIAN_POINT('Ctrl Pts',(-11.3126470548315,-38.693787980655,4.50870334116523));
#37095=CARTESIAN_POINT('Ctrl Pts',(-11.4145951579047,-38.7052830707969,
4.23384785167571));
#37096=CARTESIAN_POINT('Ctrl Pts',(-11.5134367040608,-38.7164278831925,
3.96736774334894));
#37097=CARTESIAN_POINT('Ctrl Pts',(-11.6029405119847,-38.7275726955881,
3.69743018378309));
#37098=CARTESIAN_POINT('Ctrl Pts',(-11.6828857891978,-38.7387175079836,
3.42470873017855));
#37099=CARTESIAN_POINT('Ctrl Pts',(-11.7666000466156,-38.7503877369988,
3.13912995972093));
#37100=CARTESIAN_POINT('Ctrl Pts',(-11.8398327384508,-38.7620579660139,
2.85049879505899));
#37101=CARTESIAN_POINT('Ctrl Pts',(-11.9023893162427,-38.7737281950291,
2.55960520678335));
#37102=CARTESIAN_POINT('Ctrl Pts',(-11.9649458940345,-38.7853984240442,
2.26871161850769));
#37103=CARTESIAN_POINT('Ctrl Pts',(-12.0168262958164,-38.7970686530593,
1.97555593644156));
#37104=CARTESIAN_POINT('Ctrl Pts',(-12.0578974154622,-38.8087388820745,
1.68094026312326));
#37105=CARTESIAN_POINT('Ctrl Pts',(-12.0989059319874,-38.8203913226104,
1.38677366109214));
#37106=CARTESIAN_POINT('Ctrl Pts',(-12.1291472088389,-38.8320437631464,
1.0910923577));
#37107=CARTESIAN_POINT('Ctrl Pts',(-12.1485371754145,-38.8436962036824,
0.794666437929197));
#37108=CARTESIAN_POINT('Ctrl Pts',(-12.1658307293892,-38.8540888007279,
0.530289621029534));
#37109=CARTESIAN_POINT('Ctrl Pts',(-12.1744932675459,-38.8644813977734,
0.265320699870421));
#37110=CARTESIAN_POINT('Ctrl Pts',(-12.174499996076,-38.8748739948188,0.000309105303522327));
#37111=CARTESIAN_POINT('Ctrl Pts',(-12.1742135449704,-38.8748739960349,
0.000309067021438125));
#37112=CARTESIAN_POINT('Ctrl Pts',(-12.1728218038936,-38.9322463659098,
-1.46265402061263));
#37113=CARTESIAN_POINT('Ctrl Pts',(-11.5435367915227,-39.0690361436464,
-4.95189231269601));
#37114=CARTESIAN_POINT('Ctrl Pts',(-8.28522524716096,-39.2852433292447,
-9.61375508410346));
#37115=CARTESIAN_POINT('Ctrl Pts',(-2.67484068581488,-39.5234955528298,
-12.4063460053113));
#37116=CARTESIAN_POINT('Ctrl Pts',(3.04101717371279,-39.7408953780917,-12.1939464673343));
#37117=CARTESIAN_POINT('Ctrl Pts',(6.22667163503174,-39.8788777954918,-10.5651040954537));
#37118=CARTESIAN_POINT('Ctrl Pts',(7.4120723883382,-39.9374428050303,-9.6567920162102));
#37119=CARTESIAN_POINT('',(-12.1744999965607,-38.6251260039651,0.00028938649696687));
#37120=CARTESIAN_POINT('Ctrl Pts',(-12.1748649577908,-38.6251260151384,
0.000289110302658423));
#37121=CARTESIAN_POINT('Ctrl Pts',(-12.1731836483798,-38.6907258978333,
-1.67221371080106));
#37122=CARTESIAN_POINT('Ctrl Pts',(-11.4051697641933,-38.8357431883897,
-5.37100026957135));
#37123=CARTESIAN_POINT('Ctrl Pts',(-7.77755196994913,-39.060177886808,-10.0290176561892));
#37124=CARTESIAN_POINT('Ctrl Pts',(-2.02988957584845,-39.2984301103931,
-12.5280053565324));
#37125=CARTESIAN_POINT('Ctrl Pts',(3.45078694475986,-39.5075988843473,-12.0396942716201));
#37126=CARTESIAN_POINT('Ctrl Pts',(6.39346277427829,-39.6373502504399,-10.4379033282841));
#37127=CARTESIAN_POINT('Ctrl Pts',(7.41225940988737,-39.6876842086708,-9.65703625032018));
#37128=CARTESIAN_POINT('Ctrl Pts',(7.41272179941099,-36.6876961535581,-9.65763976210219));
#37129=CARTESIAN_POINT('Ctrl Pts',(7.6381238842813,-36.6988428223107,-9.48463238252406));
#37130=CARTESIAN_POINT('Ctrl Pts',(7.85749734347105,-36.7099894910634,-9.30370683240145));
#37131=CARTESIAN_POINT('Ctrl Pts',(8.07029112440213,-36.721136159816,-9.11530862984881));
#37132=CARTESIAN_POINT('Ctrl Pts',(8.28305252155186,-36.7322811322254,-8.92693909846396));
#37133=CARTESIAN_POINT('Ctrl Pts',(8.48923604000689,-36.7434261046349,-8.73109936195701));
#37134=CARTESIAN_POINT('Ctrl Pts',(8.68832482272221,-36.7545710770443,-8.52827427003079));
#37135=CARTESIAN_POINT('Ctrl Pts',(8.88739501900923,-36.7657150089871,-8.3254681133453));
#37136=CARTESIAN_POINT('Ctrl Pts',(9.07937161545807,-36.7768589409299,-8.11567809388224));
#37137=CARTESIAN_POINT('Ctrl Pts',(9.26377477876949,-36.7880028728728,-7.89942574483958));
#37138=CARTESIAN_POINT('Ctrl Pts',(9.44819392555212,-36.7991477707357,-7.68315465174105));
#37139=CARTESIAN_POINT('Ctrl Pts',(9.62503815201837,-36.8102926685985,-7.46042031079913));
#37140=CARTESIAN_POINT('Ctrl Pts',(9.7938671124219,-36.8214375664614,-7.23177828989667));
#37141=CARTESIAN_POINT('Ctrl Pts',(9.96269478289764,-36.8325823791724,-7.00313801592018));
#37142=CARTESIAN_POINT('Ctrl Pts',(10.1235071530054,-36.8437271918833,-6.76859036814335));
#37143=CARTESIAN_POINT('Ctrl Pts',(10.2759059800293,-36.8548720045943,-6.52872166197928));
#37144=CARTESIAN_POINT('Ctrl Pts',(10.4283392073848,-36.8660193329758,-6.28879881128406));
#37145=CARTESIAN_POINT('Ctrl Pts',(10.5723549522108,-36.8771666613574,-6.04355272653906));
#37146=CARTESIAN_POINT('Ctrl Pts',(10.7075990492278,-36.888313989739,-5.7935975741309));
#37147=CARTESIAN_POINT('Ctrl Pts',(10.8191926049702,-36.89751195134,-5.58735282963866));
#37148=CARTESIAN_POINT('Ctrl Pts',(10.9248148936261,-36.9067099129411,-5.37790254937361));
#37149=CARTESIAN_POINT('Ctrl Pts',(11.0242906417777,-36.9159078745421,-5.16560413655685));
#37150=CARTESIAN_POINT('Ctrl Pts',(11.144848515391,-36.9270551814265,-4.90831282991919));
#37151=CARTESIAN_POINT('Ctrl Pts',(11.2564132397565,-36.9382024883108,-4.64676077901745));
#37152=CARTESIAN_POINT('Ctrl Pts',(11.3586997682256,-36.9493497951952,-4.38159672098096));
#37153=CARTESIAN_POINT('Ctrl Pts',(11.460968923368,-36.9604952087139,-4.11647770095578));
#37154=CARTESIAN_POINT('Ctrl Pts',(11.5539629329279,-36.9716406222325,-3.8477481474228));
#37155=CARTESIAN_POINT('Ctrl Pts',(11.6374451793146,-36.9827860357512,-3.57607605462277));
#37156=CARTESIAN_POINT('Ctrl Pts',(11.7209181578843,-36.993930211957,-3.30443412161567));
#37157=CARTESIAN_POINT('Ctrl Pts',(11.794881403517,-37.0050743881628,-3.02985055655883));
#37158=CARTESIAN_POINT('Ctrl Pts',(11.8591480264476,-37.0162185643687,-2.7530089605381));
#37159=CARTESIAN_POINT('Ctrl Pts',(11.9254385293136,-37.0277136921819,-2.46744908859315));
#37160=CARTESIAN_POINT('Ctrl Pts',(11.9814117057185,-37.0392088199951,-2.17948694843876));
#37161=CARTESIAN_POINT('Ctrl Pts',(12.0269190072913,-37.0507039478083,-1.88988609234936));
#37162=CARTESIAN_POINT('Ctrl Pts',(12.0710393075009,-37.061848719582,-1.60911188095839));
#37163=CARTESIAN_POINT('Ctrl Pts',(12.1053222141113,-37.0729934913558,-1.32679764184976));
#37164=CARTESIAN_POINT('Ctrl Pts',(12.129684684297,-37.0841382631295,-1.04364731089154));
#37165=CARTESIAN_POINT('Ctrl Pts',(12.1551959718931,-37.0958085689624,-0.747144966467237));
#37166=CARTESIAN_POINT('Ctrl Pts',(12.1698286831205,-37.1074788747954,-0.449726097386763));
#37167=CARTESIAN_POINT('Ctrl Pts',(12.1735485509352,-37.1191491806283,-0.152203574279836));
#37168=CARTESIAN_POINT('Ctrl Pts',(12.1772684187499,-37.1308194864613,0.145318948827091));
#37169=CARTESIAN_POINT('Ctrl Pts',(12.170075447735,-37.1424897922942,0.442944790376381));
#37170=CARTESIAN_POINT('Ctrl Pts',(12.1519980013252,-37.1541600981272,0.73986135578836));
#37171=CARTESIAN_POINT('Ctrl Pts',(12.134730690394,-37.1653074026142,1.02347169207873));
#37172=CARTESIAN_POINT('Ctrl Pts',(12.1075278724749,-37.1764547071013,1.30651963043172));
#37173=CARTESIAN_POINT('Ctrl Pts',(12.0704497066061,-37.1876020115883,1.58829913123846));
#37174=CARTESIAN_POINT('Ctrl Pts',(12.0333778384804,-37.1987474227007,1.87003077167098));
#37175=CARTESIAN_POINT('Ctrl Pts',(11.9864340059855,-37.2098928338131,2.15049414032514));
#37176=CARTESIAN_POINT('Ctrl Pts',(11.9297301073365,-37.2210382449255,2.4289894639765));
#37177=CARTESIAN_POINT('Ctrl Pts',(11.8730325037096,-37.2321824187225,2.70745387027918));
#37178=CARTESIAN_POINT('Ctrl Pts',(11.806577050753,-37.2433265925194,2.98395040653923));
#37179=CARTESIAN_POINT('Ctrl Pts',(11.730526779452,-37.2544707663164,3.25778939260328));
#37180=CARTESIAN_POINT('Ctrl Pts',(11.6520815091351,-37.2659658959327,3.5402522019744));
#37181=CARTESIAN_POINT('Ctrl Pts',(11.563427371625,-37.277461025549,3.81988707545358));
#37182=CARTESIAN_POINT('Ctrl Pts',(11.4647993244373,-37.2889561551654,4.09595247779841));
#37183=CARTESIAN_POINT('Ctrl Pts',(11.3691773629799,-37.3001009245536,4.36360367860211));
#37184=CARTESIAN_POINT('Ctrl Pts',(11.2641805724472,-37.3112456939418,4.6278995113326));
#37185=CARTESIAN_POINT('Ctrl Pts',(11.1500728991938,-37.3223904633301,4.88818213579082));
#37186=CARTESIAN_POINT('Ctrl Pts',(11.0305843891053,-37.3340607730604,5.16073859156343));
#37187=CARTESIAN_POINT('Ctrl Pts',(10.9011051867154,-37.3457310827908,5.4288939487069));
#37188=CARTESIAN_POINT('Ctrl Pts',(10.7619941971752,-37.3574013925212,5.6919180554509));
#37189=CARTESIAN_POINT('Ctrl Pts',(10.622883207635,-37.3690717022515,5.95494216219492));
#37190=CARTESIAN_POINT('Ctrl Pts',(10.4741405955607,-37.3807420119819,6.21283472606724));
#37191=CARTESIAN_POINT('Ctrl Pts',(10.3161801276997,-37.3924123217123,6.46489580912594));
#37192=CARTESIAN_POINT('Ctrl Pts',(10.1652985893882,-37.4035596315964,6.70566088456128));
#37193=CARTESIAN_POINT('Ctrl Pts',(10.0059621610874,-37.4147069414806,6.94117756831538));
#37194=CARTESIAN_POINT('Ctrl Pts',(9.83856153689548,-37.4258542513647,7.17085470043292));
#37195=CARTESIAN_POINT('Ctrl Pts',(9.67118934551754,-37.4369996678904,7.40049282213932));
#37196=CARTESIAN_POINT('Ctrl Pts',(9.49575584989997,-37.448145084416,7.62429315693641));
#37197=CARTESIAN_POINT('Ctrl Pts',(9.31269417572409,-37.4592905009417,7.84169480657305));
#37198=CARTESIAN_POINT('Ctrl Pts',(9.12965282422267,-37.4704346801539,8.05907232126732));
#37199=CARTESIAN_POINT('Ctrl Pts',(8.93898515694899,-37.4815788593662,8.27005236527149));
#37200=CARTESIAN_POINT('Ctrl Pts',(8.74116436747312,-37.4927230385784,8.47410737191938));
#37201=CARTESIAN_POINT('Ctrl Pts',(8.53711391475841,-37.5042181641383,8.68458836633621));
#37202=CARTESIAN_POINT('Ctrl Pts',(8.32545271468955,-37.5157132896982,8.88770087711783));
#37203=CARTESIAN_POINT('Ctrl Pts',(8.10674193044602,-37.5272084152581,9.08290622670676));
#37204=CARTESIAN_POINT('Ctrl Pts',(7.89469705879956,-37.5383531899996,9.27216206720614));
#37205=CARTESIAN_POINT('Ctrl Pts',(7.67602616543338,-37.549497964741,9.45398541568634));
#37206=CARTESIAN_POINT('Ctrl Pts',(7.45127581728972,-37.5606427394824,9.62792495528883));
#37207=CARTESIAN_POINT('Ctrl Pts',(7.21592747991917,-37.5723130404516,9.81006652608755));
#37208=CARTESIAN_POINT('Ctrl Pts',(6.97391279638077,-37.5839833414207,9.98356268944984));
#37209=CARTESIAN_POINT('Ctrl Pts',(6.72589631532803,-37.5956536423899,10.1479440777656));
#37210=CARTESIAN_POINT('Ctrl Pts',(6.47787983427525,-37.6073239433591,10.3123254660813));
#37211=CARTESIAN_POINT('Ctrl Pts',(6.22386184020973,-37.6189942443282,10.4675919013181));
#37212=CARTESIAN_POINT('Ctrl Pts',(5.96454059505376,-37.6306645452974,10.6133267988862));
#37213=CARTESIAN_POINT('Ctrl Pts',(5.71684074067779,-37.6418118458159,10.7525306380603));
#37214=CARTESIAN_POINT('Ctrl Pts',(5.46422853582719,-37.6529591463344,10.8830800410514));
#37215=CARTESIAN_POINT('Ctrl Pts',(5.20732992919923,-37.6641064468529,11.0046428955449));
#37216=CARTESIAN_POINT('Ctrl Pts',(4.95047495704132,-37.675251853992,11.1261851024731));
#37217=CARTESIAN_POINT('Ctrl Pts',(4.68933527768077,-37.686397261131,11.238743694257));
#37218=CARTESIAN_POINT('Ctrl Pts',(4.42455961597228,-37.69754266827,11.3420334356194));
#37219=CARTESIAN_POINT('Ctrl Pts',(4.159813348394,-37.7086868380991,11.4453117102476));
#37220=CARTESIAN_POINT('Ctrl Pts',(3.8914321529359,-37.7198310079283,11.5393230922518));
#37221=CARTESIAN_POINT('Ctrl Pts',(3.62008398605781,-37.7309751777574,11.6238307878207));
#37222=CARTESIAN_POINT('Ctrl Pts',(3.34019026538018,-37.7424703103512,11.7109998798798));
#37223=CARTESIAN_POINT('Ctrl Pts',(3.05713994801186,-37.7539654429449,11.7880568895911));
#37224=CARTESIAN_POINT('Ctrl Pts',(2.77168355359457,-37.7654605755387,11.8547973634615));
#37225=CARTESIAN_POINT('Ctrl Pts',(2.4949277575709,-37.7766053410216,11.919503613993));
#37226=CARTESIAN_POINT('Ctrl Pts',(2.21591065681822,-37.7877501065045,11.9745128402229));
#37227=CARTESIAN_POINT('Ctrl Pts',(1.93532814556136,-37.7988948719875,12.0196903129406));
#37228=CARTESIAN_POINT('Ctrl Pts',(1.64151428134749,-37.8105651881366,12.0669982074175));
#37229=CARTESIAN_POINT('Ctrl Pts',(1.34598412860745,-37.8222355042858,12.1035247188786));
#37230=CARTESIAN_POINT('Ctrl Pts',(1.04954582011979,-37.833905820435,12.1291757272071));
#37231=CARTESIAN_POINT('Ctrl Pts',(0.753107511632138,-37.8455761365842,
12.1548267355356));
#37232=CARTESIAN_POINT('Ctrl Pts',(0.455761382408362,-37.8572464527333,
12.1696022205541));
#37233=CARTESIAN_POINT('Ctrl Pts',(0.158319908679642,-37.8689167688825,
12.173470542804));
#37234=CARTESIAN_POINT('Ctrl Pts',(-0.12579174714374,-37.8800640806665,
12.1771655064749));
#37235=CARTESIAN_POINT('Ctrl Pts',(-0.410075244090248,-37.8912113924504,
12.1709105297779));
#37236=CARTESIAN_POINT('Ctrl Pts',(-0.693822027690313,-37.9023587042343,
12.1547135401823));
#37237=CARTESIAN_POINT('Ctrl Pts',(-0.977520616905607,-37.9135041226476,
12.138519301645));
#37238=CARTESIAN_POINT('Ctrl Pts',(-1.26068240856468,-37.9246495410609,
12.1123864367958));
#37239=CARTESIAN_POINT('Ctrl Pts',(-1.54260128195007,-37.9357949594741,
12.076374933519));
#37240=CARTESIAN_POINT('Ctrl Pts',(-1.82448885756125,-37.946939140557,12.0403674281296));
#37241=CARTESIAN_POINT('Ctrl Pts',(-2.10513352590396,-37.9580833216399,
11.994483508031));
#37242=CARTESIAN_POINT('Ctrl Pts',(-2.38383546099295,-37.9692275027228,
11.938834898972));
#37243=CARTESIAN_POINT('Ctrl Pts',(-2.67131404013532,-37.9807226268682,
11.8814338512957));
#37244=CARTESIAN_POINT('Ctrl Pts',(-2.95672525267067,-37.9922177510136,
11.8136431952161));
#37245=CARTESIAN_POINT('Ctrl Pts',(-3.23931225686239,-38.003712875159,11.7356425624054));
#37246=CARTESIAN_POINT('Ctrl Pts',(-3.5132865939056,-38.0148576517066,11.660019227481));
#37247=CARTESIAN_POINT('Ctrl Pts',(-3.78460605649515,-38.0260024282542,
11.574799132407));
#37248=CARTESIAN_POINT('Ctrl Pts',(-4.05259512972714,-38.0371472048018,
11.4801969915377));
#37249=CARTESIAN_POINT('Ctrl Pts',(-4.33322097422808,-38.0488175027461,
11.3811339761959));
#37250=CARTESIAN_POINT('Ctrl Pts',(-4.61019448973457,-38.0604878006904,
11.2717829285037));
#37251=CARTESIAN_POINT('Ctrl Pts',(-4.88276104735159,-38.0721580986347,
11.1524479287942));
#37252=CARTESIAN_POINT('Ctrl Pts',(-5.15532760496862,-38.083828396579,11.0331129290847));
#37253=CARTESIAN_POINT('Ctrl Pts',(-5.42348690088356,-38.0954986945234,
10.903794119955));
#37254=CARTESIAN_POINT('Ctrl Pts',(-5.68651039168178,-38.1071689924677,
10.7648525217624));
#37255=CARTESIAN_POINT('Ctrl Pts',(-5.93774685158698,-38.1183163022865,
10.6321373975067));
#37256=CARTESIAN_POINT('Ctrl Pts',(-6.18437272836615,-38.1294636121054,
10.4906033555107));
#37257=CARTESIAN_POINT('Ctrl Pts',(-6.42576965953203,-38.1406109219243,
10.340596430218));
#37258=CARTESIAN_POINT('Ctrl Pts',(-6.66712559058785,-38.1517563384261,
10.1906149828815));
#37259=CARTESIAN_POINT('Ctrl Pts',(-6.9032541226648,-38.1629017549279,10.0321636661054));
#37260=CARTESIAN_POINT('Ctrl Pts',(-7.13356394341092,-38.1740471714297,
9.86563306206286));
#37261=CARTESIAN_POINT('Ctrl Pts',(-7.36384819705636,-38.1851913506591,
9.69912094487725));
#37262=CARTESIAN_POINT('Ctrl Pts',(-7.58831481311788,-38.1963355298885,
9.52453148764227));
#37263=CARTESIAN_POINT('Ctrl Pts',(-7.80640276521373,-38.2074797091179,
9.34229768939438));
#37264=CARTESIAN_POINT('Ctrl Pts',(-8.03135862286497,-38.2189748346958,
9.15432508483766));
#37265=CARTESIAN_POINT('Ctrl Pts',(-8.24952732595125,-38.2304699602737,
8.95821905765051));
#37266=CARTESIAN_POINT('Ctrl Pts',(-8.46033028003315,-38.2419650858516,
8.75449951754835));
#37267=CARTESIAN_POINT('Ctrl Pts',(-8.66470833983174,-38.2531098607101,
8.55698898203202));
#37268=CARTESIAN_POINT('Ctrl Pts',(-8.86216279097333,-38.2642546355686,
8.35232234771498));
#37269=CARTESIAN_POINT('Ctrl Pts',(-9.05220323824906,-38.2753994104272,
8.14101141034904));
#37270=CARTESIAN_POINT('Ctrl Pts',(-9.25120494426631,-38.2870697113648,
7.91973621531168));
#37271=CARTESIAN_POINT('Ctrl Pts',(-9.44207640298544,-38.2987400123023,
7.69117525897117));
#37272=CARTESIAN_POINT('Ctrl Pts',(-9.6243005169155,-38.3104103132399,7.45595666632393));
#37273=CARTESIAN_POINT('Ctrl Pts',(-9.80652463084557,-38.3220806141775,
7.22073807367666));
#37274=CARTESIAN_POINT('Ctrl Pts',(-9.98010120145821,-38.3337509151151,
6.97886211532039));
#37275=CARTESIAN_POINT('Ctrl Pts',(-10.144563284333,-38.3454212160527,6.73099443025792));
#37276=CARTESIAN_POINT('Ctrl Pts',(-10.3016546456759,-38.3565684873844,
6.49423546795641));
#37277=CARTESIAN_POINT('Ctrl Pts',(-10.4504774518845,-38.367715758716,6.25193932153469));
#37278=CARTESIAN_POINT('Ctrl Pts',(-10.5906543344632,-38.3788630300476,
6.00470573949428));
#37279=CARTESIAN_POINT('Ctrl Pts',(-10.7308074057654,-38.3900084078376,
5.7575141540162));
#37280=CARTESIAN_POINT('Ctrl Pts',(-10.8623173540756,-38.4011537856276,
5.50538703934738));
#37281=CARTESIAN_POINT('Ctrl Pts',(-10.9848518805822,-38.4122991634176,
5.24895031522197));
#37282=CARTESIAN_POINT('Ctrl Pts',(-11.1073728029286,-38.4234433038135,
4.99254206149096));
#37283=CARTESIAN_POINT('Ctrl Pts',(-11.2209201783031,-38.4345874442093,
4.73182539434702));
#37284=CARTESIAN_POINT('Ctrl Pts',(-11.3252085991643,-38.4457315846052,
4.46744898520573));
#37285=CARTESIAN_POINT('Ctrl Pts',(-11.4327818597973,-38.4572267391913,
4.19474534149411));
#37286=CARTESIAN_POINT('Ctrl Pts',(-11.5305033242619,-38.4687218937773,
3.91814794521018));
#37287=CARTESIAN_POINT('Ctrl Pts',(-11.6181137451896,-38.4802170483634,
3.63839020087693));
#37288=CARTESIAN_POINT('Ctrl Pts',(-11.7030534493892,-38.4913617845709,
3.36716059371813));
#37289=CARTESIAN_POINT('Ctrl Pts',(-11.7784893469094,-38.5025065207784,
3.09296073127381));
#37290=CARTESIAN_POINT('Ctrl Pts',(-11.8442357567959,-38.513651256986,2.81647467367221));
#37291=CARTESIAN_POINT('Ctrl Pts',(-11.9130830140131,-38.5253216207613,
2.52694849638708));
#37292=CARTESIAN_POINT('Ctrl Pts',(-11.9713047289161,-38.5369919845366,
2.23491559225353));
#37293=CARTESIAN_POINT('Ctrl Pts',(-12.0187474391742,-38.5486623483119,
1.94117496463956));
#37294=CARTESIAN_POINT('Ctrl Pts',(-12.0661901494323,-38.5603327120872,
1.64743433702562));
#37295=CARTESIAN_POINT('Ctrl Pts',(-12.1028538102164,-38.5720030758626,
1.35198631855737));
#37296=CARTESIAN_POINT('Ctrl Pts',(-12.1286469510863,-38.5836734396379,
1.05563885202526));
#37297=CARTESIAN_POINT('Ctrl Pts',(-12.1549901730804,-38.5955926931028,
0.752971288674556));
#37298=CARTESIAN_POINT('Ctrl Pts',(-12.1700001024465,-38.6075119465678,
0.449311157315627));
#37299=CARTESIAN_POINT('Ctrl Pts',(-12.173630879507,-38.6194312000327,0.145469789009793));
#37300=CARTESIAN_POINT('Ctrl Pts',(-12.1742091193982,-38.6213294680102,
0.0970798171563845));
#37301=CARTESIAN_POINT('Ctrl Pts',(-12.1744988461963,-38.6232277359876,
0.0486852550215822));
#37302=CARTESIAN_POINT('Ctrl Pts',(-12.1744999965607,-38.6251260039651,
0.00028938649696687));
#37303=CARTESIAN_POINT('Origin',(0.,-13.3748739960349,0.));
#37304=CARTESIAN_POINT('',(7.412721799411,-33.6876951030527,-9.65763976210218));
#37305=CARTESIAN_POINT('',(7.412721799411,-33.9374387645002,-9.65763976210218));
#37306=CARTESIAN_POINT('',(7.41272179941101,-13.3748739960349,-9.65763976210217));
#37307=CARTESIAN_POINT('',(-12.1744999966649,-35.8748739960676,-0.000284967810357368));
#37308=CARTESIAN_POINT('Ctrl Pts',(7.41272179941099,-33.9374387645002,-9.65763976210218));
#37309=CARTESIAN_POINT('Ctrl Pts',(7.638184643001,-33.9485835323456,-9.48458574716623));
#37310=CARTESIAN_POINT('Ctrl Pts',(7.857581029635,-33.959728300191,-9.30363583840648));
#37311=CARTESIAN_POINT('Ctrl Pts',(8.07036553404239,-33.9708730680363,-9.11524275030241));
#37312=CARTESIAN_POINT('Ctrl Pts',(8.28315653782117,-33.9820181762918,-8.92684390784772));
#37313=CARTESIAN_POINT('Ctrl Pts',(8.48933505810636,-33.9931632845472,-8.73100161084966));
#37314=CARTESIAN_POINT('Ctrl Pts',(8.68839053721542,-34.0043083928026,-8.52820732175441));
#37315=CARTESIAN_POINT('Ctrl Pts',(8.88748351632993,-34.0154556006818,-8.32537482830037));
#37316=CARTESIAN_POINT('Ctrl Pts',(9.07945058689651,-34.0266028085611,-8.11558791699093));
#37317=CARTESIAN_POINT('Ctrl Pts',(9.26381869082178,-34.0377500164403,-7.89937424822885));
#37318=CARTESIAN_POINT('Ctrl Pts',(9.29659092252151,-34.0397314810844,-7.8609413289849));
#37319=CARTESIAN_POINT('Ctrl Pts',(9.3291231530178,-34.0417129457284,-7.82230543318109));
#37320=CARTESIAN_POINT('Ctrl Pts',(9.36141285701634,-34.0436944103725,-7.78346963574017));
#37321=CARTESIAN_POINT('Ctrl Pts',(9.54306798782381,-34.0548417166199,-7.56498755041469));
#37322=CARTESIAN_POINT('Ctrl Pts',(9.71709831636431,-34.0659890228673,-7.34011069825187));
#37323=CARTESIAN_POINT('Ctrl Pts',(9.88306413050628,-34.0771363291147,-7.10939474514534));
#37324=CARTESIAN_POINT('Ctrl Pts',(10.0490017553756,-34.0882817419936,-6.87871797911443));
#37325=CARTESIAN_POINT('Ctrl Pts',(10.2068774448553,-34.0994271548724,-6.64220430866852));
#37326=CARTESIAN_POINT('Ctrl Pts',(10.356293478878,-34.1105725677512,-6.40044026839951));
#37327=CARTESIAN_POINT('Ctrl Pts',(10.5056929254,-34.1217167433161,-6.15870306769419));
#37328=CARTESIAN_POINT('Ctrl Pts',(10.6466344516049,-34.132860918881,-5.91171688792128));
#37329=CARTESIAN_POINT('Ctrl Pts',(10.7787645084179,-34.1440050944459,-5.66009592869868));
#37330=CARTESIAN_POINT('Ctrl Pts',(10.9150556091399,-34.1555002227386,-5.40055091430638));
#37331=CARTESIAN_POINT('Ctrl Pts',(11.0419711186301,-34.1669953510312,-5.13607473106142));
#37332=CARTESIAN_POINT('Ctrl Pts',(11.1591743840538,-34.1784904793239,-4.86736862342242));
#37333=CARTESIAN_POINT('Ctrl Pts',(11.2728054403154,-34.1896352504617,-4.6068523423738));
#37334=CARTESIAN_POINT('Ctrl Pts',(11.3773074082564,-34.2007800215995,-4.34236042018621));
#37335=CARTESIAN_POINT('Ctrl Pts',(11.4724220783378,-34.2119247927374,-4.07455297013887));
#37336=CARTESIAN_POINT('Ctrl Pts',(11.5720219152447,-34.2235950996074,-3.79411696248277));
#37337=CARTESIAN_POINT('Ctrl Pts',(11.6613277225685,-34.2352654064774,-3.5100455127723));
#37338=CARTESIAN_POINT('Ctrl Pts',(11.7401009596519,-34.2469357133475,-3.22311645883009));
#37339=CARTESIAN_POINT('Ctrl Pts',(11.8188741967353,-34.2586060202175,-2.93618740488788));
#37340=CARTESIAN_POINT('Ctrl Pts',(11.8871147832216,-34.2702763270876,-2.64640107256773));
#37341=CARTESIAN_POINT('Ctrl Pts',(11.9446448465681,-34.2819466339576,-2.35455085724545));
#37342=CARTESIAN_POINT('Ctrl Pts',(11.9995967207427,-34.2930939402076,-2.07577980473253));
#37343=CARTESIAN_POINT('Ctrl Pts',(12.0447933593859,-34.3042412464575,-1.79504252936051));
#37344=CARTESIAN_POINT('Ctrl Pts',(12.0801145768396,-34.3153885527074,-1.51303736253506));
#37345=CARTESIAN_POINT('Ctrl Pts',(12.1154297949892,-34.3265339655889,-1.23108009425072));
#37346=CARTESIAN_POINT('Ctrl Pts',(12.1408729076176,-34.3376793784703,-0.947855629040423));
#37347=CARTESIAN_POINT('Ctrl Pts',(12.1563753727891,-34.3488247913517,-0.664069308015263));
#37348=CARTESIAN_POINT('Ctrl Pts',(12.1718761169461,-34.3599689669192,-0.380314491679434));
#37349=CARTESIAN_POINT('Ctrl Pts',(12.1774384027462,-34.3711131424867,-0.0959982103629502));
#37350=CARTESIAN_POINT('Ctrl Pts',(12.1730457121208,-34.3822573180542,0.188171040858175));
#37351=CARTESIAN_POINT('Ctrl Pts',(12.1685146867457,-34.3937524463449,0.481289358968064));
#37352=CARTESIAN_POINT('Ctrl Pts',(12.1533915147295,-34.4052475746356,0.774250939540593));
#37353=CARTESIAN_POINT('Ctrl Pts',(12.1277161686617,-34.4167427029263,1.06627894210765));
#37354=CARTESIAN_POINT('Ctrl Pts',(12.1028233750677,-34.4278874740667,1.34940629596561));
#37355=CARTESIAN_POINT('Ctrl Pts',(12.0680121410407,-34.4390322452072,1.63165585970076));
#37356=CARTESIAN_POINT('Ctrl Pts',(12.0233716344006,-34.4501770163476,1.91232444713011));
#37357=CARTESIAN_POINT('Ctrl Pts',(11.9766260884783,-34.4618473232134,2.20622806360036));
#37358=CARTESIAN_POINT('Ctrl Pts',(11.9191020086131,-34.4735176300793,2.49839769914427));
#37359=CARTESIAN_POINT('Ctrl Pts',(11.8509621693877,-34.4851879369452,2.78803621026358));
#37360=CARTESIAN_POINT('Ctrl Pts',(11.7828223301624,-34.496858243811,3.07767472138287));
#37361=CARTESIAN_POINT('Ctrl Pts',(11.7040668169537,-34.5085285506769,3.36478178350285));
#37362=CARTESIAN_POINT('Ctrl Pts',(11.6149191198025,-34.5201988575427,3.64857562487699));
#37363=CARTESIAN_POINT('Ctrl Pts',(11.5297665448279,-34.5313461637786,3.91965134670903));
#37364=CARTESIAN_POINT('Ctrl Pts',(11.4351073244025,-34.5424934700145,4.18778524183307));
#37365=CARTESIAN_POINT('Ctrl Pts',(11.3311701091902,-34.5536407762504,4.45230661641746));
#37366=CARTESIAN_POINT('Ctrl Pts',(11.2272505477016,-34.5647861891177,4.71678306207768));
#37367=CARTESIAN_POINT('Ctrl Pts',(11.1140562351574,-34.575931601985,4.97764796404744));
#37368=CARTESIAN_POINT('Ctrl Pts',(10.9918645231726,-34.5870770148522,5.2342491872493));
#37369=CARTESIAN_POINT('Ctrl Pts',(10.8696863763659,-34.5982211904055,5.49082192372942));
#37370=CARTESIAN_POINT('Ctrl Pts',(10.7385129393202,-34.6093653659588,5.743131685842));
#37371=CARTESIAN_POINT('Ctrl Pts',(10.5986687532571,-34.6205095415121,5.99054846476783));
#37372=CARTESIAN_POINT('Ctrl Pts',(10.4544205894249,-34.6320046698134,6.24575690114288));
#37373=CARTESIAN_POINT('Ctrl Pts',(10.3009468455545,-34.6434997981147,6.49575891739394));
#37374=CARTESIAN_POINT('Ctrl Pts',(10.1386543714878,-34.6549949264161,6.73989152624218));
#37375=CARTESIAN_POINT('Ctrl Pts',(9.98130836963331,-34.6661396975425,6.97658327763416));
#37376=CARTESIAN_POINT('Ctrl Pts',(9.81567339958986,-34.6772844686689,7.20775787559392));
#37377=CARTESIAN_POINT('Ctrl Pts',(9.64216426105065,-34.6884292397953,7.43284054806221));
#37378=CARTESIAN_POINT('Ctrl Pts',(9.46047323556585,-34.7000995466841,7.66853707634841));
#37379=CARTESIAN_POINT('Ctrl Pts',(9.27014774830922,-34.7117698535728,7.89755306912699));
#37380=CARTESIAN_POINT('Ctrl Pts',(9.07171219303635,-34.7234401604616,8.11926647775005));
#37381=CARTESIAN_POINT('Ctrl Pts',(8.87327663776348,-34.7351104673503,8.3409798863731));
#37382=CARTESIAN_POINT('Ctrl Pts',(8.66673124476339,-34.7467807742391,8.55539046669953));
#37383=CARTESIAN_POINT('Ctrl Pts',(8.45264636382744,-34.7584510811278,8.76191872240749));
#37384=CARTESIAN_POINT('Ctrl Pts',(8.24815561997432,-34.769598387403,8.95919148847938));
#37385=CARTESIAN_POINT('Ctrl Pts',(8.03672521997992,-34.7807456936781,9.14933180573395));
#37386=CARTESIAN_POINT('Ctrl Pts',(7.81887688946857,-34.7918929999533,9.33186018097862));
#37387=CARTESIAN_POINT('Ctrl Pts',(7.60106556046648,-34.80303841286,9.51435755380363));
#37388=CARTESIAN_POINT('Ctrl Pts',(7.37683868168765,-34.8141838257667,9.68924539461877));
#37389=CARTESIAN_POINT('Ctrl Pts',(7.14675186016544,-34.8253292386734,9.85608381149541));
#37390=CARTESIAN_POINT('Ctrl Pts',(6.91669058185361,-34.8364734142662,10.0229037067168));
#37391=CARTESIAN_POINT('Ctrl Pts',(6.68077087572726,-34.8476175898589,10.1816758058515));
#37392=CARTESIAN_POINT('Ctrl Pts',(6.43957919596821,-34.8587617654517,10.3320022274898));
#37393=CARTESIAN_POINT('Ctrl Pts',(6.19079190131112,-34.8702568937235,10.4870627328614));
#37394=CARTESIAN_POINT('Ctrl Pts',(5.93639544874569,-34.8817520219953,10.6331368327272));
#37395=CARTESIAN_POINT('Ctrl Pts',(5.67706434630255,-34.893247150267,10.7698370766665));
#37396=CARTESIAN_POINT('Ctrl Pts',(5.42563733091963,-34.9043919214325,10.9023708684562));
#37397=CARTESIAN_POINT('Ctrl Pts',(5.16957226212979,-34.9155366925979,11.0260936195817));
#37398=CARTESIAN_POINT('Ctrl Pts',(4.90950841370616,-34.9266814637634,11.1406991425919));
#37399=CARTESIAN_POINT('Ctrl Pts',(4.63718116174956,-34.9383517705883,11.2607089299177));
#37400=CARTESIAN_POINT('Ctrl Pts',(4.3604692188947,-34.9500220774132,11.3707208190715));
#37401=CARTESIAN_POINT('Ctrl Pts',(4.08013071339311,-34.9616923842381,11.4704395561646));
#37402=CARTESIAN_POINT('Ctrl Pts',(3.7997922078915,-34.973362691063,11.5701582932578));
#37403=CARTESIAN_POINT('Ctrl Pts',(3.51582745878365,-34.985032997888,11.6595837741217));
#37404=CARTESIAN_POINT('Ctrl Pts',(3.22901458356905,-34.9967033047129,11.7384801004686));
#37405=CARTESIAN_POINT('Ctrl Pts',(2.95505512490198,-35.0078506109063,11.8138407161336));
#37406=CARTESIAN_POINT('Ctrl Pts',(2.67841538341678,-35.0189979170997,11.8796176615914));
#37407=CARTESIAN_POINT('Ctrl Pts',(2.39978292570686,-35.0301452232932,11.9356395789872));
#37408=CARTESIAN_POINT('Ctrl Pts',(2.1211977936875,-35.0412906361179,11.9916519810668));
#37409=CARTESIAN_POINT('Ctrl Pts',(1.8406208825985,-35.0524360489427,12.0379126105056));
#37410=CARTESIAN_POINT('Ctrl Pts',(1.55875055819259,-35.0635814617674,12.0743010956053));
#37411=CARTESIAN_POINT('Ctrl Pts',(1.27691152577331,-35.0747256372782,12.1106855410175));
#37412=CARTESIAN_POINT('Ctrl Pts',(0.9937796312455,-35.0858698127889,12.1371999964074));
#37413=CARTESIAN_POINT('Ctrl Pts',(0.710060222313936,-35.0970139882996,
12.1537757396904));
#37414=CARTESIAN_POINT('Ctrl Pts',(0.417405910368738,-35.1085091166328,
12.1708734869462));
#37415=CARTESIAN_POINT('Ctrl Pts',(0.124126775978267,-35.120004244966,12.1773963708101));
#37416=CARTESIAN_POINT('Ctrl Pts',(-0.168999507858268,-35.1314993732992,
12.1733269658029));
#37417=CARTESIAN_POINT('Ctrl Pts',(-0.453191666266195,-35.1426441443837,
12.1693815912111));
#37418=CARTESIAN_POINT('Ctrl Pts',(-0.737239874493748,-35.1537889154681,
12.155480050062));
#37419=CARTESIAN_POINT('Ctrl Pts',(-1.02043628531443,-35.1649336865525,
12.1316594098917));
#37420=CARTESIAN_POINT('Ctrl Pts',(-1.31698692942595,-35.1766039935101,
12.1067154984728));
#37421=CARTESIAN_POINT('Ctrl Pts',(-1.61260319276483,-35.1882743004677,
12.0708945277011));
#37422=CARTESIAN_POINT('Ctrl Pts',(-1.9064780983657,-35.1999446074253,12.0243000424329));
#37423=CARTESIAN_POINT('Ctrl Pts',(-2.20035300396654,-35.2116149143829,
11.9777055571647));
#37424=CARTESIAN_POINT('Ctrl Pts',(-2.49248622184222,-35.2232852213404,
11.920337618608));
#37425=CARTESIAN_POINT('Ctrl Pts',(-2.78208162737388,-35.234955528298,11.8523614553653));
#37426=CARTESIAN_POINT('Ctrl Pts',(-3.05869891833767,-35.2461028346215,
11.7874316195767));
#37427=CARTESIAN_POINT('Ctrl Pts',(-3.33308347439242,-35.2572501409449,
11.7128040752966));
#37428=CARTESIAN_POINT('Ctrl Pts',(-3.60454956580632,-35.2683974472683,
11.6286573892967));
#37429=CARTESIAN_POINT('Ctrl Pts',(-3.87596954874084,-35.2795428602233,
11.5445249956003));
#37430=CARTESIAN_POINT('Ctrl Pts',(-4.14447180201004,-35.2906882731782,
11.4508767671215));
#37431=CARTESIAN_POINT('Ctrl Pts',(-4.40938551257941,-35.3018336861332,
11.3479412076136));
#37432=CARTESIAN_POINT('Ctrl Pts',(-4.67426981361183,-35.3129778617742,
11.2450170755518));
#37433=CARTESIAN_POINT('Ctrl Pts',(-4.9355661188806,-35.3241220374152,11.1328077678662));
#37434=CARTESIAN_POINT('Ctrl Pts',(-5.19262220129437,-35.3352662130561,
11.0115904811532));
#37435=CARTESIAN_POINT('Ctrl Pts',(-5.45777349882198,-35.3467613412917,
10.8865558173052));
#37436=CARTESIAN_POINT('Ctrl Pts',(-5.71841290697284,-35.3582564695273,
10.7519367395923));
#37437=CARTESIAN_POINT('Ctrl Pts',(-5.97384924005429,-35.3697515977629,
10.6080900970487));
#37438=CARTESIAN_POINT('Ctrl Pts',(-6.22150019559604,-35.3808963689756,
10.4686277188989));
#37439=CARTESIAN_POINT('Ctrl Pts',(-6.46426030265879,-35.3920411401884,
10.3204920726344));
#37440=CARTESIAN_POINT('Ctrl Pts',(-6.70152576426091,-35.4031859114011,
10.1640544410657));
#37441=CARTESIAN_POINT('Ctrl Pts',(-6.94997956062028,-35.4148562181481,
10.0002399389706));
#37442=CARTESIAN_POINT('Ctrl Pts',(-7.19240777343318,-35.4265265248951,
9.82732182100891));
#37443=CARTESIAN_POINT('Ctrl Pts',(-7.42815137572672,-35.4381968316421,
9.64577717912296));
#37444=CARTESIAN_POINT('Ctrl Pts',(-7.66389497802024,-35.4498671383891,
9.46423253723702));
#37445=CARTESIAN_POINT('Ctrl Pts',(-7.89295370933516,-35.4615374451361,
9.27406158308419));
#37446=CARTESIAN_POINT('Ctrl Pts',(-8.11470759005776,-35.4732077518831,
9.0757903775847));
#37447=CARTESIAN_POINT('Ctrl Pts',(-8.32652365126632,-35.4843550580777,
8.88640462404963));
#37448=CARTESIAN_POINT('Ctrl Pts',(-8.53173846022696,-35.4955023642722,
8.68957211823678));
#37449=CARTESIAN_POINT('Ctrl Pts',(-8.72983535399109,-35.5066496704667,
8.48577780419729));
#37450=CARTESIAN_POINT('Ctrl Pts',(-8.92789860102508,-35.5177950832929,
8.28201810459399));
#37451=CARTESIAN_POINT('Ctrl Pts',(-9.11884616072902,-35.528940496119,8.07129914875044));
#37452=CARTESIAN_POINT('Ctrl Pts',(-9.30219836495137,-35.5400859089451,
7.85414259032112));
#37453=CARTESIAN_POINT('Ctrl Pts',(-9.48553021423546,-35.5512300844576,
7.63701013963763));
#37454=CARTESIAN_POINT('Ctrl Pts',(-9.66126821973614,-35.56237425997,7.41344171722012));
#37455=CARTESIAN_POINT('Ctrl Pts',(-9.82897233455958,-35.5735184354825,
7.18399283800189));
#37456=CARTESIAN_POINT('Ctrl Pts',(-10.0019577940555,-35.5850135638146,
6.94731814552835));
#37457=CARTESIAN_POINT('Ctrl Pts',(-10.1663949731909,-35.5965086921468,
6.70438685320291));
#37458=CARTESIAN_POINT('Ctrl Pts',(-10.3218477339838,-35.6080038204789,
6.45584305931104));
#37459=CARTESIAN_POINT('Ctrl Pts',(-10.4725624875548,-35.6191485915657,
6.21487457179775));
#37460=CARTESIAN_POINT('Ctrl Pts',(-10.6148322327911,-35.6302933626525,
5.96863087732274));
#37461=CARTESIAN_POINT('Ctrl Pts',(-10.7483044718205,-35.6414381337393,
5.71772692868804));
#37462=CARTESIAN_POINT('Ctrl Pts',(-10.8880706444308,-35.6531084406941,
5.45499151008326));
#37463=CARTESIAN_POINT('Ctrl Pts',(-11.0181894980664,-35.6647787476489,
5.18714603041487));
#37464=CARTESIAN_POINT('Ctrl Pts',(-11.1383106735327,-35.6764490546037,
4.91492477967551));
#37465=CARTESIAN_POINT('Ctrl Pts',(-11.2584318489989,-35.6881193615585,
4.64270352893615));
#37466=CARTESIAN_POINT('Ctrl Pts',(-11.3685552188829,-35.6997896685134,
4.36610681761556));
#37467=CARTESIAN_POINT('Ctrl Pts',(-11.4683881438355,-35.7114599754682,
4.08589324778976));
#37468=CARTESIAN_POINT('Ctrl Pts',(-11.5636605180159,-35.7225971614369,
3.81848034680994));
#37469=CARTESIAN_POINT('Ctrl Pts',(-11.6495908466594,-35.7337343474056,
3.54769134091233));
#37470=CARTESIAN_POINT('Ctrl Pts',(-11.7259574475739,-35.7448715333744,
3.27419794570916));
#37471=CARTESIAN_POINT('Ctrl Pts',(-11.8023132777083,-35.7560071485493,
3.00074312413884));
#37472=CARTESIAN_POINT('Ctrl Pts',(-11.8691079996121,-35.7671427637243,
2.72458493211118));
#37473=CARTESIAN_POINT('Ctrl Pts',(-11.9261699500892,-35.7782783788992,
2.44640973093008));
#37474=CARTESIAN_POINT('Ctrl Pts',(-11.9832242232964,-35.7894124958583,
2.16827195619616));
#37475=CARTESIAN_POINT('Ctrl Pts',(-12.0305482866717,-35.8005466128173,
1.88811797652426));
#37476=CARTESIAN_POINT('Ctrl Pts',(-12.0680214761787,-35.8116807297764,
1.60664492047536));
#37477=CARTESIAN_POINT('Ctrl Pts',(-12.1054959778234,-35.8228152366007,
1.32516200854266));
#37478=CARTESIAN_POINT('Ctrl Pts',(-12.1331188783859,-35.833949743425,1.04236019299949));
#37479=CARTESIAN_POINT('Ctrl Pts',(-12.1508211493447,-35.8450842502493,
0.758943770405247));
#37480=CARTESIAN_POINT('Ctrl Pts',(-12.1666082922634,-35.8550141655112,
0.506188879272841));
#37481=CARTESIAN_POINT('Ctrl Pts',(-12.1745059239959,-35.864944080773,0.252945394476219));
#37482=CARTESIAN_POINT('Ctrl Pts',(-12.1744999966649,-35.8748739960349,
-0.000284966977105543));
#37483=CARTESIAN_POINT('Ctrl Pts',(-12.1744999966649,-35.8748739960676,
-0.000284967810371163));
#37484=CARTESIAN_POINT('Ctrl Pts',(-12.1744930883501,-35.8864472961776,
-0.295424542797684));
#37485=CARTESIAN_POINT('Ctrl Pts',(-12.163749488268,-35.8980205962875,-0.590512724686085));
#37486=CARTESIAN_POINT('Ctrl Pts',(-12.1423063610032,-35.9095938963975,
-0.884786124179511));
#37487=CARTESIAN_POINT('Ctrl Pts',(-12.1208567139894,-35.9211707153511,
-1.17914899703588));
#37488=CARTESIAN_POINT('Ctrl Pts',(-12.0887010545349,-35.9327475343047,
-1.47269637376915));
#37489=CARTESIAN_POINT('Ctrl Pts',(-12.0459284961632,-35.9443243532583,
-1.76466906680104));
#37490=CARTESIAN_POINT('Ctrl Pts',(-12.0392930536843,-35.9461203018566,
-1.80996371560749));
#37491=CARTESIAN_POINT('Ctrl Pts',(-12.0324022028897,-35.9479162504549,
-1.85522048095315));
#37492=CARTESIAN_POINT('Ctrl Pts',(-12.0252563877582,-35.9497121990533,
-1.90043654423916));
#37493=CARTESIAN_POINT('Ctrl Pts',(-11.9809028943906,-35.9608595059425,
-2.18108897173295));
#37494=CARTESIAN_POINT('Ctrl Pts',(-11.9267134419172,-35.9720068128318,
-2.46022991528048));
#37495=CARTESIAN_POINT('Ctrl Pts',(-11.8628155407781,-35.9831541197211,
-2.73716234364608));
#37496=CARTESIAN_POINT('Ctrl Pts',(-11.7989284926723,-35.9942995332446,
-3.01404773514772));
#37497=CARTESIAN_POINT('Ctrl Pts',(-11.7253363480305,-36.0054449467682,
-3.28872510056579));
#37498=CARTESIAN_POINT('Ctrl Pts',(-11.6422175183502,-36.0165903602918,
-3.56050860207074));
#37499=CARTESIAN_POINT('Ctrl Pts',(-11.559107916142,-36.0277345365026,-3.8322619314151));
#37500=CARTESIAN_POINT('Ctrl Pts',(-11.466473818764,-36.0388787127133,-4.10112178333928));
#37501=CARTESIAN_POINT('Ctrl Pts',(-11.3645435686143,-36.0500228889241,
-4.36641726442477));
#37502=CARTESIAN_POINT('Ctrl Pts',(-11.2594033383302,-36.0615180167336,
-4.64006741179234));
#37503=CARTESIAN_POINT('Ctrl Pts',(-11.1443720573033,-36.0730131445432,
-4.90992477220224));
#37504=CARTESIAN_POINT('Ctrl Pts',(-11.0197546303388,-36.0845082723527,
-5.17527372581657));
#37505=CARTESIAN_POINT('Ctrl Pts',(-10.8989353748965,-36.0956530441313,
-5.43253520030673));
#37506=CARTESIAN_POINT('Ctrl Pts',(-10.7691057848687,-36.1067978159099,
-5.68555876622977));
#37507=CARTESIAN_POINT('Ctrl Pts',(-10.6305916042168,-36.1179425876886,
-5.93371488987754));
#37508=CARTESIAN_POINT('Ctrl Pts',(-10.4855457583789,-36.1296128935136,
-6.19357286748642));
#37509=CARTESIAN_POINT('Ctrl Pts',(-10.3309767217692,-36.1412831993385,
-6.44809302920758));
#37510=CARTESIAN_POINT('Ctrl Pts',(-10.1673116861847,-36.1529535051635,
-6.69658295894055));
#37511=CARTESIAN_POINT('Ctrl Pts',(-10.0036466506002,-36.1646238109885,
-6.9450728886735));
#37512=CARTESIAN_POINT('Ctrl Pts',(-9.83088580791383,-36.1762941168134,
-7.18753231105948));
#37513=CARTESIAN_POINT('Ctrl Pts',(-9.64950806513854,-36.1879644226384,
-7.42330413972284));
#37514=CARTESIAN_POINT('Ctrl Pts',(-9.47625871296853,-36.199111727114,-7.6485099226974));
#37515=CARTESIAN_POINT('Ctrl Pts',(-9.29509606919364,-36.2102590315895,
-7.8676816020831));
#37516=CARTESIAN_POINT('Ctrl Pts',(-9.10646565514324,-36.221406336065,-8.0802681590215));
#37517=CARTESIAN_POINT('Ctrl Pts',(-8.91786728005395,-36.2325517471659,
-8.2928186080371));
#37518=CARTESIAN_POINT('Ctrl Pts',(-8.72180384403198,-36.2436971582667,
-8.49878596821237));
#37519=CARTESIAN_POINT('Ctrl Pts',(-8.51876020628826,-36.2548425693675,
-8.69765340754388));
#37520=CARTESIAN_POINT('Ctrl Pts',(-8.31573910957317,-36.2659867431529,
-8.89649876947028));
#37521=CARTESIAN_POINT('Ctrl Pts',(-8.10573954903184,-36.2771309169383,
-9.08824559786713));
#37522=CARTESIAN_POINT('Ctrl Pts',(-7.88928307487955,-36.2882750907237,
-9.27241407694993));
#37523=CARTESIAN_POINT('Ctrl Pts',(-7.66600988509742,-36.2997702203486,
-9.46238244792694));
#37524=CARTESIAN_POINT('Ctrl Pts',(-7.43586672490532,-36.3112653499736,
-9.64428721563409));
#37525=CARTESIAN_POINT('Ctrl Pts',(-7.19946377540692,-36.3227604795986,
-9.81764592947839));
#37526=CARTESIAN_POINT('Ctrl Pts',(-6.97026615536178,-36.3339052489754,
-9.98572084018279));
#37527=CARTESIAN_POINT('Ctrl Pts',(-6.73518490496334,-36.3450500183522,
-10.1457627683423));
#37528=CARTESIAN_POINT('Ctrl Pts',(-6.49480730688629,-36.3561947877291,
-10.2973748254794));
#37529=CARTESIAN_POINT('Ctrl Pts',(-6.24309451396523,-36.3678650974781,
-10.4561362685081));
#37530=CARTESIAN_POINT('Ctrl Pts',(-5.98557411618706,-36.3795354072272,
-10.6056535064113));
#37531=CARTESIAN_POINT('Ctrl Pts',(-5.7229525669938,-36.3912057169763,-10.7455229824304));
#37532=CARTESIAN_POINT('Ctrl Pts',(-5.46033101780052,-36.4028760267254,
-10.8853924584494));
#37533=CARTESIAN_POINT('Ctrl Pts',(-5.19260861744099,-36.4145463364744,
-11.0156140226206));
#37534=CARTESIAN_POINT('Ctrl Pts',(-4.9205203219068,-36.4262166462235,-11.1358398880238));
#37535=CARTESIAN_POINT('Ctrl Pts',(-4.66062554473769,-36.4373639561281,
-11.2506778836736));
#37536=CARTESIAN_POINT('Ctrl Pts',(-4.39666996201338,-36.4485112660327,
-11.3564306914372));
#37537=CARTESIAN_POINT('Ctrl Pts',(-4.12930845682457,-36.4596585759373,
-11.4528276822101));
#37538=CARTESIAN_POINT('Ctrl Pts',(-3.86199236269481,-36.4708039924835,
-11.5492083000596));
#37539=CARTESIAN_POINT('Ctrl Pts',(-3.59127175189979,-36.4819494090297,
-11.6362361830668));
#37540=CARTESIAN_POINT('Ctrl Pts',(-3.31781968883708,-36.4930948255759,
-11.7136895452443));
#37541=CARTESIAN_POINT('Ctrl Pts',(-3.04439798317911,-36.5042390048086,
-11.7911343089017));
#37542=CARTESIAN_POINT('Ctrl Pts',(-2.76824568734694,-36.5153831840413,
-11.8590066015354));
#37543=CARTESIAN_POINT('Ctrl Pts',(-2.49005036894981,-36.526527363274,-11.9171346979923));
#37544=CARTESIAN_POINT('Ctrl Pts',(-2.20309427787332,-36.5380224888186,
-11.9770933322249));
#37545=CARTESIAN_POINT('Ctrl Pts',(-1.91396469214712,-36.5495176143631,
-12.0266840376984));
#37546=CARTESIAN_POINT('Ctrl Pts',(-1.62342826198514,-36.5610127399077,
-12.065775189692));
#37547=CARTESIAN_POINT('Ctrl Pts',(-1.34174686044864,-36.5721575146694,
-12.1036749135756));
#37548=CARTESIAN_POINT('Ctrl Pts',(-1.05874337738828,-36.5833022894311,
-12.1317055846882));
#37549=CARTESIAN_POINT('Ctrl Pts',(-0.775123413472737,-36.5944470641928,
-12.149799749127));
#37550=CARTESIAN_POINT('Ctrl Pts',(-0.478129494697926,-36.6061173651288,
-12.1687471346687));
#37551=CARTESIAN_POINT('Ctrl Pts',(-0.180459873677726,-36.6177876660647,
-12.1767983435379));
#37552=CARTESIAN_POINT('Ctrl Pts',(0.11707202117144,-36.6294579670007,-12.1739370949524));
#37553=CARTESIAN_POINT('Ctrl Pts',(0.414603916020578,-36.6411282679367,
-12.1710758463669));
#37554=CARTESIAN_POINT('Ctrl Pts',(0.711997749299544,-36.6527985688726,
-12.1573021523303));
#37555=CARTESIAN_POINT('Ctrl Pts',(1.00844175372276,-36.6644688698086,-12.1326623409435));
#37556=CARTESIAN_POINT('Ctrl Pts',(1.29160072405077,-36.6756161703009,-12.1091267540628));
#37557=CARTESIAN_POINT('Ctrl Pts',(1.57397769503675,-36.6867634707932,-12.0756705357027));
#37558=CARTESIAN_POINT('Ctrl Pts',(1.85486813075634,-36.6979107712855,-12.0323694452716));
#37559=CARTESIAN_POINT('Ctrl Pts',(2.13571085696984,-36.7090561783983,-11.9890757095716));
#37560=CARTESIAN_POINT('Ctrl Pts',(2.41506728847831,-36.720201585511,-11.9359404808946));
#37561=CARTESIAN_POINT('Ctrl Pts',(2.69224029849889,-36.7313469926238,-11.8730911065796));
#37562=CARTESIAN_POINT('Ctrl Pts',(2.96938253809598,-36.7424911624267,-11.8102487095019));
#37563=CARTESIAN_POINT('Ctrl Pts',(3.24434158014842,-36.7536353322296,-11.7376943791884));
#37564=CARTESIAN_POINT('Ctrl Pts',(3.51643151935759,-36.7647795020325,-11.655606360017));
#37565=CARTESIAN_POINT('Ctrl Pts',(3.79709037410433,-36.776274634646,-11.5709331467551));
#37566=CARTESIAN_POINT('Ctrl Pts',(4.07469619766536,-36.7877697672594,-11.4761161021925));
#37567=CARTESIAN_POINT('Ctrl Pts',(4.34851283179752,-36.7992648998728,-11.3714065269734));
#37568=CARTESIAN_POINT('Ctrl Pts',(4.61398364177174,-36.8104096653299,-11.2698884587465));
#37569=CARTESIAN_POINT('Ctrl Pts',(4.87589256715123,-36.821554430787,-11.159072070423));
#37570=CARTESIAN_POINT('Ctrl Pts',(5.13358776672708,-36.8326991962441,-11.039235792903));
#37571=CARTESIAN_POINT('Ctrl Pts',(5.40343503015256,-36.8443695124357,-10.9137484279808));
#37572=CARTESIAN_POINT('Ctrl Pts',(5.66866130576691,-36.8560398286273,-10.7783701409865));
#37573=CARTESIAN_POINT('Ctrl Pts',(5.92854455678638,-36.8677101448189,-10.6334758986983));
#37574=CARTESIAN_POINT('Ctrl Pts',(6.18842780780583,-36.8793804610105,-10.4885816564102));
#37575=CARTESIAN_POINT('Ctrl Pts',(6.4429677454689,-36.8910507772021,-10.3341716298738));
#37576=CARTESIAN_POINT('Ctrl Pts',(6.69147375292597,-36.9027210933937,-10.1706749659943));
#37577=CARTESIAN_POINT('Ctrl Pts',(6.93796703319707,-36.9142968880769,-10.008502512276));
#37578=CARTESIAN_POINT('Ctrl Pts',(7.17860021783118,-36.9258726827601,-9.83733979174084));
#37579=CARTESIAN_POINT('Ctrl Pts',(7.41272179941099,-36.9374484774433,-9.65763976210219));
#37580=CARTESIAN_POINT('',(-12.1744999990795,-35.6251260039956,-0.000149711562892353));
#37581=CARTESIAN_POINT('Ctrl Pts',(-12.1744999990795,-35.6251260039956,
-0.000149711562934393));
#37582=CARTESIAN_POINT('Ctrl Pts',(-12.174496426179,-35.6365176701443,-0.290696921273105));
#37583=CARTESIAN_POINT('Ctrl Pts',(-12.1640875501384,-35.647909336293,-0.58120652559487));
#37584=CARTESIAN_POINT('Ctrl Pts',(-12.1433074390434,-35.6593010024416,
-0.870938970808622));
#37585=CARTESIAN_POINT('Ctrl Pts',(-12.1225204619165,-35.670696432552,-1.16076714756995));
#37586=CARTESIAN_POINT('Ctrl Pts',(-12.0913554174435,-35.6820918626624,
-1.44981741179922));
#37587=CARTESIAN_POINT('Ctrl Pts',(-12.0498983619847,-35.6934872927729,
-1.73735422865857));
#37588=CARTESIAN_POINT('Ctrl Pts',(-12.0121118806754,-35.7038737807208,
-1.99943276838512));
#37589=CARTESIAN_POINT('Ctrl Pts',(-11.9657758328564,-35.7142602686687,
-2.26025391982292));
#37590=CARTESIAN_POINT('Ctrl Pts',(-11.9109926366114,-35.7246467566166,
-2.51926669104116));
#37591=CARTESIAN_POINT('Ctrl Pts',(-11.8521965285982,-35.7357940628915,
-2.79725234936639));
#37592=CARTESIAN_POINT('Ctrl Pts',(-11.783655703664,-35.7469413691664,-3.0732202996823));
#37593=CARTESIAN_POINT('Ctrl Pts',(-11.7055335188614,-35.7580886754414,
-3.34648103069664));
#37594=CARTESIAN_POINT('Ctrl Pts',(-11.6274246031012,-35.7692340883479,
-3.61969534841323));
#37595=CARTESIAN_POINT('Ctrl Pts',(-11.5397376498562,-35.7803795012544,
-3.89020310848564));
#37596=CARTESIAN_POINT('Ctrl Pts',(-11.4426862708534,-35.7915249141608,
-4.15732860823185));
#37597=CARTESIAN_POINT('Ctrl Pts',(-11.3456456660616,-35.8026690897533,
-4.42442445289702));
#37598=CARTESIAN_POINT('Ctrl Pts',(-11.2392428024865,-35.8138132653458,
-4.68813853636811));
#37599=CARTESIAN_POINT('Ctrl Pts',(-11.1237403838462,-35.8249574409383,
-4.94781266043789));
#37600=CARTESIAN_POINT('Ctrl Pts',(-11.004600559911,-35.8364525692102,-5.21566444905335));
#37601=CARTESIAN_POINT('Ctrl Pts',(-10.8757788785789,-35.8479476974822,
-5.47921742693672));
#37602=CARTESIAN_POINT('Ctrl Pts',(-10.7376168148967,-35.8594428257542,
-5.73777268514943));
#37603=CARTESIAN_POINT('Ctrl Pts',(-10.6036657578032,-35.8705875969194,
-5.98844750305287));
#37604=CARTESIAN_POINT('Ctrl Pts',(-10.4609353850308,-35.8817323680846,
-6.23442449239448));
#37605=CARTESIAN_POINT('Ctrl Pts',(-10.30978353461,-35.8928771392499,-6.47509179235978));
#37606=CARTESIAN_POINT('Ctrl Pts',(-10.1515040647607,-35.9045474460752,
-6.72710784471055));
#37607=CARTESIAN_POINT('Ctrl Pts',(-9.98398994001832,-35.9162177529005,
-6.97330112872041));
#37608=CARTESIAN_POINT('Ctrl Pts',(-9.80770356017696,-35.9278880597258,
-7.21300222692966));
#37609=CARTESIAN_POINT('Ctrl Pts',(-9.63141718033562,-35.9395583665511,
-7.45270332513889));
#37610=CARTESIAN_POINT('Ctrl Pts',(-9.4463587512404,-35.9512286733765,-7.68591197247079));
#37611=CARTESIAN_POINT('Ctrl Pts',(-9.25304049328369,-35.9628989802018,
-7.91199670624631));
#37612=CARTESIAN_POINT('Ctrl Pts',(-9.06838572400005,-35.9740462863956,
-8.12794953343979));
#37613=CARTESIAN_POINT('Ctrl Pts',(-8.87614002640509,-35.9851935925894,
-8.33746742022859));
#37614=CARTESIAN_POINT('Ctrl Pts',(-8.67677679908099,-35.9963408987832,
-8.54002310470703));
#37615=CARTESIAN_POINT('Ctrl Pts',(-8.47744743357855,-36.0074863116083,
-8.74254438512533));
#37616=CARTESIAN_POINT('Ctrl Pts',(-8.27100313898243,-36.0186317244334,
-8.93810563411376));
#37617=CARTESIAN_POINT('Ctrl Pts',(-8.05795483269958,-36.0297771372585,
-9.1262157636215));
#37618=CARTESIAN_POINT('Ctrl Pts',(-7.84493017808824,-36.0409213127697,
-9.31430500998273));
#37619=CARTESIAN_POINT('Ctrl Pts',(-7.62530317567703,-36.0520654882808,
-9.49494461212312));
#37620=CARTESIAN_POINT('Ctrl Pts',(-7.39961947215846,-36.063209663792,-9.66768234466014));
#37621=CARTESIAN_POINT('Ctrl Pts',(-7.16682852840535,-36.0747047921249,
-9.84585994079197));
#37622=CARTESIAN_POINT('Ctrl Pts',(-6.9275934559246,-36.0861999204578,-10.0156297224767));
#37623=CARTESIAN_POINT('Ctrl Pts',(-6.68254854954543,-36.0976950487907,
-10.1765414131211));
#37624=CARTESIAN_POINT('Ctrl Pts',(-6.44497230785367,-36.1088398198755,
-10.3325487150986));
#37625=CARTESIAN_POINT('Ctrl Pts',(-6.2019353743058,-36.1199845909603,-10.4802297442823));
#37626=CARTESIAN_POINT('Ctrl Pts',(-5.95404475521485,-36.1311293620451,
-10.6192184883304));
#37627=CARTESIAN_POINT('Ctrl Pts',(-5.69446476074719,-36.1427996690021,
-10.7647612988788));
#37628=CARTESIAN_POINT('Ctrl Pts',(-5.429562588848,-36.154469975959,-10.9007721676023));
#37629=CARTESIAN_POINT('Ctrl Pts',(-5.16006460113188,-36.166140282916,-11.0268845809751));
#37630=CARTESIAN_POINT('Ctrl Pts',(-4.89056661341578,-36.1778105898729,
-11.1529969943479));
#37631=CARTESIAN_POINT('Ctrl Pts',(-4.61647311747857,-36.1894808968299,
-11.2692108181213));
#37632=CARTESIAN_POINT('Ctrl Pts',(-4.33853605764074,-36.2011512037868,
-11.3752167067951));
#37633=CARTESIAN_POINT('Ctrl Pts',(-4.07305464777408,-36.2122985101097,
-11.4764719794663));
#37634=CARTESIAN_POINT('Ctrl Pts',(-3.80398730860846,-36.2234458164327,
-11.5684443772484));
#37635=CARTESIAN_POINT('Ctrl Pts',(-3.53200203188287,-36.2345931227556,
-11.6508974717305));
#37636=CARTESIAN_POINT('Ctrl Pts',(-3.26006295181857,-36.2457385357101,
-11.7333365615659));
#37637=CARTESIAN_POINT('Ctrl Pts',(-2.98520717886023,-36.2568839486646,
-11.8062594987885));
#37638=CARTESIAN_POINT('Ctrl Pts',(-2.70811833795219,-36.2680293616191,
-11.8694795723169));
#37639=CARTESIAN_POINT('Ctrl Pts',(-2.43106025821149,-36.2791735372596,
-11.9326926274346));
#37640=CARTESIAN_POINT('Ctrl Pts',(-2.1517698655459,-36.2903177129001,-11.9862049104721));
#37641=CARTESIAN_POINT('Ctrl Pts',(-1.87094268199846,-36.3014618885405,
-12.0298804537151));
#37642=CARTESIAN_POINT('Ctrl Pts',(-1.5812716833385,-36.3129570167765,-12.0749314280132));
#37643=CARTESIAN_POINT('Ctrl Pts',(-1.28996582371931,-36.3244521450124,
-12.1095160101662));
#37644=CARTESIAN_POINT('Ctrl Pts',(-0.997797531322615,-36.3359472732484,
-12.1335423655455));
#37645=CARTESIAN_POINT('Ctrl Pts',(-0.714534160316956,-36.3470920444607,
-12.1568364278884));
#37646=CARTESIAN_POINT('Ctrl Pts',(-0.430460427915619,-36.358236815673,
-12.1702063130348));
#37647=CARTESIAN_POINT('Ctrl Pts',(-0.146284477231075,-36.3693815868853,
-12.1736211170597));
#37648=CARTESIAN_POINT('Ctrl Pts',(0.151291888549954,-36.3810518936331,
-12.1771969473476));
#37649=CARTESIAN_POINT('Ctrl Pts',(0.448980027019182,-36.3927222003809,
-12.169856231212));
#37650=CARTESIAN_POINT('Ctrl Pts',(0.745966753667841,-36.4043925071286,
-12.1516247412608));
#37651=CARTESIAN_POINT('Ctrl Pts',(1.04295348031647,-36.4160628138764,-12.1333932513097));
#37652=CARTESIAN_POINT('Ctrl Pts',(1.33923846081193,-36.4277331206241,-12.1042710168617));
#37653=CARTESIAN_POINT('Ctrl Pts',(1.63401340472503,-36.4394034273719,-12.0643462501363));
#37654=CARTESIAN_POINT('Ctrl Pts',(1.91557811671966,-36.4505507335666,-12.0262106973134));
#37655=CARTESIAN_POINT('Ctrl Pts',(2.19584925314808,-36.4616980397613,-11.9782081635445));
#37656=CARTESIAN_POINT('Ctrl Pts',(2.47412713324821,-36.4728453459559,-11.9204507120547));
#37657=CARTESIAN_POINT('Ctrl Pts',(2.75235774788912,-36.4839907587822,-11.8627030706599));
#37658=CARTESIAN_POINT('Ctrl Pts',(3.02859552104343,-36.4951361716085,-11.7952038736759));
#37659=CARTESIAN_POINT('Ctrl Pts',(3.30215083685498,-36.5062815844348,-11.7181163204953));
#37660=CARTESIAN_POINT('Ctrl Pts',(3.57567578378372,-36.5174257599474,-11.6410373252286));
#37661=CARTESIAN_POINT('Ctrl Pts',(3.84651861133585,-36.52856993546,-11.5543721716479));
#37662=CARTESIAN_POINT('Ctrl Pts',(4.11400354010584,-36.5397141109726,-11.4583343083538));
#37663=CARTESIAN_POINT('Ctrl Pts',(4.38991211491443,-36.5512092393046,-11.3592720168407));
#37664=CARTESIAN_POINT('Ctrl Pts',(4.66224758709874,-36.5627043676366,-11.250237209273));
#37665=CARTESIAN_POINT('Ctrl Pts',(4.93028776824498,-36.5741994959687,-11.1315188888262));
#37666=CARTESIAN_POINT('Ctrl Pts',(5.19015841733053,-36.5853442670556,-11.0164189554471));
#37667=CARTESIAN_POINT('Ctrl Pts',(5.44599147331901,-36.5964890381425,-10.8922171642219));
#37668=CARTESIAN_POINT('Ctrl Pts',(5.69715035220492,-36.6076338092294,-10.7592252562334));
#37669=CARTESIAN_POINT('Ctrl Pts',(5.96015272238509,-36.619304116184,-10.6199620648587));
#37670=CARTESIAN_POINT('Ctrl Pts',(6.21802920235262,-36.6309744231386,-10.4710599556509));
#37671=CARTESIAN_POINT('Ctrl Pts',(6.47007809708769,-36.6426447300932,-10.3129307021615));
#37672=CARTESIAN_POINT('Ctrl Pts',(6.72212699182275,-36.6543150370478,-10.1548014486722));
#37673=CARTESIAN_POINT('Ctrl Pts',(6.96834802179005,-36.6659853440024,-9.98744523663738));
#37674=CARTESIAN_POINT('Ctrl Pts',(7.20807366931145,-36.677655650957,-9.81132632358027));
#37675=CARTESIAN_POINT('Ctrl Pts',(7.27682267471017,-36.6810024851574,-9.76081858596533));
#37676=CARTESIAN_POINT('Ctrl Pts',(7.34504387489234,-36.6843493193577,-9.70958595586962));
#37677=CARTESIAN_POINT('Ctrl Pts',(7.41272179941099,-36.6876961535581,-9.65763976210219));
#37678=CARTESIAN_POINT('Ctrl Pts',(7.412721799411,-33.6876951030527,-9.65763976210218));
#37679=CARTESIAN_POINT('Ctrl Pts',(7.63818831033701,-33.6988400412174,-9.48458293230233));
#37680=CARTESIAN_POINT('Ctrl Pts',(7.85759515882196,-33.7099849793821,-9.30362458373371));
#37681=CARTESIAN_POINT('Ctrl Pts',(8.07039566856871,-33.7211299175467,-9.11521606999788));
#37682=CARTESIAN_POINT('Ctrl Pts',(8.28319341563403,-33.7322747110223,-8.92681000227451));
#37683=CARTESIAN_POINT('Ctrl Pts',(8.48938479699339,-33.7434195044979,-8.73095414112008));
#37684=CARTESIAN_POINT('Ctrl Pts',(8.68845788705469,-33.7545642979734,-8.52813870635775));
#37685=CARTESIAN_POINT('Ctrl Pts',(8.88757719156055,-33.7657116786919,-8.32527618837254));
#37686=CARTESIAN_POINT('Ctrl Pts',(9.079574714239,-33.7768590594104,-8.11545105737663));
#37687=CARTESIAN_POINT('Ctrl Pts',(9.26397579995409,-33.7880064401288,-7.8991899982128));
#37688=CARTESIAN_POINT('Ctrl Pts',(9.43282943823787,-33.7982139493978,-7.70116260310658));
#37689=CARTESIAN_POINT('Ctrl Pts',(9.59531392857967,-33.8084214586668,-7.49773932359984));
#37690=CARTESIAN_POINT('Ctrl Pts',(9.75109440402036,-33.8186289679358,-7.28934895404814));
#37691=CARTESIAN_POINT('Ctrl Pts',(9.92121745963441,-33.8297762741829,-7.06177225466792));
#37692=CARTESIAN_POINT('Ctrl Pts',(10.0833954685513,-33.8409235804299,-6.82820331985483));
#37693=CARTESIAN_POINT('Ctrl Pts',(10.2372180184084,-33.852070886677,-6.58921979399485));
#37694=CARTESIAN_POINT('Ctrl Pts',(10.3910144415251,-33.8632162995555,-6.35027685945625));
#37695=CARTESIAN_POINT('Ctrl Pts',(10.5364580946448,-33.874361712434,-6.10592139420259));
#37696=CARTESIAN_POINT('Ctrl Pts',(10.6731820964192,-33.8855071253125,-5.85675970026745));
#37697=CARTESIAN_POINT('Ctrl Pts',(10.8098909197055,-33.8966513008771,-5.60762566715101));
#37698=CARTESIAN_POINT('Ctrl Pts',(10.9378818963315,-33.9077954764416,-5.35368670459258));
#37699=CARTESIAN_POINT('Ctrl Pts',(11.0568336864415,-33.9189396520062,-5.09557446029123));
#37700=CARTESIAN_POINT('Ctrl Pts',(11.1795315100773,-33.9304347802991,-4.82933373705164));
#37701=CARTESIAN_POINT('Ctrl Pts',(11.2926114639303,-33.941929908592,-4.55865288790692));
#37702=CARTESIAN_POINT('Ctrl Pts',(11.3957735795932,-33.9534250368849,-4.28424961605236));
#37703=CARTESIAN_POINT('Ctrl Pts',(11.4957914427987,-33.9645698080224,-4.01820981325164));
#37704=CARTESIAN_POINT('Ctrl Pts',(11.5864869838508,-33.97571457916,-3.74867139848463));
#37705=CARTESIAN_POINT('Ctrl Pts',(11.6676364475165,-33.9868593502975,-3.47630694539264));
#37706=CARTESIAN_POINT('Ctrl Pts',(11.7526125436312,-33.9985296571681,-3.19109904753701));
#37707=CARTESIAN_POINT('Ctrl Pts',(11.8271205113252,-34.0101999640387,-2.90279247716342));
#37708=CARTESIAN_POINT('Ctrl Pts',(11.8909623210325,-34.0218702709092,-2.61217635885952));
#37709=CARTESIAN_POINT('Ctrl Pts',(11.9548041307399,-34.0335405777798,-2.32156024055564));
#37710=CARTESIAN_POINT('Ctrl Pts',(12.0079797190489,-34.0452108846504,-2.02863490389215));
#37711=CARTESIAN_POINT('Ctrl Pts',(12.0503524473524,-34.056881191521,-1.73420187538456));
#37712=CARTESIAN_POINT('Ctrl Pts',(12.0908262570107,-34.0680284977683,-1.45296375761318));
#37713=CARTESIAN_POINT('Ctrl Pts',(12.1214562644126,-34.0791758040156,-1.17026611606645));
#37714=CARTESIAN_POINT('Ctrl Pts',(12.142158528628,-34.0903231102629,-0.886812559488088));
#37715=CARTESIAN_POINT('Ctrl Pts',(12.1628572765665,-34.1014685231416,-0.603407147460176));
#37716=CARTESIAN_POINT('Ctrl Pts',(12.1736316284451,-34.1126139360204,-0.319246342673114));
#37717=CARTESIAN_POINT('Ctrl Pts',(12.1744495802706,-34.1237593488991,-0.0350380856780686));
#37718=CARTESIAN_POINT('Ctrl Pts',(12.1752674412908,-34.1349035244639,0.249138619785386));
#37719=CARTESIAN_POINT('Ctrl Pts',(12.1661311086289,-34.1460477000287,0.533362500259884));
#37720=CARTESIAN_POINT('Ctrl Pts',(12.1470606956327,-34.1571918755935,0.816925153619469));
#37721=CARTESIAN_POINT('Ctrl Pts',(12.1273897165896,-34.1686870038862,1.10941777099075));
#37722=CARTESIAN_POINT('Ctrl Pts',(12.0971488397799,-34.1801821321789,1.40120654292002));
#37723=CARTESIAN_POINT('Ctrl Pts',(12.0564181252866,-34.1916772604716,1.69151773217481));
#37724=CARTESIAN_POINT('Ctrl Pts',(12.0169288321053,-34.2028220316094,1.97298059892988));
#37725=CARTESIAN_POINT('Ctrl Pts',(11.9675797055986,-34.2139668027472,2.25305434264466));
#37726=CARTESIAN_POINT('Ctrl Pts',(11.9084961294965,-34.225111573885,2.53104132399424));
#37727=CARTESIAN_POINT('Ctrl Pts',(11.8466264458957,-34.2367818807552,2.82213688245413));
#37728=CARTESIAN_POINT('Ctrl Pts',(11.7740822255187,-34.2484521876253,3.11094382810151));
#37729=CARTESIAN_POINT('Ctrl Pts',(11.6910672154904,-34.2601224944955,3.39667449321921));
#37730=CARTESIAN_POINT('Ctrl Pts',(11.608052205462,-34.2717928013657,3.68240515833693));
#37731=CARTESIAN_POINT('Ctrl Pts',(11.5145665078164,-34.2834631082358,3.96505922319547));
#37732=CARTESIAN_POINT('Ctrl Pts',(11.4108737097382,-34.295133415106,4.24386750858299));
#37733=CARTESIAN_POINT('Ctrl Pts',(11.3118278672755,-34.3062807213527,4.51018110049645));
#37734=CARTESIAN_POINT('Ctrl Pts',(11.2034400892115,-34.3174280275994,4.77306556836597));
#37735=CARTESIAN_POINT('Ctrl Pts',(11.0859733768434,-34.3285753338461,5.03186292916634));
#37736=CARTESIAN_POINT('Ctrl Pts',(10.9685266161816,-34.3397207467242,5.29061633326782));
#37737=CARTESIAN_POINT('Ctrl Pts',(10.8420041101378,-34.3508661596023,5.54528377345437));
#37738=CARTESIAN_POINT('Ctrl Pts',(10.7067165369335,-34.3620115724805,5.79522831713764));
#37739=CARTESIAN_POINT('Ctrl Pts',(10.5714439827516,-34.3731557480446,6.04514511309366));
#37740=CARTESIAN_POINT('Ctrl Pts',(10.4274084313955,-34.3842999236088,6.29033982499244));
#37741=CARTESIAN_POINT('Ctrl Pts',(10.2749665443453,-34.395444099173,6.53020005532642));
#37742=CARTESIAN_POINT('Ctrl Pts',(10.117723952571,-34.4069392274662,6.77761397161364));
#37743=CARTESIAN_POINT('Ctrl Pts',(9.95153713121388,-34.4184343557593,7.01935171891168));
#37744=CARTESIAN_POINT('Ctrl Pts',(9.77684664447996,-34.4299294840525,7.25477221836227));
#37745=CARTESIAN_POINT('Ctrl Pts',(9.60748050563951,-34.4410742551897,7.48301739496749));
#37746=CARTESIAN_POINT('Ctrl Pts',(9.43012155403504,-34.4522190263269,7.7053244809599));
#37747=CARTESIAN_POINT('Ctrl Pts',(9.24521373484962,-34.4633637974641,7.92114090563651));
#37748=CARTESIAN_POINT('Ctrl Pts',(9.05158652023803,-34.4750341043353,8.14713423226626));
#37749=CARTESIAN_POINT('Ctrl Pts',(8.84968157512732,-34.4867044112064,8.36600978804986));
#37750=CARTESIAN_POINT('Ctrl Pts',(8.64005473522879,-34.4983747180776,8.5771734517993));
#37751=CARTESIAN_POINT('Ctrl Pts',(8.43042789533026,-34.5100450249488,8.78833711554873));
#37752=CARTESIAN_POINT('Ctrl Pts',(8.21307940324054,-34.52171533182,8.99178865534857));
#37753=CARTESIAN_POINT('Ctrl Pts',(7.98860879055077,-34.5333856386912,9.18697882013097));
#37754=CARTESIAN_POINT('Ctrl Pts',(7.77419774798598,-34.5445329449391,9.37342160757606));
#37755=CARTESIAN_POINT('Ctrl Pts',(7.55322486774204,-34.5556802511869,9.55238288856828));
#37756=CARTESIAN_POINT('Ctrl Pts',(7.32623595483955,-34.5668275574348,9.72341076906742));
#37757=CARTESIAN_POINT('Ctrl Pts',(7.09928559597489,-34.5779729703142,9.89440960050293));
#37758=CARTESIAN_POINT('Ctrl Pts',(6.8663214574821,-34.5891183831935,10.0574775612436));
#37759=CARTESIAN_POINT('Ctrl Pts',(6.62792113425293,-34.6002637960728,10.21220405633));
#37760=CARTESIAN_POINT('Ctrl Pts',(6.38954727716309,-34.6114079716382,10.3669133743719));
#37761=CARTESIAN_POINT('Ctrl Pts',(6.14573866412767,-34.6225521472036,10.5132829307161));
#37762=CARTESIAN_POINT('Ctrl Pts',(5.89710152521148,-34.6336963227689,10.6509456787343));
#37763=CARTESIAN_POINT('Ctrl Pts',(5.64063429770763,-34.6451914510612,10.7929437063366));
#37764=CARTESIAN_POINT('Ctrl Pts',(5.37902975093787,-34.6566865793535,10.9256774968982));
#37765=CARTESIAN_POINT('Ctrl Pts',(5.11298151220427,-34.6681817076457,11.0487949707585));
#37766=CARTESIAN_POINT('Ctrl Pts',(4.85504209151592,-34.6793264787841,11.1681599777786));
#37767=CARTESIAN_POINT('Ctrl Pts',(4.59292609736638,-34.6904712499225,11.2784860573086));
#37768=CARTESIAN_POINT('Ctrl Pts',(4.32728777084149,-34.7016160210608,11.3795004634793));
#37769=CARTESIAN_POINT('Ctrl Pts',(4.04912317254769,-34.71328632793,11.4852782406621));
#37770=CARTESIAN_POINT('Ctrl Pts',(3.76709635207613,-34.7249566347993,11.5808449099813));
#37771=CARTESIAN_POINT('Ctrl Pts',(3.48197968126964,-34.7366269416685,11.6659447859668));
#37772=CARTESIAN_POINT('Ctrl Pts',(3.19686301046314,-34.7482972485377,11.7510446619523));
#37773=CARTESIAN_POINT('Ctrl Pts',(2.9086568133186,-34.759967555407,11.8256776570603));
#37774=CARTESIAN_POINT('Ctrl Pts',(2.61815035720158,-34.7716378622762,11.8896483950151));
#37775=CARTESIAN_POINT('Ctrl Pts',(2.34066284388209,-34.7827851685224,11.950752307257));
#37776=CARTESIAN_POINT('Ctrl Pts',(2.06099383559946,-34.7939324747685,12.0021468563789));
#37777=CARTESIAN_POINT('Ctrl Pts',(1.77983883484186,-34.8050797810147,12.043696441375));
#37778=CARTESIAN_POINT('Ctrl Pts',(1.49873158822519,-34.8162251938923,12.0852389691794));
#37779=CARTESIAN_POINT('Ctrl Pts',(1.21613911682261,-34.8273706067699,12.1169398323548));
#37780=CARTESIAN_POINT('Ctrl Pts',(0.932765073298876,-34.8385160196475,
12.1387149059542));
#37781=CARTESIAN_POINT('Ctrl Pts',(0.649422488696312,-34.8496601952111,
12.160487562182));
#37782=CARTESIAN_POINT('Ctrl Pts',(0.365298771126767,-34.8608043707748,
12.1723366087547));
#37783=CARTESIAN_POINT('Ctrl Pts',(0.0811018770416422,-34.8719485463384,
12.174229862112));
#37784=CARTESIAN_POINT('Ctrl Pts',(-0.212044954636546,-34.883443674632,
12.1761827378641));
#37785=CARTESIAN_POINT('Ctrl Pts',(-0.505269349828249,-34.8949388029255,
12.1675425913307));
#37786=CARTESIAN_POINT('Ctrl Pts',(-0.797793774022385,-34.9064339312191,
12.1483322042217));
#37787=CARTESIAN_POINT('Ctrl Pts',(-1.08140241902979,-34.9175787023558,
12.1297073257247));
#37788=CARTESIAN_POINT('Ctrl Pts',(-1.36435285121784,-34.9287234734924,
12.1011470191103));
#37789=CARTESIAN_POINT('Ctrl Pts',(-1.64594008431267,-34.9398682446291,
12.0627248782708));
#37790=CARTESIAN_POINT('Ctrl Pts',(-1.94080566577381,-34.9515385515011,
12.022490927409));
#37791=CARTESIAN_POINT('Ctrl Pts',(-2.23417607541674,-34.9632088583732,
11.9714427292178));
#37792=CARTESIAN_POINT('Ctrl Pts',(-2.52525076469805,-34.9748791652452,
11.9097253883283));
#37793=CARTESIAN_POINT('Ctrl Pts',(-2.81632545397939,-34.9865494721172,
11.8480080474388));
#37794=CARTESIAN_POINT('Ctrl Pts',(-3.10510409651557,-34.9982197789893,
11.7756216420282));
#37795=CARTESIAN_POINT('Ctrl Pts',(-3.39080016893301,-35.0098900858613,
11.6927723173063));
#37796=CARTESIAN_POINT('Ctrl Pts',(-3.66369287414124,-35.0210373921087,
11.6136358554125));
#37797=CARTESIAN_POINT('Ctrl Pts',(-3.93385472728386,-35.0321846983561,
11.5249300100742));
#37798=CARTESIAN_POINT('Ctrl Pts',(-4.2006101415968,-35.0433320046035,11.4268685425323));
#37799=CARTESIAN_POINT('Ctrl Pts',(-4.46732024753662,-35.0544774174824,
11.3288237307182));
#37800=CARTESIAN_POINT('Ctrl Pts',(-4.73062481951651,-35.0656228303613,
11.2214265612428));
#37801=CARTESIAN_POINT('Ctrl Pts',(-4.98986574788565,-35.0767682432401,
11.1049398948431));
#37802=CARTESIAN_POINT('Ctrl Pts',(-5.24907789648447,-35.087912418805,10.988466160273));
#37803=CARTESIAN_POINT('Ctrl Pts',(-5.50422705905216,-35.0990565943699,
10.8629050530432));
#37804=CARTESIAN_POINT('Ctrl Pts',(-5.75467620310833,-35.1102007699348,
10.7285671013131));
#37805=CARTESIAN_POINT('Ctrl Pts',(-6.01301249949392,-35.1216958982274,
10.5899985745779));
#37806=CARTESIAN_POINT('Ctrl Pts',(-6.26634768811444,-35.1331910265201,
10.4420915758947));
#37807=CARTESIAN_POINT('Ctrl Pts',(-6.51400994570973,-35.1446861548127,
10.2852381925357));
#37808=CARTESIAN_POINT('Ctrl Pts',(-6.75412376698444,-35.1558309259506,
10.1331655044164));
#37809=CARTESIAN_POINT('Ctrl Pts',(-6.98890510846621,-35.1669756970884,
9.97268385469132));
#37810=CARTESIAN_POINT('Ctrl Pts',(-7.21777016470931,-35.1781204682263,
9.80419522956536));
#37811=CARTESIAN_POINT('Ctrl Pts',(-7.45742743583133,-35.1897907750963,
9.62776146210592));
#37812=CARTESIAN_POINT('Ctrl Pts',(-7.6905967708411,-35.2014610819663,9.44254759390732));
#37813=CARTESIAN_POINT('Ctrl Pts',(-7.91664467542025,-35.2131313888364,
9.24906413282664));
#37814=CARTESIAN_POINT('Ctrl Pts',(-8.14269257999939,-35.2248016957064,
9.05558067174598));
#37815=CARTESIAN_POINT('Ctrl Pts',(-8.36161880497333,-35.2364720025764,
8.85382784261634));
#37816=CARTESIAN_POINT('Ctrl Pts',(-8.57283138154773,-35.2481423094464,
8.64436303920366));
#37817=CARTESIAN_POINT('Ctrl Pts',(-8.7745785421954,-35.2592896156963,8.44428532588983));
#37818=CARTESIAN_POINT('Ctrl Pts',(-8.96934848056512,-35.2704369219463,
8.23711190810849));
#37819=CARTESIAN_POINT('Ctrl Pts',(-9.15665028193266,-35.2815842281962,
8.02335377908656));
#37820=CARTESIAN_POINT('Ctrl Pts',(-9.34392027011314,-35.2927296410776,
7.80963195685556));
#37821=CARTESIAN_POINT('Ctrl Pts',(-9.52372447804811,-35.303875053959,7.58932785684307));
#37822=CARTESIAN_POINT('Ctrl Pts',(-9.69561083324766,-35.3150204668404,
7.36298722124455));
#37823=CARTESIAN_POINT('Ctrl Pts',(-9.8674781063922,-35.3261646424078,7.13667171297192));
#37824=CARTESIAN_POINT('Ctrl Pts',(-10.0314291207498,-35.3373088179753,
6.90432121967417));
#37825=CARTESIAN_POINT('Ctrl Pts',(-10.1870531218382,-35.3484529935428,
6.66651325228162));
#37826=CARTESIAN_POINT('Ctrl Pts',(-10.3475780388049,-35.3599481218335,
6.42121622899009));
#37827=CARTESIAN_POINT('Ctrl Pts',(-10.4992428040734,-35.3714432501243,
6.17011267067247));
#37828=CARTESIAN_POINT('Ctrl Pts',(-10.6416451441391,-35.382938378415,5.91386835127568));
#37829=CARTESIAN_POINT('Ctrl Pts',(-10.7797072387721,-35.3940831495554,
5.6654340386276));
#37830=CARTESIAN_POINT('Ctrl Pts',(-10.9090630261503,-35.4052279206958,
5.41216793644504));
#37831=CARTESIAN_POINT('Ctrl Pts',(-11.0293922551297,-35.4163726918363,
5.15470239029231));
#37832=CARTESIAN_POINT('Ctrl Pts',(-11.1553956525465,-35.4280429987021,
4.8850959629249));
#37833=CARTESIAN_POINT('Ctrl Pts',(-11.2715005718733,-35.439713305568,4.61088479720244));
#37834=CARTESIAN_POINT('Ctrl Pts',(-11.3773950641872,-35.4513836124339,
4.33282030592177));
#37835=CARTESIAN_POINT('Ctrl Pts',(-11.4832895565011,-35.4630539192998,
4.05475581464107));
#37836=CARTESIAN_POINT('Ctrl Pts',(-11.578973510603,-35.4747242261657,3.77283831446075));
#37837=CARTESIAN_POINT('Ctrl Pts',(-11.6641938765588,-35.4863945330316,
3.48784051528297));
#37838=CARTESIAN_POINT('Ctrl Pts',(-11.7486157263752,-35.4979554889427,
3.20551314986525));
#37839=CARTESIAN_POINT('Ctrl Pts',(-11.8227942500949,-35.5095164448538,
2.92007971671269));
#37840=CARTESIAN_POINT('Ctrl Pts',(-11.8865239621894,-35.521077400765,2.63229906095355));
#37841=CARTESIAN_POINT('Ctrl Pts',(-11.9482806334632,-35.5322804351166,
2.35342795401509));
#37842=CARTESIAN_POINT('Ctrl Pts',(-12.0002256656454,-35.5434834694682,
2.07235304358251));
#37843=CARTESIAN_POINT('Ctrl Pts',(-12.042223537602,-35.5546865038198,1.78977722647935));
#37844=CARTESIAN_POINT('Ctrl Pts',(-12.0862340710423,-35.5664264205107,
1.49365954554348));
#37845=CARTESIAN_POINT('Ctrl Pts',(-12.119320691996,-35.5781663372016,1.19589388457444));
#37846=CARTESIAN_POINT('Ctrl Pts',(-12.1413881016093,-35.5899062538925,
0.897298844366037));
#37847=CARTESIAN_POINT('Ctrl Pts',(-12.1634555112226,-35.6016461705834,
0.598703804157665));
#37848=CARTESIAN_POINT('Ctrl Pts',(-12.1745036811867,-35.6133860872742,
0.299279713519359));
#37849=CARTESIAN_POINT('Ctrl Pts',(-12.1744999990795,-35.6251260039651,
-0.00014971078451594));
#37850=CARTESIAN_POINT('Origin',(0.,-13.3748739960349,0.));
#37851=CARTESIAN_POINT('',(7.41272179941102,-30.6876856710377,-9.65763976210216));
#37852=CARTESIAN_POINT('',(7.41333450932786,-30.9374378643274,-9.65843860956001));
#37853=CARTESIAN_POINT('',(7.41272179941101,-13.3748739960349,-9.65763976210217));
#37854=CARTESIAN_POINT('',(-12.1744999985554,-32.8748739960349,0.000187550598588881));
#37855=CARTESIAN_POINT('Ctrl Pts',(7.41333450932841,-30.9374378643275,-9.65843860955958));
#37856=CARTESIAN_POINT('Ctrl Pts',(7.47386574430169,-30.9404304108071,-9.61201282177837));
#37857=CARTESIAN_POINT('Ctrl Pts',(9.12856187469929,-31.0228403651483,-8.31759967269045));
#37858=CARTESIAN_POINT('Ctrl Pts',(11.6976034309138,-31.1846677273513,-4.92316720896363));
#37859=CARTESIAN_POINT('Ctrl Pts',(12.6271934885173,-31.4229199509364,1.27494548820119));
#37860=CARTESIAN_POINT('Ctrl Pts',(10.4773717109103,-31.6611721745215,7.16213539565936));
#37861=CARTESIAN_POINT('Ctrl Pts',(5.77241822665602,-31.8994243981066,11.3026850443117));
#37862=CARTESIAN_POINT('Ctrl Pts',(-0.340263191846742,-32.1376766216917,
12.6868326368173));
#37863=CARTESIAN_POINT('Ctrl Pts',(-6.36996413642198,-32.3759288452768,
10.9770241092494));
#37864=CARTESIAN_POINT('Ctrl Pts',(-10.8462127664019,-32.6141810688619,
6.59023292610109));
#37865=CARTESIAN_POINT('Ctrl Pts',(-12.1244826930503,-32.7804961191146,
2.40607098746999));
#37866=CARTESIAN_POINT('Ctrl Pts',(-12.1754508005637,-32.8673937615056,
0.190879886591904));
#37867=CARTESIAN_POINT('Ctrl Pts',(-12.175309711376,-32.8748739960349,0.000187563072374733));
#37868=CARTESIAN_POINT('Ctrl Pts',(-12.1744999985554,-32.8748739960349,
0.000187550598588881));
#37869=CARTESIAN_POINT('Ctrl Pts',(-12.1745043615588,-32.8859843814439,
-0.283028740965722));
#37870=CARTESIAN_POINT('Ctrl Pts',(-12.1646216592697,-32.8970947668528,
-0.566289459754149));
#37871=CARTESIAN_POINT('Ctrl Pts',(-12.1448686657604,-32.9082051522618,
-0.848890653400877));
#37872=CARTESIAN_POINT('Ctrl Pts',(-12.125118898305,-32.9193137231254,-1.13144569269124));
#37873=CARTESIAN_POINT('Ctrl Pts',(-12.0955020767017,-32.930422293989,-1.4133411523803));
#37874=CARTESIAN_POINT('Ctrl Pts',(-12.0560869992745,-32.9415308648526,
-1.69387618081272));
#37875=CARTESIAN_POINT('Ctrl Pts',(-12.0166757019596,-32.9526383703461,
-1.97438430446705));
#37876=CARTESIAN_POINT('Ctrl Pts',(-11.9674680629165,-32.9637458758396,
-2.2535319898437));
#37877=CARTESIAN_POINT('Ctrl Pts',(-11.9085845275246,-32.9748533813331,
-2.5306253774118));
#37878=CARTESIAN_POINT('Ctrl Pts',(-11.849696245945,-32.9859617821245,-2.80774109952985));
#37879=CARTESIAN_POINT('Ctrl Pts',(-11.7811305632598,-32.9970701829159,
-3.08280192803896));
#37880=CARTESIAN_POINT('Ctrl Pts',(-11.703058959395,-33.0081785837073,-3.35512462405274));
#37881=CARTESIAN_POINT('Ctrl Pts',(-11.6249866141567,-33.0192870899849,
-3.62744990606199));
#37882=CARTESIAN_POINT('Ctrl Pts',(-11.5374082443903,-33.0303955962625,
-3.89703674452342));
#37883=CARTESIAN_POINT('Ctrl Pts',(-11.4405453455313,-33.0415041025401,
-4.16321659859816));
#37884=CARTESIAN_POINT('Ctrl Pts',(-11.3436617578851,-33.0526149814652,
-4.4294533055898));
#37885=CARTESIAN_POINT('Ctrl Pts',(-11.2374897710976,-33.0637258603903,
-4.6922813200952));
#37886=CARTESIAN_POINT('Ctrl Pts',(-11.1222997533272,-33.0748367393155,
-4.95105023678181));
#37887=CARTESIAN_POINT('Ctrl Pts',(-11.067529982669,-33.0801196648877,-5.07408793132099));
#37888=CARTESIAN_POINT('Ctrl Pts',(-11.0107221639337,-33.0854025904599,
-5.19620826044135));
#37889=CARTESIAN_POINT('Ctrl Pts',(-10.9519091180938,-33.0906855160321,
-5.31734303191104));
#37890=CARTESIAN_POINT('Ctrl Pts',(-10.8278098809659,-33.1018328222794,
-5.5729450418798));
#37891=CARTESIAN_POINT('Ctrl Pts',(-10.6947401199187,-33.1129801285267,
-5.82423887901939));
#37892=CARTESIAN_POINT('Ctrl Pts',(-10.5530246517763,-33.124127434774,-6.07059477720272));
#37893=CARTESIAN_POINT('Ctrl Pts',(-10.4113332539878,-33.1352728476528,
-6.31690883186865));
#37894=CARTESIAN_POINT('Ctrl Pts',(-10.2609992138668,-33.1464182605315,
-6.55828639092668));
#37895=CARTESIAN_POINT('Ctrl Pts',(-10.1023927896335,-33.1575636734103,
-6.7941232086239));
#37896=CARTESIAN_POINT('Ctrl Pts',(-9.94380397317836,-33.168707848975,-7.02993384476881));
#37897=CARTESIAN_POINT('Ctrl Pts',(-9.77694475525955,-33.1798520245398,
-7.26020474653669));
#37898=CARTESIAN_POINT('Ctrl Pts',(-9.60222881583929,-33.1909962001045,
-7.48436049494315));
#37899=CARTESIAN_POINT('Ctrl Pts',(-9.42201071655001,-33.2024913283972,
-7.71557536324092));
#37900=CARTESIAN_POINT('Ctrl Pts',(-9.2334332035449,-33.21398645669,-7.94028343973844));
#37901=CARTESIAN_POINT('Ctrl Pts',(-9.03699622097056,-33.2254815849827,
-8.15788879258377));
#37902=CARTESIAN_POINT('Ctrl Pts',(-8.84654639230963,-33.2366263561204,
-8.36886180602542));
#37903=CARTESIAN_POINT('Ctrl Pts',(-8.64870928031278,-33.2477711272582,
-8.57315844163609));
#37904=CARTESIAN_POINT('Ctrl Pts',(-8.44397971682008,-33.258915898396,-8.77027119261035));
#37905=CARTESIAN_POINT('Ctrl Pts',(-8.22959605637275,-33.2705862052662,
-8.97667886697739));
#37906=CARTESIAN_POINT('Ctrl Pts',(-8.00765450035677,-33.2822565121364,
-9.1752086165817));
#37907=CARTESIAN_POINT('Ctrl Pts',(-7.77876523658056,-33.2939268190066,
-9.36532229259441));
#37908=CARTESIAN_POINT('Ctrl Pts',(-7.54987597280433,-33.3055971258768,
-9.55543596860713));
#37909=CARTESIAN_POINT('Ctrl Pts',(-7.31403926496306,-33.317267432747,-9.73713336341621));
#37910=CARTESIAN_POINT('Ctrl Pts',(-7.07190449795741,-33.3289377396172,
-9.90992517740522));
#37911=CARTESIAN_POINT('Ctrl Pts',(-6.8406209138327,-33.3400850458639,-10.0749733881227));
#37912=CARTESIAN_POINT('Ctrl Pts',(-6.60352227774398,-33.3512323521105,
-10.2319459674008));
#37913=CARTESIAN_POINT('Ctrl Pts',(-6.36119516972689,-33.3623796583572,
-10.3804453788189));
#37914=CARTESIAN_POINT('Ctrl Pts',(-6.1189092209383,-33.3735250712353,-10.5289195676309));
#37915=CARTESIAN_POINT('Ctrl Pts',(-5.87139680057618,-33.3846704841134,
-10.6689233225553));
#37916=CARTESIAN_POINT('Ctrl Pts',(-5.61927217655415,-33.3958158969915,
-10.8001032613491));
#37917=CARTESIAN_POINT('Ctrl Pts',(-5.36717554228243,-33.4069600725556,
-10.9312686371318));
#37918=CARTESIAN_POINT('Ctrl Pts',(-5.11046796335894,-33.4181042481198,
-11.0536120297623));
#37919=CARTESIAN_POINT('Ctrl Pts',(-4.84978803993833,-33.4292484236839,
-11.1668261479111));
#37920=CARTESIAN_POINT('Ctrl Pts',(-4.58089877613062,-33.4407435519771,
-11.2836056086468));
#37921=CARTESIAN_POINT('Ctrl Pts',(-4.30778318746436,-33.4522386802703,
-11.3906713514839));
#37922=CARTESIAN_POINT('Ctrl Pts',(-4.03116543587642,-33.4637338085635,
-11.4877393545726));
#37923=CARTESIAN_POINT('Ctrl Pts',(-3.76297864793515,-33.4748785797007,
-11.5818488461391));
#37924=CARTESIAN_POINT('Ctrl Pts',(-3.49150028225666,-33.4860233508378,
-11.6665609182723));
#37925=CARTESIAN_POINT('Ctrl Pts',(-3.2174076966831,-33.497168121975,-11.7416667455402));
#37926=CARTESIAN_POINT('Ctrl Pts',(-2.9303901756055,-33.5088384288462,-11.8203142153935));
#37927=CARTESIAN_POINT('Ctrl Pts',(-2.64050625979877,-33.5205087357174,
-11.8884275851291));
#37928=CARTESIAN_POINT('Ctrl Pts',(-2.34854926057755,-33.5321790425887,
-11.9458263264054));
#37929=CARTESIAN_POINT('Ctrl Pts',(-2.05659226135631,-33.5438493494599,
-12.0032250676818));
#37930=CARTESIAN_POINT('Ctrl Pts',(-1.7625625096131,-33.5555196563311,-12.0499091243916));
#37931=CARTESIAN_POINT('Ctrl Pts',(-1.46726435779509,-33.5671899632023,
-12.0857596184247));
#37932=CARTESIAN_POINT('Ctrl Pts',(-1.18519988690572,-33.5783372694502,
-12.1200034854055));
#37933=CARTESIAN_POINT('Ctrl Pts',(-0.901893961091638,-33.589484575698,
-12.1443736781867));
#37934=CARTESIAN_POINT('Ctrl Pts',(-0.618051873483406,-33.6006318819459,
-12.1588018378327));
#37935=CARTESIAN_POINT('Ctrl Pts',(-0.33425799641702,-33.6117772948253,
-12.1732275468576));
#37936=CARTESIAN_POINT('Ctrl Pts',(-0.0499284056740375,-33.6229227077046,
-12.177714580606));
#37937=CARTESIAN_POINT('Ctrl Pts',(0.234228423537759,-33.634068120584,-12.1722466001806));
#37938=CARTESIAN_POINT('Ctrl Pts',(0.518353706925605,-33.6452122961493,
-12.1667792267859));
#37939=CARTESIAN_POINT('Ctrl Pts',(0.802306000450644,-33.6563564717146,
-12.1513590511794));
#37940=CARTESIAN_POINT('Ctrl Pts',(1.0853775201037,-33.6675006472799,-12.1260218492651));
#37941=CARTESIAN_POINT('Ctrl Pts',(1.37736353694585,-33.6789957755722,-12.0998867273921));
#37942=CARTESIAN_POINT('Ctrl Pts',(1.66841210986734,-33.6904909038645,-12.0631998598776));
#37943=CARTESIAN_POINT('Ctrl Pts',(1.95775146155432,-33.7019860321568,-12.0160583996909));
#37944=CARTESIAN_POINT('Ctrl Pts',(2.23827211116114,-33.7131308032951,-11.9703537523351));
#37945=CARTESIAN_POINT('Ctrl Pts',(2.51718591111053,-33.7242755744335,-11.9148224061326));
#37946=CARTESIAN_POINT('Ctrl Pts',(2.79379816578905,-33.7354203455718,-11.8496051435832));
#37947=CARTESIAN_POINT('Ctrl Pts',(3.08345417180536,-33.7470906524411,-11.7813125373307));
#37948=CARTESIAN_POINT('Ctrl Pts',(3.37058603990602,-33.7587609593103,-11.7023986217551));
#37949=CARTESIAN_POINT('Ctrl Pts',(3.65441080124198,-33.7704312661796,-11.6130845147087));
#37950=CARTESIAN_POINT('Ctrl Pts',(3.93823556257797,-33.7821015730489,-11.5237704076622));
#37951=CARTESIAN_POINT('Ctrl Pts',(4.2187528997546,-33.7937718799181,-11.4240562182253));
#37952=CARTESIAN_POINT('Ctrl Pts',(4.495199651367,-33.8054421867874,-11.3142224807695));
#37953=CARTESIAN_POINT('Ctrl Pts',(4.75926020200681,-33.8165896053773,-11.2093098456155));
#37954=CARTESIAN_POINT('Ctrl Pts',(5.01968578183422,-33.8277370239671,-11.0951332138277));
#37955=CARTESIAN_POINT('Ctrl Pts',(5.27582436586328,-33.838884442557,-10.971970083379));
#37956=CARTESIAN_POINT('Ctrl Pts',(5.53191609534507,-33.8500298219881,-10.8488294827367));
#37957=CARTESIAN_POINT('Ctrl Pts',(5.78372215460884,-33.8611752014191,-10.7167057814429));
#37958=CARTESIAN_POINT('Ctrl Pts',(6.03061264389333,-33.8723205808502,-10.5759236660121));
#37959=CARTESIAN_POINT('Ctrl Pts',(6.27749257898572,-33.8834654838333,-10.4351475688021));
#37960=CARTESIAN_POINT('Ctrl Pts',(6.51945713068993,-33.8946103868163,-10.2857139263875));
#37961=CARTESIAN_POINT('Ctrl Pts',(6.75590182217983,-33.9057552897994,-10.1279929314286));
#37962=CARTESIAN_POINT('Ctrl Pts',(6.9799620768191,-33.916316448033,-9.9785330045858));
#37963=CARTESIAN_POINT('Ctrl Pts',(7.19906559768597,-33.9268776062666,-9.82163158858564));
#37964=CARTESIAN_POINT('Ctrl Pts',(7.41272179941099,-33.9374387645002,-9.65763976210218));
#37965=CARTESIAN_POINT('',(-12.1744999999831,-32.6251260039388,-2.02629457301205E-5));
#37966=CARTESIAN_POINT('Ctrl Pts',(-12.1744999999831,-32.6251260039651,
-2.02636154117562E-5));
#37967=CARTESIAN_POINT('Ctrl Pts',(-12.1744999682797,-32.6258732859801,
-0.0190678768165046));
#37968=CARTESIAN_POINT('Ctrl Pts',(-12.1744552351083,-32.6266205679952,
-0.0381154725570181));
#37969=CARTESIAN_POINT('Ctrl Pts',(-12.1743658010439,-32.6273678500103,
-0.057162858329975));
#37970=CARTESIAN_POINT('Ctrl Pts',(-12.1730317010868,-32.6385151562574,
-0.341295271704965));
#37971=CARTESIAN_POINT('Ctrl Pts',(-12.1617461874558,-32.6496624625045,
-0.625423396093907));
#37972=CARTESIAN_POINT('Ctrl Pts',(-12.1405297269587,-32.6608097687516,
-0.908838928981096));
#37973=CARTESIAN_POINT('Ctrl Pts',(-12.1193168700748,-32.6719551816302,
-1.19220632377607));
#37974=CARTESIAN_POINT('Ctrl Pts',(-12.0881764538661,-32.6831005945087,
-1.47486110281071));
#37975=CARTESIAN_POINT('Ctrl Pts',(-12.0471809543266,-32.6942460073873,
-1.75609831834951));
#37976=CARTESIAN_POINT('Ctrl Pts',(-12.0061900059243,-32.7053901829519,
-2.03730431218924));
#37977=CARTESIAN_POINT('Ctrl Pts',(-11.9553461973366,-32.7165343585165,
-2.31709279288919));
#37978=CARTESIAN_POINT('Ctrl Pts',(-11.8947736229075,-32.7276785340811,
-2.59476602216561));
#37979=CARTESIAN_POINT('Ctrl Pts',(-11.8322934950546,-32.739173662374,-2.88118374553293));
#37980=CARTESIAN_POINT('Ctrl Pts',(-11.7594619685466,-32.7506687906668,
-3.16535053951657));
#37981=CARTESIAN_POINT('Ctrl Pts',(-11.6764720426416,-32.7621639189597,
-3.44651285902283));
#37982=CARTESIAN_POINT('Ctrl Pts',(-11.5960115460404,-32.7733086900973,
-3.71910570214559));
#37983=CARTESIAN_POINT('Ctrl Pts',(-11.506002790155,-32.7844534612349,-3.98887423638641));
#37984=CARTESIAN_POINT('Ctrl Pts',(-11.4066724115637,-32.7955982323725,
-4.25514685354945));
#37985=CARTESIAN_POINT('Ctrl Pts',(-11.3026580728741,-32.807268539243,-4.53397565273587));
#37986=CARTESIAN_POINT('Ctrl Pts',(-11.1884219401367,-32.8189388461134,
-4.80897060131908));
#37987=CARTESIAN_POINT('Ctrl Pts',(-11.0642814033507,-32.8306091529839,
-5.07938256852815));
#37988=CARTESIAN_POINT('Ctrl Pts',(-10.9401408665647,-32.8422794598544,
-5.34979453573721));
#37989=CARTESIAN_POINT('Ctrl Pts',(-10.8060960736838,-32.8539497667249,
-5.61562322032863));
#37990=CARTESIAN_POINT('Ctrl Pts',(-10.6625208843845,-32.8656200735954,
-5.87614658088653));
#37991=CARTESIAN_POINT('Ctrl Pts',(-10.5253799657805,-32.8767673798425,
-6.12499468033231));
#37992=CARTESIAN_POINT('Ctrl Pts',(-10.3795031187475,-32.8879146860897,
-6.3690768373752));
#37993=CARTESIAN_POINT('Ctrl Pts',(-10.2252472674586,-32.8990619923368,
-6.60778091111761));
#37994=CARTESIAN_POINT('Ctrl Pts',(-10.0710176165062,-32.9102074052154,
-6.84644444100378));
#37995=CARTESIAN_POINT('Ctrl Pts',(-9.9084119473859,-32.921352818094,-7.07973148737207));
#37996=CARTESIAN_POINT('Ctrl Pts',(-9.73783124627379,-32.9324982309726,
-7.30705774365399));
#37997=CARTESIAN_POINT('Ctrl Pts',(-9.56726948226978,-32.9436424065372,
-7.53435876318956));
#37998=CARTESIAN_POINT('Ctrl Pts',(-9.3887346142411,-32.9547865821018,-7.75570010072467));
#37999=CARTESIAN_POINT('Ctrl Pts',(-9.20266950256293,-32.9659307576664,
-7.97052848163773));
#38000=CARTESIAN_POINT('Ctrl Pts',(-9.01074482252143,-32.9774258859592,
-8.19212224469573));
#38001=CARTESIAN_POINT('Ctrl Pts',(-8.81080811489427,-32.9889210142521,
-8.40678596077151));
#38002=CARTESIAN_POINT('Ctrl Pts',(-8.60338944894226,-33.0004161425449,
-8.6139503272209));
#38003=CARTESIAN_POINT('Ctrl Pts',(-8.40229264490357,-33.0115609136825,
-8.81480058248823));
#38004=CARTESIAN_POINT('Ctrl Pts',(-8.19416340784828,-33.0227056848202,
-9.00860166320182));
#38005=CARTESIAN_POINT('Ctrl Pts',(-7.97952213246204,-33.0338504559578,
-9.19487230947491));
#38006=CARTESIAN_POINT('Ctrl Pts',(-7.75475936973759,-33.0455207628282,
-9.38992661576092));
#38007=CARTESIAN_POINT('Ctrl Pts',(-7.52285587600274,-33.0571910696987,
-9.57672298982141));
#38008=CARTESIAN_POINT('Ctrl Pts',(-7.28444883114305,-33.0688613765691,
-9.75475553135283));
#38009=CARTESIAN_POINT('Ctrl Pts',(-7.04604178628334,-33.0805316834396,
-9.93278807288427));
#38010=CARTESIAN_POINT('Ctrl Pts',(-6.80113146436942,-33.09220199031,-10.1020565881776));
#38011=CARTESIAN_POINT('Ctrl Pts',(-6.55039166588011,-33.1038722971805,
-10.2621059862763));
#38012=CARTESIAN_POINT('Ctrl Pts',(-6.31088868167215,-33.1150196034276,
-10.4149828279117));
#38013=CARTESIAN_POINT('Ctrl Pts',(-6.06599569770914,-33.1261669096747,
-10.5594943509551));
#38014=CARTESIAN_POINT('Ctrl Pts',(-5.81631905191834,-33.1373142159218,
-10.695273859808));
#38015=CARTESIAN_POINT('Ctrl Pts',(-5.56668481367376,-33.1484596288003,
-10.8310303065287));
#38016=CARTESIAN_POINT('Ctrl Pts',(-5.31226877001417,-33.1596050416789,
-10.9580575727416));
#38017=CARTESIAN_POINT('Ctrl Pts',(-5.05370262822269,-33.1707504545575,
-11.0760344887281));
#38018=CARTESIAN_POINT('Ctrl Pts',(-4.79516519128955,-33.1818946301221,
-11.1939983074444));
#38019=CARTESIAN_POINT('Ctrl Pts',(-4.53247881883711,-33.1930388056867,
-11.3029136715195));
#38020=CARTESIAN_POINT('Ctrl Pts',(-4.26629713627511,-33.2041829812513,
-11.4025066978718));
#38021=CARTESIAN_POINT('Ctrl Pts',(-3.9917328517731,-33.2156781095442,-11.5052361109501));
#38022=CARTESIAN_POINT('Ctrl Pts',(-3.71344981544439,-33.227173237837,-11.5980463999713));
#38023=CARTESIAN_POINT('Ctrl Pts',(-3.43218589779943,-33.2386683661299,
-11.6806913413953));
#38024=CARTESIAN_POINT('Ctrl Pts',(-3.15949455312228,-33.2498131372675,
-11.7608173682115));
#38025=CARTESIAN_POINT('Ctrl Pts',(-2.8840016112494,-33.2609579084051,-11.8313884471381));
#38026=CARTESIAN_POINT('Ctrl Pts',(-2.60639431557328,-33.2721026795427,
-11.8922310321381));
#38027=CARTESIAN_POINT('Ctrl Pts',(-2.31569634698968,-33.2837729864132,
-11.9559426713433));
#38028=CARTESIAN_POINT('Ctrl Pts',(-2.02268013077371,-33.2954432932836,
-12.0089861705082));
#38029=CARTESIAN_POINT('Ctrl Pts',(-1.7281472467221,-33.3071136001541,-12.0512222344311));
#38030=CARTESIAN_POINT('Ctrl Pts',(-1.43361436267048,-33.3187839070246,
-12.0934582983541));
#38031=CARTESIAN_POINT('Ctrl Pts',(-1.13756514413288,-33.3304542138951,
-12.1248868881006));
#38032=CARTESIAN_POINT('Ctrl Pts',(-0.840809011698687,-33.3421245207656,
-12.1454308468595));
#38033=CARTESIAN_POINT('Ctrl Pts',(-0.557351899073608,-33.3532718270128,
-12.1650541354633));
#38034=CARTESIAN_POINT('Ctrl Pts',(-0.273165182359102,-33.3644191332599,
-12.1747527915611));
#38035=CARTESIAN_POINT('Ctrl Pts',(0.0110432552658722,-33.375566439507,
-12.1744949914365));
#38036=CARTESIAN_POINT('Ctrl Pts',(0.295203420124147,-33.3867118523856,
-12.1742372350993));
#38037=CARTESIAN_POINT('Ctrl Pts',(0.579385031881237,-33.3978572652642,
-12.1640263990678));
#38038=CARTESIAN_POINT('Ctrl Pts',(0.862879717510703,-33.4090026781428,
-12.1438827745951));
#38039=CARTESIAN_POINT('Ctrl Pts',(1.14634293082577,-33.4201468537074,-12.1237413863777));
#38040=CARTESIAN_POINT('Ctrl Pts',(1.42911910428309,-33.431291029272,-12.0936694305245));
#38041=CARTESIAN_POINT('Ctrl Pts',(1.71050324800699,-33.4424352048366,-12.0537392077545));
#38042=CARTESIAN_POINT('Ctrl Pts',(2.00074875005628,-33.4539303331295,-12.0125515011501));
#38043=CARTESIAN_POINT('Ctrl Pts',(2.28951283081739,-33.4654254614223,-11.9608745844622));
#38044=CARTESIAN_POINT('Ctrl Pts',(2.57602976407274,-33.4769205897152,-11.8988453601436));
#38045=CARTESIAN_POINT('Ctrl Pts',(2.85381401900554,-33.4880653608528,-11.83870670912));
#38046=CARTESIAN_POINT('Ctrl Pts',(3.12948580577611,-33.4992101319904,-11.7688375157536));
#38047=CARTESIAN_POINT('Ctrl Pts',(3.40235863131958,-33.510354903128,-11.6894142707787));
#38048=CARTESIAN_POINT('Ctrl Pts',(3.68809887410928,-33.5220252099985,-11.6062457938259));
#38049=CARTESIAN_POINT('Ctrl Pts',(3.97076952676932,-33.5336955168689,-11.5126006236716));
#38050=CARTESIAN_POINT('Ctrl Pts',(4.24960009200961,-33.5453658237394,-11.4087400403371));
#38051=CARTESIAN_POINT('Ctrl Pts',(4.52843065724992,-33.5570361306098,-11.3048794570027));
#38052=CARTESIAN_POINT('Ctrl Pts',(4.80342082373624,-33.5687064374803,-11.1908035858233));
#38053=CARTESIAN_POINT('Ctrl Pts',(5.07382294533181,-33.5803767443507,-11.0668320204756));
#38054=CARTESIAN_POINT('Ctrl Pts',(5.33210550270062,-33.5915239819759,-10.948416925394));
#38055=CARTESIAN_POINT('Ctrl Pts',(5.58627938950382,-33.6026712196011,-10.8209383299319));
#38056=CARTESIAN_POINT('Ctrl Pts',(5.83570782148966,-33.6138184572262,-10.6847070372661));
#38057=CARTESIAN_POINT('Ctrl Pts',(6.08509174313785,-33.6249637056343,-10.5485000549839));
#38058=CARTESIAN_POINT('Ctrl Pts',(6.32973166681211,-33.6361089540423,-10.4035436219664));
#38059=CARTESIAN_POINT('Ctrl Pts',(6.56901533244333,-33.6472542024504,-10.2501945255748));
#38060=CARTESIAN_POINT('Ctrl Pts',(6.80827488209085,-33.6583983275948,-10.0968608843306));
#38061=CARTESIAN_POINT('Ctrl Pts',(7.04217902691351,-33.6695424527393,-9.9351364122925));
#38062=CARTESIAN_POINT('Ctrl Pts',(7.27014334671615,-33.6806865778837,-9.76542195546096));
#38063=CARTESIAN_POINT('Ctrl Pts',(7.31793216376122,-33.6830227529401,-9.72984422498785));
#38064=CARTESIAN_POINT('Ctrl Pts',(7.36546005321909,-33.6853589279964,-9.69391551734931));
#38065=CARTESIAN_POINT('Ctrl Pts',(7.412721799411,-33.6876951030527,-9.65763976210218));
#38066=CARTESIAN_POINT('Ctrl Pts',(7.41272179941101,-30.6876856710377,-9.65763976210217));
#38067=CARTESIAN_POINT('Ctrl Pts',(7.63967546407975,-30.6989071344683,-9.48344146738549));
#38068=CARTESIAN_POINT('Ctrl Pts',(7.86046128966899,-30.7101285978989,-9.30125847901165));
#38069=CARTESIAN_POINT('Ctrl Pts',(8.07452674462437,-30.7213500613295,-9.11155684284227));
#38070=CARTESIAN_POINT('Ctrl Pts',(8.28717754530411,-30.7324973675766,-8.92310885234291));
#38071=CARTESIAN_POINT('Ctrl Pts',(8.49326006179604,-30.7436446738237,-8.72718501437767));
#38072=CARTESIAN_POINT('Ctrl Pts',(8.69225549345207,-30.7547919800708,-8.5242679853787));
#38073=CARTESIAN_POINT('Ctrl Pts',(8.89121712575985,-30.7659373929494,-8.32138542181079));
#38074=CARTESIAN_POINT('Ctrl Pts',(9.08309388980057,-30.777082805828,-8.11151222901466));
#38075=CARTESIAN_POINT('Ctrl Pts',(9.26740381715966,-30.7882282187066,-7.89516793612995));
#38076=CARTESIAN_POINT('Ctrl Pts',(9.45169328325431,-30.7993723942712,-7.67884766082179));
#38077=CARTESIAN_POINT('Ctrl Pts',(9.62841741714516,-30.8105165698359,-7.45605792294065));
#38078=CARTESIAN_POINT('Ctrl Pts',(9.79713372167153,-30.8216607454005,-7.22735228764217));
#38079=CARTESIAN_POINT('Ctrl Pts',(9.97116324537854,-30.8331558736934,-6.99144424726733));
#38080=CARTESIAN_POINT('Ctrl Pts',(10.1366722171911,-30.8446510019862,-6.74924189734947));
#38081=CARTESIAN_POINT('Ctrl Pts',(10.2932216574243,-30.8561461302791,-6.50138740278804));
#38082=CARTESIAN_POINT('Ctrl Pts',(10.4449996662181,-30.8672909014166,-6.26108720370023));
#38083=CARTESIAN_POINT('Ctrl Pts',(10.5883560576907,-30.8784356725542,-6.01547453459209));
#38084=CARTESIAN_POINT('Ctrl Pts',(10.7229356202202,-30.8895804436918,-5.76516278474537));
#38085=CARTESIAN_POINT('Ctrl Pts',(10.8638613309254,-30.9012507505623,-5.50304749337414));
#38086=CARTESIAN_POINT('Ctrl Pts',(10.9951623959193,-30.9129210574327,-5.23577956394708));
#38087=CARTESIAN_POINT('Ctrl Pts',(11.1164852149529,-30.9245913643032,-4.96409173119642));
#38088=CARTESIAN_POINT('Ctrl Pts',(11.2378080339866,-30.9362616711737,-4.69240389844574));
#38089=CARTESIAN_POINT('Ctrl Pts',(11.3491524782766,-30.9479319780441,-4.41629647229513));
#38090=CARTESIAN_POINT('Ctrl Pts',(11.4502225594297,-30.9596022849146,-4.13652675435896));
#38091=CARTESIAN_POINT('Ctrl Pts',(11.5467632210884,-30.9707495911617,-3.86929481614853));
#38092=CARTESIAN_POINT('Ctrl Pts',(11.6339589947617,-30.9818968974088,-3.59864180777725));
#38093=CARTESIAN_POINT('Ctrl Pts',(11.7115853118451,-30.993044203656,-3.32523980088261));
#38094=CARTESIAN_POINT('Ctrl Pts',(11.7891984441082,-31.0041896165345,-3.05188423128495));
#38095=CARTESIAN_POINT('Ctrl Pts',(11.8572452920049,-31.015335029413,-2.77578085187103));
#38096=CARTESIAN_POINT('Ctrl Pts',(11.9155512731645,-31.0264804422916,-2.49761648508908));
#38097=CARTESIAN_POINT('Ctrl Pts',(11.9738507814546,-31.0376246178562,-2.21948299887197));
#38098=CARTESIAN_POINT('Ctrl Pts',(12.022411527657,-31.0487687934208,-1.9392892431739));
#38099=CARTESIAN_POINT('Ctrl Pts',(12.0611098753863,-31.0599129689854,-1.65773303757252));
#38100=CARTESIAN_POINT('Ctrl Pts',(12.1010269127024,-31.0714080972782,-1.36731005506706));
#38101=CARTESIAN_POINT('Ctrl Pts',(12.1304502618443,-31.0829032255711,-1.07543771211255));
#38102=CARTESIAN_POINT('Ctrl Pts',(12.1493017737572,-31.094398353864,-0.782889941294685));
#38103=CARTESIAN_POINT('Ctrl Pts',(12.1675787151288,-31.1055431250016,-0.499258661197821));
#38104=CARTESIAN_POINT('Ctrl Pts',(12.17591869138,-31.1166878961392,-0.214992794448297));
#38105=CARTESIAN_POINT('Ctrl Pts',(12.1743033368384,-31.1278326672768,0.069199079805505));
#38106=CARTESIAN_POINT('Ctrl Pts',(12.1726118096663,-31.1395029741473,0.366792125161997));
#38107=CARTESIAN_POINT('Ctrl Pts',(12.1600034675358,-31.1511732810177,0.664303713974559));
#38108=CARTESIAN_POINT('Ctrl Pts',(12.136518471558,-31.1628435878882,0.960921245228644));
#38109=CARTESIAN_POINT('Ctrl Pts',(12.1130334755802,-31.1745138947587,1.25753877648276));
#38110=CARTESIAN_POINT('Ctrl Pts',(12.0786718609865,-31.1861842016292,1.55326191641704));
#38111=CARTESIAN_POINT('Ctrl Pts',(12.0335361321028,-31.1978545084997,1.84728406244831));
#38112=CARTESIAN_POINT('Ctrl Pts',(11.9904231447464,-31.2090018147468,2.12812971129163));
#38113=CARTESIAN_POINT('Ctrl Pts',(11.9374676168789,-31.2201491209939,2.40750735169076));
#38114=CARTESIAN_POINT('Ctrl Pts',(11.8747939778081,-31.231296427241,2.68471939587967));
#38115=CARTESIAN_POINT('Ctrl Pts',(11.8121309838468,-31.2424418401196,2.96188435563876));
#38116=CARTESIAN_POINT('Ctrl Pts',(11.7397532329452,-31.2535872529982,3.2368841934707));
#38117=CARTESIAN_POINT('Ctrl Pts',(11.6578361044304,-31.2647326658768,3.50903228999679));
#38118=CARTESIAN_POINT('Ctrl Pts',(11.5759280699893,-31.2758768414414,3.7811501738566));
#38119=CARTESIAN_POINT('Ctrl Pts',(11.4844828494922,-31.287021017006,4.0504166932242));
#38120=CARTESIAN_POINT('Ctrl Pts',(11.383725818712,-31.2981651925706,4.31615995236384));
#38121=CARTESIAN_POINT('Ctrl Pts',(11.2797957443419,-31.3096603208635,4.59027200659853));
#38122=CARTESIAN_POINT('Ctrl Pts',(11.1659579563437,-31.3211554491563,4.8606350145712));
#38123=CARTESIAN_POINT('Ctrl Pts',(11.0425141946155,-31.3326505774492,5.12653201606268));
#38124=CARTESIAN_POINT('Ctrl Pts',(10.922832844588,-31.3437953485868,5.38432480900107));
#38125=CARTESIAN_POINT('Ctrl Pts',(10.7941225236154,-31.3549401197244,5.63791954766483));
#38126=CARTESIAN_POINT('Ctrl Pts',(10.6567061908373,-31.366084890862,5.88668526525489));
#38127=CARTESIAN_POINT('Ctrl Pts',(10.5128099409518,-31.3777551977325,6.14718162065625));
#38128=CARTESIAN_POINT('Ctrl Pts',(10.3593670062242,-31.3894255046029,6.40238228983842));
#38129=CARTESIAN_POINT('Ctrl Pts',(10.1968015149776,-31.4010958114734,6.65159297568257));
#38130=CARTESIAN_POINT('Ctrl Pts',(10.0342360237311,-31.4127661183439,6.90080366152668));
#38131=CARTESIAN_POINT('Ctrl Pts',(9.86254816662018,-31.4244364252143,7.14402408782862));
#38132=CARTESIAN_POINT('Ctrl Pts',(9.68221394281234,-31.4361067320848,7.38059505836828));
#38133=CARTESIAN_POINT('Ctrl Pts',(9.50996133266801,-31.4472540383319,7.60656418557765));
#38134=CARTESIAN_POINT('Ctrl Pts',(9.32976884399584,-31.4584013445791,7.82653423106822));
#38135=CARTESIAN_POINT('Ctrl Pts',(9.1420795592616,-31.4695486508262,8.0399522126771));
#38136=CARTESIAN_POINT('Ctrl Pts',(8.95442215352886,-31.4806940637047,8.25333394526852));
#38137=CARTESIAN_POINT('Ctrl Pts',(8.75927067002798,-31.4918394765833,8.4601656355874));
#38138=CARTESIAN_POINT('Ctrl Pts',(8.557107679775,-31.5029848894619,8.65992831417996));
#38139=CARTESIAN_POINT('Ctrl Pts',(8.35496713275467,-31.5141290650264,8.85966881601174));
#38140=CARTESIAN_POINT('Ctrl Pts',(8.14581682298889,-31.525273240591,9.05234168573748));
#38141=CARTESIAN_POINT('Ctrl Pts',(7.93017617569519,-31.5364174161556,9.23746480764265));
#38142=CARTESIAN_POINT('Ctrl Pts',(7.70774456633725,-31.5479125444485,9.42841783274024));
#38143=CARTESIAN_POINT('Ctrl Pts',(7.47840742626827,-31.5594076727413,9.61133769016819));
#38144=CARTESIAN_POINT('Ctrl Pts',(7.24277279859588,-31.5709028010342,9.78573923819349));
#38145=CARTESIAN_POINT('Ctrl Pts',(7.01432002011501,-31.5820475721717,9.95482524482719));
#38146=CARTESIAN_POINT('Ctrl Pts',(6.77994817299307,-31.5931923433093,10.1159043417922));
#38147=CARTESIAN_POINT('Ctrl Pts',(6.54024278067235,-31.6043371144469,10.2685770494194));
#38148=CARTESIAN_POINT('Ctrl Pts',(6.28923399346961,-31.6160074213174,10.4284490940549));
#38149=CARTESIAN_POINT('Ctrl Pts',(6.03237681530273,-31.6276777281879,10.57910268941));
#38150=CARTESIAN_POINT('Ctrl Pts',(5.77037590892259,-31.6393480350584,10.7201311614982));
#38151=CARTESIAN_POINT('Ctrl Pts',(5.50837500254246,-31.6510183419289,10.8611596335865));
#38152=CARTESIAN_POINT('Ctrl Pts',(5.24123066753154,-31.6626886487994,10.9925628311193));
#38153=CARTESIAN_POINT('Ctrl Pts',(4.96967631529748,-31.6743589556699,11.1139897233699));
#38154=CARTESIAN_POINT('Ctrl Pts',(4.71029157411813,-31.685506261917,11.2299749129259));
#38155=CARTESIAN_POINT('Ctrl Pts',(4.44680592598916,-31.6966535681641,11.3368929521746));
#38156=CARTESIAN_POINT('Ctrl Pts',(4.1798730513762,-31.7078008744112,11.4344703211115));
#38157=CARTESIAN_POINT('Ctrl Pts',(3.9129855152784,-31.7189462872898,11.5320311165445));
#38158=CARTESIAN_POINT('Ctrl Pts',(3.64265217210709,-31.7300917001683,11.6202543175883));
#38159=CARTESIAN_POINT('Ctrl Pts',(3.36954509927963,-31.7412371130469,11.6989151665409));
#38160=CARTESIAN_POINT('Ctrl Pts',(3.09646834558192,-31.7523812886114,11.7775672829167));
#38161=CARTESIAN_POINT('Ctrl Pts',(2.82061873337085,-31.7635254641758,11.8466590931784));
#38162=CARTESIAN_POINT('Ctrl Pts',(2.54268306433363,-31.7746696397403,11.9060158358853));
#38163=CARTESIAN_POINT('Ctrl Pts',(2.2559946364402,-31.7861647680332,11.9672418430058));
#38164=CARTESIAN_POINT('Ctrl Pts',(1.96708692245802,-31.7976598963261,12.0181096212011));
#38165=CARTESIAN_POINT('Ctrl Pts',(1.67672598435743,-31.809155024619,12.0584841594365));
#38166=CARTESIAN_POINT('Ctrl Pts',(1.39521488504789,-31.8202997957566,12.0976281321661));
#38167=CARTESIAN_POINT('Ctrl Pts',(1.11233811118305,-31.8314445668942,12.1269089964084));
#38168=CARTESIAN_POINT('Ctrl Pts',(0.828800958063812,-31.8425893380319,
12.1462561813059));
#38169=CARTESIAN_POINT('Ctrl Pts',(0.531893507454375,-31.8542596449024,
12.1665156897378));
#38170=CARTESIAN_POINT('Ctrl Pts',(0.234262215273674,-31.8659299517729,
12.1758821023111));
#38171=CARTESIAN_POINT('Ctrl Pts',(-0.0632795684179096,-31.8776002586434,
12.1743355443417));
#38172=CARTESIAN_POINT('Ctrl Pts',(-0.360821352109494,-31.889270565514,
12.1727889863723));
#38173=CARTESIAN_POINT('Ctrl Pts',(-0.658273291861257,-31.9009408723845,
12.1603294683821));
#38174=CARTESIAN_POINT('Ctrl Pts',(-0.95482342212009,-31.912611179255,12.1369997315058));
#38175=CARTESIAN_POINT('Ctrl Pts',(-1.23808376448244,-31.9237584855021,
12.1147155084335));
#38176=CARTESIAN_POINT('Ctrl Pts',(-1.52060594814087,-31.9349057917492,
12.0825072854502));
#38177=CARTESIAN_POINT('Ctrl Pts',(-1.80168510862513,-31.9460530979963,
12.0404477084267));
#38178=CARTESIAN_POINT('Ctrl Pts',(-2.08271652784845,-31.9571985108749,
11.9983952752173));
#38179=CARTESIAN_POINT('Ctrl Pts',(-2.36230514952426,-31.9683439237534,
11.9464948680739));
#38180=CARTESIAN_POINT('Ctrl Pts',(-2.63975329032011,-31.9794893366319,
11.8848707530307));
#38181=CARTESIAN_POINT('Ctrl Pts',(-2.9171706300654,-31.9906335121966,11.8232534792208));
#38182=CARTESIAN_POINT('Ctrl Pts',(-3.19244770309873,-32.0017776877613,
11.751914710889));
#38183=CARTESIAN_POINT('Ctrl Pts',(-3.46489782257824,-32.0129218633259,
11.6710296601925));
#38184=CARTESIAN_POINT('Ctrl Pts',(-3.74592794980863,-32.0244169916188,
11.5875973749297));
#38185=CARTESIAN_POINT('Ctrl Pts',(-4.02394989801542,-32.0359121199116,
11.4940078756704));
#38186=CARTESIAN_POINT('Ctrl Pts',(-4.29822640699997,-32.0474072482045,
11.3905092074133));
#38187=CARTESIAN_POINT('Ctrl Pts',(-4.56414331050772,-32.0585520193421,
11.2901650493154));
#38188=CARTESIAN_POINT('Ctrl Pts',(-4.82653944546716,-32.0696967904797,
11.1805069143627));
#38189=CARTESIAN_POINT('Ctrl Pts',(-5.08476174609812,-32.0808415616173,
11.0618103507255));
#38190=CARTESIAN_POINT('Ctrl Pts',(-5.35516061314951,-32.0925118684878,
10.9375166074974));
#38191=CARTESIAN_POINT('Ctrl Pts',(-5.62098224809431,-32.1041821753582,
10.8033116367849));
#38192=CARTESIAN_POINT('Ctrl Pts',(-5.88150296641168,-32.1158524822287,
10.6595672100743));
#38193=CARTESIAN_POINT('Ctrl Pts',(-6.14202368472907,-32.1275227890992,
10.5158227833637));
#38194=CARTESIAN_POINT('Ctrl Pts',(-6.39724319690685,-32.1391930959696,
10.3625390704213));
#38195=CARTESIAN_POINT('Ctrl Pts',(-6.64646899845364,-32.1508634028401,
10.2001421609012));
#38196=CARTESIAN_POINT('Ctrl Pts',(-6.88452583494995,-32.1620107090872,
10.0450230107282));
#38197=CARTESIAN_POINT('Ctrl Pts',(-7.11718546291348,-32.1731580153343,
9.88154319117064));
#38198=CARTESIAN_POINT('Ctrl Pts',(-7.3438637301814,-32.1843053215814,9.71010379772154));
#38199=CARTESIAN_POINT('Ctrl Pts',(-7.57050349617527,-32.19545073446,9.53869352323099));
#38200=CARTESIAN_POINT('Ctrl Pts',(-7.79116371711331,-32.2065961473386,
9.3593265348274));
#38201=CARTESIAN_POINT('Ctrl Pts',(-8.00529124878566,-32.2177415602172,
9.17244581734423));
#38202=CARTESIAN_POINT('Ctrl Pts',(-8.2193950089754,-32.2288857357819,8.98558584652402));
#38203=CARTESIAN_POINT('Ctrl Pts',(-8.42696732714878,-32.2400299113465,
8.79121398762406));
#38204=CARTESIAN_POINT('Ctrl Pts',(-8.627489094617,-32.2511740869111,8.58981269715847));
#38205=CARTESIAN_POINT('Ctrl Pts',(-8.83432569990824,-32.2626692152039,
8.3820688709039));
#38206=CARTESIAN_POINT('Ctrl Pts',(-9.03366027000809,-32.2741643434968,
8.16684589996586));
#38207=CARTESIAN_POINT('Ctrl Pts',(-9.22496414319454,-32.2856594717896,
7.94471439428599));
#38208=CARTESIAN_POINT('Ctrl Pts',(-9.41043731322679,-32.2968042429273,
7.72935317950114));
#38209=CARTESIAN_POINT('Ctrl Pts',(-9.58836188649626,-32.3079490140649,
7.50749853242398));
#38210=CARTESIAN_POINT('Ctrl Pts',(-9.75829629083444,-32.3190937852025,
7.27970492192416));
#38211=CARTESIAN_POINT('Ctrl Pts',(-9.93624401376104,-32.3307640920729,
7.04116962094411));
#38212=CARTESIAN_POINT('Ctrl Pts',(-10.1054296870796,-32.3424343989434,
6.79612202615387));
#38213=CARTESIAN_POINT('Ctrl Pts',(-10.2653957777935,-32.3541047058139,
6.54523489076284));
#38214=CARTESIAN_POINT('Ctrl Pts',(-10.4253618685074,-32.3657750126843,
6.2943477553718));
#38215=CARTESIAN_POINT('Ctrl Pts',(-10.576108203647,-32.3774453195548,6.03762136698964));
#38216=CARTESIAN_POINT('Ctrl Pts',(-10.7172306218485,-32.3891156264253,
5.77576125269328));
#38217=CARTESIAN_POINT('Ctrl Pts',(-10.8519688998768,-32.4002579882968,
5.52574724829742));
#38218=CARTESIAN_POINT('Ctrl Pts',(-10.9779752599429,-32.4114003501683,
5.27097837052066));
#38219=CARTESIAN_POINT('Ctrl Pts',(-11.0949288753281,-32.4225427120399,
5.0120857436213));
#38220=CARTESIAN_POINT('Ctrl Pts',(-11.2118624589273,-32.4336831654505,
4.75323745978609));
#38221=CARTESIAN_POINT('Ctrl Pts',(-11.3197462835136,-32.4448236188611,
4.49026708040664));
#38222=CARTESIAN_POINT('Ctrl Pts',(-11.418306790496,-32.4559640722717,4.22382768210448));
#38223=CARTESIAN_POINT('Ctrl Pts',(-11.5168563332357,-32.4671032863762,
3.9574179235265));
#38224=CARTESIAN_POINT('Ctrl Pts',(-11.6060845367131,-32.4782425004807,
3.68754016717926));
#38225=CARTESIAN_POINT('Ctrl Pts',(-11.6857666143717,-32.4893817145852,
3.41486586624351));
#38226=CARTESIAN_POINT('Ctrl Pts',(-11.7666848528916,-32.500693738698,3.13796138822696));
#38227=CARTESIAN_POINT('Ctrl Pts',(-11.8377582625043,-32.5120057628108,
2.85817315383455));
#38228=CARTESIAN_POINT('Ctrl Pts',(-11.8988041826084,-32.5233177869236,
2.57621995837733));
#38229=CARTESIAN_POINT('Ctrl Pts',(-11.9589208024357,-32.5344576084204,
2.29855892826241));
#38230=CARTESIAN_POINT('Ctrl Pts',(-12.009312981119,-32.5455974299172,2.01879864552249));
#38231=CARTESIAN_POINT('Ctrl Pts',(-12.0498576548315,-32.556737251414,1.73763654090826));
#38232=CARTESIAN_POINT('Ctrl Pts',(-12.0913424556654,-32.5681353768348,
1.44995500733155));
#38233=CARTESIAN_POINT('Ctrl Pts',(-12.1225175320442,-32.5795335022556,
1.16080614795246));
#38234=CARTESIAN_POINT('Ctrl Pts',(-12.1433070423736,-32.5909316276764,
0.870944501468714));
#38235=CARTESIAN_POINT('Ctrl Pts',(-12.1640965527031,-32.6023297530972,
0.581082854984967));
#38236=CARTESIAN_POINT('Ctrl Pts',(-12.1745004835326,-32.613727878518,0.290508720558424));
#38237=CARTESIAN_POINT('Ctrl Pts',(-12.1744999999831,-32.6251260039388,
-2.02629457920173E-5));
#38238=CARTESIAN_POINT('Origin',(0.,-13.3748739960349,0.));
#38239=CARTESIAN_POINT('',(7.412721799411,-27.6877007372717,-9.65763976210218));
#38240=CARTESIAN_POINT('',(7.41272179941101,-27.9374461219842,-9.65763976210217));
#38241=CARTESIAN_POINT('',(7.41272179941101,-13.3748739960349,-9.65763976210217));
#38242=CARTESIAN_POINT('',(-12.174396721221,-29.8748739960031,-4.71261348963091E-6));
#38243=CARTESIAN_POINT('Ctrl Pts',(7.41272179941101,-27.9374461219842,-9.65763976210217));
#38244=CARTESIAN_POINT('Ctrl Pts',(7.63815696377125,-27.9485898492208,-9.48460699236017));
#38245=CARTESIAN_POINT('Ctrl Pts',(7.8575395359938,-27.9597335764574,-9.303670767682));
#38246=CARTESIAN_POINT('Ctrl Pts',(8.0703221215742,-27.970877303694,-9.11528118622954));
#38247=CARTESIAN_POINT('Ctrl Pts',(8.28312509826385,-27.982022098842,-8.92687355126708));
#38248=CARTESIAN_POINT('Ctrl Pts',(8.48932662312901,-27.9931668939901,-8.73101130733214));
#38249=CARTESIAN_POINT('Ctrl Pts',(8.68841372480532,-28.0043116891381,-8.52818369857348));
#38250=CARTESIAN_POINT('Ctrl Pts',(8.88750330607416,-28.0154566230925,-8.32535356363499));
#38251=CARTESIAN_POINT('Ctrl Pts',(9.0794781021168,-28.0266015570469,-8.11555808277237));
#38252=CARTESIAN_POINT('Ctrl Pts',(9.26386259015722,-28.0377464910013,-7.89932276595188));
#38253=CARTESIAN_POINT('Ctrl Pts',(9.44828472996781,-28.0488937007788,-7.68304329334291));
#38254=CARTESIAN_POINT('Ctrl Pts',(9.62511329145496,-28.0600409105564,-7.46032156006608));
#38255=CARTESIAN_POINT('Ctrl Pts',(9.79391260850612,-28.0711881203339,-7.23171667496349));
#38256=CARTESIAN_POINT('Ctrl Pts',(9.87568694844433,-28.0765883538043,-7.12096970090879));
#38257=CARTESIAN_POINT('Ctrl Pts',(9.95557752999588,-28.0819885872747,-7.00884249464973));
#38258=CARTESIAN_POINT('Ctrl Pts',(10.0335383821488,-28.087388820745,-6.89540120543738));
#38259=CARTESIAN_POINT('Ctrl Pts',(10.194467256614,-28.0985361269921,-6.66123266460331));
#38260=CARTESIAN_POINT('Ctrl Pts',(10.3472188441184,-28.1096834332392,-6.42139291309911));
#38261=CARTESIAN_POINT('Ctrl Pts',(10.4914060523786,-28.1208307394863,-6.1764754750677));
#38262=CARTESIAN_POINT('Ctrl Pts',(10.6355687704599,-28.1319761523649,-5.93159963623197));
#38263=CARTESIAN_POINT('Ctrl Pts',(10.7711698782457,-28.1431215652434,-5.68164806252201));
#38264=CARTESIAN_POINT('Ctrl Pts',(10.8978669207609,-28.154266978122,-5.42724118013789));
#38265=CARTESIAN_POINT('Ctrl Pts',(11.0245498979363,-28.1654111536866,-5.1728625408699));
#38266=CARTESIAN_POINT('Ctrl Pts',(11.1423306648156,-28.1765553292512,-4.91402981929681));
#38267=CARTESIAN_POINT('Ctrl Pts',(11.250913280774,-28.1876995048158,-4.65138695428623));
#38268=CARTESIAN_POINT('Ctrl Pts',(11.3629153838978,-28.1991946331086,-4.38047293188917));
#38269=CARTESIAN_POINT('Ctrl Pts',(11.4651304890387,-28.2106897614015,-4.10550516952863));
#38270=CARTESIAN_POINT('Ctrl Pts',(11.5572874357625,-28.2221848896944,-3.82721274260596));
#38271=CARTESIAN_POINT('Ctrl Pts',(11.6466355538357,-28.2333296608319,-3.55740232132468));
#38272=CARTESIAN_POINT('Ctrl Pts',(11.7265294669145,-28.2444744319695,-3.28446716262288));
#38273=CARTESIAN_POINT('Ctrl Pts',(11.7967723708194,-28.2556192031071,-3.00908821423886));
#38274=CARTESIAN_POINT('Ctrl Pts',(11.8703276043836,-28.2672895099776,-2.72072367147365));
#38275=CARTESIAN_POINT('Ctrl Pts',(11.9332996556248,-28.2789598168481,-2.42967962578353));
#38276=CARTESIAN_POINT('Ctrl Pts',(11.9855220652797,-28.2906301237186,-2.13675245938659));
#38277=CARTESIAN_POINT('Ctrl Pts',(12.0377444749345,-28.3023004305891,-1.84382529298966));
#38278=CARTESIAN_POINT('Ctrl Pts',(12.0792171927608,-28.3139707374596,-1.54901533771966));
#38279=CARTESIAN_POINT('Ctrl Pts',(12.1098355954862,-28.3256410443301,-1.25312892405157));
#38280=CARTESIAN_POINT('Ctrl Pts',(12.1390818454577,-28.3367883505772,-0.970502554057997));
#38281=CARTESIAN_POINT('Ctrl Pts',(12.1584339953508,-28.3479356568243,-0.686809677550053));
#38282=CARTESIAN_POINT('Ctrl Pts',(12.1678361799058,-28.3590829630714,-0.40275668706502));
#38283=CARTESIAN_POINT('Ctrl Pts',(12.177236767501,-28.37022837595,-0.118751942944197));
#38284=CARTESIAN_POINT('Ctrl Pts',(12.1766907550221,-28.3813737888286,0.165612526537045));
#38285=CARTESIAN_POINT('Ctrl Pts',(12.1661943454187,-28.3925192017072,0.449628067964166));
#38286=CARTESIAN_POINT('Ctrl Pts',(12.1556991010799,-28.4036633772718,0.733612079254089));
#38287=CARTESIAN_POINT('Ctrl Pts',(12.1352556752733,-28.4148075528364,1.0172469733435));
#38288=CARTESIAN_POINT('Ctrl Pts',(12.104912365353,-28.425951728401,1.29982571028703));
#38289=CARTESIAN_POINT('Ctrl Pts',(12.07361348296,-28.4374468566938,1.59130342572396));
#38290=CARTESIAN_POINT('Ctrl Pts',(12.0317810995415,-28.4489419849867,1.88165708895882));
#38291=CARTESIAN_POINT('Ctrl Pts',(11.9795260125188,-28.4604371132795,2.1701167630765));
#38292=CARTESIAN_POINT('Ctrl Pts',(11.9288635952924,-28.4715818844171,2.44978454655556));
#38293=CARTESIAN_POINT('Ctrl Pts',(11.8684044580646,-28.4827266555547,2.727671809539));
#38294=CARTESIAN_POINT('Ctrl Pts',(11.7983016566862,-28.4938714266923,3.00308645693653));
#38295=CARTESIAN_POINT('Ctrl Pts',(11.7248931322342,-28.5055417335628,3.29148838211453));
#38296=CARTESIAN_POINT('Ctrl Pts',(11.6409096368336,-28.5172120404333,3.57717857842725));
#38297=CARTESIAN_POINT('Ctrl Pts',(11.5465861114499,-28.5288823473038,3.85937811322915));
#38298=CARTESIAN_POINT('Ctrl Pts',(11.4522625860663,-28.5405526541742,4.14157764803105));
#38299=CARTESIAN_POINT('Ctrl Pts',(11.3475991453805,-28.5522229610447,4.42028620590779));
#38300=CARTESIAN_POINT('Ctrl Pts',(11.2328897869991,-28.5638932679152,4.6947457101671));
#38301=CARTESIAN_POINT('Ctrl Pts',(11.1233210874371,-28.5750405741623,4.95690541002459));
#38302=CARTESIAN_POINT('Ctrl Pts',(11.0045543630941,-28.5861878804094,5.21526682176328));
#38303=CARTESIAN_POINT('Ctrl Pts',(10.8768785996751,-28.5973351866565,5.46918295341547));
#38304=CARTESIAN_POINT('Ctrl Pts',(10.7492245219682,-28.6084805995351,5.72305595744509));
#38305=CARTESIAN_POINT('Ctrl Pts',(10.6126645460732,-28.6196260124137,5.97248495058034));
#38306=CARTESIAN_POINT('Ctrl Pts',(10.467534458856,-28.6307714252922,6.21684587251955));
#38307=CARTESIAN_POINT('Ctrl Pts',(10.3224204833328,-28.6419156008568,6.46117966660059));
#38308=CARTESIAN_POINT('Ctrl Pts',(10.1687384324912,-28.6530597764214,6.70044628368926));
#38309=CARTESIAN_POINT('Ctrl Pts',(10.0068690633192,-28.664203951986,6.93404800961067));
#38310=CARTESIAN_POINT('Ctrl Pts',(9.83990209886954,-28.6756990802789,7.17500632845005));
#38311=CARTESIAN_POINT('Ctrl Pts',(9.66422395039496,-28.6871942085718,7.40993692714886));
#38312=CARTESIAN_POINT('Ctrl Pts',(9.48030035284617,-28.6986893368646,7.63821677290091));
#38313=CARTESIAN_POINT('Ctrl Pts',(9.30198251686694,-28.7098341080022,7.85953893403023));
#38314=CARTESIAN_POINT('Ctrl Pts',(9.11591458607458,-28.7209788791398,8.0746095348416));
#38315=CARTESIAN_POINT('Ctrl Pts',(8.92256215039984,-28.7321236502774,8.28289411511775));
#38316=CARTESIAN_POINT('Ctrl Pts',(8.72009211035867,-28.7437939571479,8.50100043046518));
#38317=CARTESIAN_POINT('Ctrl Pts',(8.50963424411612,-28.7554642640184,8.71166509837527));
#38318=CARTESIAN_POINT('Ctrl Pts',(8.29176759747592,-28.7671345708889,8.91431659519946));
#38319=CARTESIAN_POINT('Ctrl Pts',(8.07390095083574,-28.7788048777594,9.11696809202363));
#38320=CARTESIAN_POINT('Ctrl Pts',(7.84862577543433,-28.7904751846298,9.31160619568754));
#38321=CARTESIAN_POINT('Ctrl Pts',(7.61656299213793,-28.8021454915003,9.49770595653471));
#38322=CARTESIAN_POINT('Ctrl Pts',(7.39490001937541,-28.8132927977474,9.67546572324013));
#38323=CARTESIAN_POINT('Ctrl Pts',(7.16697823266025,-28.8244401039945,9.84548870117944));
#38324=CARTESIAN_POINT('Ctrl Pts',(6.93336099330269,-28.8355874102417,10.0073450818161));
#38325=CARTESIAN_POINT('Ctrl Pts',(6.69978343380329,-28.8467328231202,10.1691739711672));
#38326=CARTESIAN_POINT('Ctrl Pts',(6.46051257220027,-28.8578782359988,10.322838880697));
#38327=CARTESIAN_POINT('Ctrl Pts',(6.21614189045026,-28.8690236488774,10.4679525336997));
#38328=CARTESIAN_POINT('Ctrl Pts',(5.97179833764223,-28.880167824442,10.6130500768326));
#38329=CARTESIAN_POINT('Ctrl Pts',(5.72235632451466,-28.8913120000066,10.7495981229215));
#38330=CARTESIAN_POINT('Ctrl Pts',(5.46843621193528,-28.9024561755712,10.8772540489774));
#38331=CARTESIAN_POINT('Ctrl Pts',(5.20651963916458,-28.913951303864,11.0089301194816));
#38332=CARTESIAN_POINT('Ctrl Pts',(4.93983860834533,-28.9254464321569,11.1311447906859));
#38333=CARTESIAN_POINT('Ctrl Pts',(4.66910021250522,-28.9369415604497,11.2435738737994));
#38334=CARTESIAN_POINT('Ctrl Pts',(4.40661358487193,-28.9480863315874,11.3525762588611));
#38335=CARTESIAN_POINT('Ctrl Pts',(4.14031351438129,-28.959231102725,11.4523806207877));
#38336=CARTESIAN_POINT('Ctrl Pts',(3.87086458095801,-28.9703758738626,11.5427404738166));
#38337=CARTESIAN_POINT('Ctrl Pts',(3.58870968516497,-28.9820461807331,11.6373612785507));
#38338=CARTESIAN_POINT('Ctrl Pts',(3.30310211058093,-28.9937164876035,11.7216253225378));
#38339=CARTESIAN_POINT('Ctrl Pts',(3.01482379511475,-29.005386794474,11.7953078694204));
#38340=CARTESIAN_POINT('Ctrl Pts',(2.72654547964853,-29.0170571013445,11.868990416303));
#38341=CARTESIAN_POINT('Ctrl Pts',(2.43559675052517,-29.0287274082149,11.9320913915042));
#38342=CARTESIAN_POINT('Ctrl Pts',(2.14277402700613,-29.0403977150854,11.9844469926312));
#38343=CARTESIAN_POINT('Ctrl Pts',(1.86307404898437,-29.0515450213325,12.0344562962418));
#38344=CARTESIAN_POINT('Ctrl Pts',(1.58158081379775,-29.0626923275796,12.0746770922416));
#38345=CARTESIAN_POINT('Ctrl Pts',(1.29899467062888,-29.0738396338267,12.1050015735512));
#38346=CARTESIAN_POINT('Ctrl Pts',(1.01645652468036,-29.0849850467053,12.1353209042516));
#38347=CARTESIAN_POINT('Ctrl Pts',(0.732826106484331,-29.0961304595838,
12.1557472477031));
#38348=CARTESIAN_POINT('Ctrl Pts',(0.448809859789771,-29.1072758724624,
12.1662245565235));
#38349=CARTESIAN_POINT('Ctrl Pts',(0.164825143310763,-29.118420048027,12.1767007021999));
#38350=CARTESIAN_POINT('Ctrl Pts',(-0.119545049638622,-29.1295642235916,
12.1772300089198));
#38351=CARTESIAN_POINT('Ctrl Pts',(-0.403592042607901,-29.1407083991562,
12.1678085008412));
#38352=CARTESIAN_POINT('Ctrl Pts',(-0.696584252436126,-29.152203527449,
12.1580902903332));
#38353=CARTESIAN_POINT('Ctrl Pts',(-0.989232279100445,-29.1636986557419,
12.1377843664195));
#38354=CARTESIAN_POINT('Ctrl Pts',(-1.28076011128974,-29.1751937840348,
12.1069444447114));
#38355=CARTESIAN_POINT('Ctrl Pts',(-1.56340253921341,-29.1863385551724,
12.0770444853042));
#38356=CARTESIAN_POINT('Ctrl Pts',(-1.84499176824494,-29.19748332631,12.0372431750742));
#38357=CARTESIAN_POINT('Ctrl Pts',(-2.12482630052757,-29.2086280974475,
11.9876421135512));
#38358=CARTESIAN_POINT('Ctrl Pts',(-2.41785653186929,-29.220298404318,11.9357020959475));
#38359=CARTESIAN_POINT('Ctrl Pts',(-2.70896228484959,-29.2319687111885,
11.8730159224245));
#38360=CARTESIAN_POINT('Ctrl Pts',(-2.99734942177683,-29.243639018059,11.7997604506945));
#38361=CARTESIAN_POINT('Ctrl Pts',(-3.28573655870407,-29.2553093249295,
11.7265049789645));
#38362=CARTESIAN_POINT('Ctrl Pts',(-3.57140475656548,-29.2669796318,11.6426803001354));
#38363=CARTESIAN_POINT('Ctrl Pts',(-3.85357632161499,-29.2786499386705,
11.5485237058028));
#38364=CARTESIAN_POINT('Ctrl Pts',(-4.12310246901941,-29.2897972449176,
11.4585867055287));
#38365=CARTESIAN_POINT('Ctrl Pts',(-4.38951899259722,-29.3009445511647,
11.3591966162271));
#38366=CARTESIAN_POINT('Ctrl Pts',(-4.65215935045579,-29.3120918574118,
11.2505939233432));
#38367=CARTESIAN_POINT('Ctrl Pts',(-4.91475509888341,-29.3232372702904,
11.1420096766126));
#38368=CARTESIAN_POINT('Ctrl Pts',(-5.17357571569862,-29.334382683169,11.0242160522334));
#38369=CARTESIAN_POINT('Ctrl Pts',(-5.42797407681309,-29.3455280960475,
10.897501900502));
#38370=CARTESIAN_POINT('Ctrl Pts',(-5.68234419575679,-29.3566722716121,
10.7708018160103));
#38371=CARTESIAN_POINT('Ctrl Pts',(-5.93229280062053,-29.3678164471767,
10.6351833005706));
#38372=CARTESIAN_POINT('Ctrl Pts',(-6.17719572531623,-29.3789606227413,
10.490981995082));
#38373=CARTESIAN_POINT('Ctrl Pts',(-6.42981114063899,-29.3904557510341,
10.3422394975339));
#38374=CARTESIAN_POINT('Ctrl Pts',(-6.67705766802854,-29.401950879327,10.1843650133689));
#38375=CARTESIAN_POINT('Ctrl Pts',(-6.91827962488474,-29.4134460076198,
10.017777062897));
#38376=CARTESIAN_POINT('Ctrl Pts',(-7.15214943773357,-29.4245907787574,
9.85626650512062));
#38377=CARTESIAN_POINT('Ctrl Pts',(-7.38035625506918,-29.435735549895,9.68656592549823));
#38378=CARTESIAN_POINT('Ctrl Pts',(-7.60233273639396,-29.4468803210326,
9.50910023162826));
#38379=CARTESIAN_POINT('Ctrl Pts',(-7.83477659935983,-29.4585506279031,
9.32326607847446));
#38380=CARTESIAN_POINT('Ctrl Pts',(-8.06038815211743,-29.4702209347736,
9.12891705472717));
#38381=CARTESIAN_POINT('Ctrl Pts',(-8.27855472469325,-29.4818912416441,
8.92658848162383));
#38382=CARTESIAN_POINT('Ctrl Pts',(-8.49672129726908,-29.4935615485146,
8.72425990852047));
#38383=CARTESIAN_POINT('Ctrl Pts',(-8.70744264963618,-29.5052318553851,
8.51395202063506));
#38384=CARTESIAN_POINT('Ctrl Pts',(-8.91014947085614,-29.5169021622556,
8.29624533490916));
#38385=CARTESIAN_POINT('Ctrl Pts',(-9.10377205847044,-29.5280494685027,
8.08829509634546));
#38386=CARTESIAN_POINT('Ctrl Pts',(-9.29014048970121,-29.5391967747498,
7.87353252575311));
#38387=CARTESIAN_POINT('Ctrl Pts',(-9.46878458047568,-29.550344080997,7.65248775357047));
#38388=CARTESIAN_POINT('Ctrl Pts',(-9.64739832857408,-29.5614894938755,
7.43148052581425));
#38389=CARTESIAN_POINT('Ctrl Pts',(-9.81829018797549,-29.5726349067541,
7.2041934341806));
#38390=CARTESIAN_POINT('Ctrl Pts',(-9.98103016933431,-29.5837803196327,
6.97118978430787));
#38391=CARTESIAN_POINT('Ctrl Pts',(-10.143752084027,-29.5949244951972,6.73821200146009));
#38392=CARTESIAN_POINT('Ctrl Pts',(-10.2983237750866,-29.6060686707618,
6.49951914625352));
#38393=CARTESIAN_POINT('Ctrl Pts',(-10.4443578030689,-29.6172128463264,
6.2557046230999));
#38394=CARTESIAN_POINT('Ctrl Pts',(-10.594990739265,-29.6287079746193,6.00421188529549));
#38395=CARTESIAN_POINT('Ctrl Pts',(-10.7365394011799,-29.6402031029121,
5.74726991837197));
#38396=CARTESIAN_POINT('Ctrl Pts',(-10.868628337183,-29.651698231205,5.48555998218799));
#38397=CARTESIAN_POINT('Ctrl Pts',(-10.9966913673694,-29.6628430023426,
5.23182663803549));
#38398=CARTESIAN_POINT('Ctrl Pts',(-11.1158626482813,-29.6739877734802,
4.97361191341933));
#38399=CARTESIAN_POINT('Ctrl Pts',(-11.2258473549232,-29.6851325446178,
4.71156040117959));
#38400=CARTESIAN_POINT('Ctrl Pts',(-11.341018430374,-29.6968028514883,4.43715175465375));
#38401=CARTESIAN_POINT('Ctrl Pts',(-11.4461155690856,-29.7084731583587,
4.15853605659713));
#38402=CARTESIAN_POINT('Ctrl Pts',(-11.5408569815104,-29.7201434652292,
3.8764765422123));
#38403=CARTESIAN_POINT('Ctrl Pts',(-11.6355983939352,-29.7318137720997,
3.59441702782744));
#38404=CARTESIAN_POINT('Ctrl Pts',(-11.7199839815676,-29.7434840789702,
3.30891401794856));
#38405=CARTESIAN_POINT('Ctrl Pts',(-11.7937916549543,-29.7551543858407,
3.02074968336178));
#38406=CARTESIAN_POINT('Ctrl Pts',(-11.8651552549867,-29.7664382412116,
2.74212764620159));
#38407=CARTESIAN_POINT('Ctrl Pts',(-11.9266493212993,-29.7777220965825,
2.46094394049381));
#38408=CARTESIAN_POINT('Ctrl Pts',(-11.9781123416308,-29.7890059519535,
2.17790610019643));
#38409=CARTESIAN_POINT('Ctrl Pts',(-12.0295653763274,-29.8002876178598,
1.89492317918895));
#38410=CARTESIAN_POINT('Ctrl Pts',(-12.0709912069458,-29.8115692837662,
1.61008709067454));
#38411=CARTESIAN_POINT('Ctrl Pts',(-12.1022795090425,-29.8228509496725,
1.32411515171836));
#38412=CARTESIAN_POINT('Ctrl Pts',(-12.1335625490621,-29.8341307182245,
1.03819130761862));
#38413=CARTESIAN_POINT('Ctrl Pts',(-12.1547114378685,-29.8454104867765,
0.751132245746415));
#38414=CARTESIAN_POINT('Ctrl Pts',(-12.1656676092229,-29.8566902553285,
0.463661376334469));
#38415=CARTESIAN_POINT('Ctrl Pts',(-12.1715549693444,-29.8627515022189,
0.309187292468078));
#38416=CARTESIAN_POINT('Ctrl Pts',(-12.1745000598421,-29.8688127491093,
0.154594386717212));
#38417=CARTESIAN_POINT('Ctrl Pts',(-12.1744999999991,-29.8748739959996,
-4.71256420053583E-6));
#38418=CARTESIAN_POINT('Ctrl Pts',(-12.1734593809614,-29.8748739960349,
-4.71306082890088E-6));
#38419=CARTESIAN_POINT('Ctrl Pts',(-12.1734729483294,-29.9143848671652,
-1.00768895467666));
#38420=CARTESIAN_POINT('Ctrl Pts',(-11.8010964029253,-30.0333131461572,
-4.04082287428804));
#38421=CARTESIAN_POINT('Ctrl Pts',(-9.30992091872449,-30.2316588330109,
-8.62536224638919));
#38422=CARTESIAN_POINT('Ctrl Pts',(-4.04710485413492,-30.469911056596,-12.0288172192438));
#38423=CARTESIAN_POINT('Ctrl Pts',(2.1241845520127,-30.7051707337015,-12.4928842203625));
#38424=CARTESIAN_POINT('Ctrl Pts',(5.86746336791747,-30.8610130029453,-10.8440791401043));
#38425=CARTESIAN_POINT('Ctrl Pts',(7.41333450932841,-30.9374378643275,-9.65843860955958));
#38426=CARTESIAN_POINT('',(-12.1744999986658,-29.6251260039304,0.000180241411394071));
#38427=CARTESIAN_POINT('Ctrl Pts',(-12.1744999986658,-29.6251260039651,
0.00018024052605028));
#38428=CARTESIAN_POINT('Ctrl Pts',(-12.1745042222142,-29.6363114795878,
-0.285102936417017));
#38429=CARTESIAN_POINT('Ctrl Pts',(-12.1644766085762,-29.6474969552104,
-0.570385273907491));
#38430=CARTESIAN_POINT('Ctrl Pts',(-12.1444433863984,-29.6586824308331,
-0.854953264549404));
#38431=CARTESIAN_POINT('Ctrl Pts',(-12.1244071877467,-29.6698695683589,
-1.13956353541974));
#38432=CARTESIAN_POINT('Ctrl Pts',(-12.0943624266308,-29.6810567058848,
-1.42345898533909));
#38433=CARTESIAN_POINT('Ctrl Pts',(-12.0543873318725,-29.6922438434107,
-1.70592974743708));
#38434=CARTESIAN_POINT('Ctrl Pts',(-12.0144104223308,-29.7034314888086,
-1.98841333310159));
#38435=CARTESIAN_POINT('Ctrl Pts',(-11.9645023183561,-29.7146191342066,
-2.2694718422521));
#38436=CARTESIAN_POINT('Ctrl Pts',(-11.9047927944751,-29.7258067796045,
-2.54840318054546));
#38437=CARTESIAN_POINT('Ctrl Pts',(-11.8450710809749,-29.7369967089452,
-2.8273914622972));
#38438=CARTESIAN_POINT('Ctrl Pts',(-11.7755440050082,-29.7481866382859,
-3.10425144891475));
#38439=CARTESIAN_POINT('Ctrl Pts',(-11.6963922226106,-29.7593765676266,
-3.37829235337227));
#38440=CARTESIAN_POINT('Ctrl Pts',(-11.6752552402276,-29.7623647674141,
-3.4514732419674));
#38441=CARTESIAN_POINT('Ctrl Pts',(-11.6534321750649,-29.7653529672017,
-3.52445317187036));
#38442=CARTESIAN_POINT('Ctrl Pts',(-11.6309270707671,-29.7683411669892,
-3.59721916547995));
#38443=CARTESIAN_POINT('Ctrl Pts',(-11.5469730825569,-29.7794884732363,
-3.86866849043174));
#38444=CARTESIAN_POINT('Ctrl Pts',(-11.4534995431357,-29.7906357794834,
-4.13721802276228));
#38445=CARTESIAN_POINT('Ctrl Pts',(-11.3507321374569,-29.8017830857305,
-4.40219606488654));
#38446=CARTESIAN_POINT('Ctrl Pts',(-11.247982186809,-29.8129284986091,-4.66712910052394));
#38447=CARTESIAN_POINT('Ctrl Pts',(-11.1359416179192,-29.8240739114877,
-4.92849160846213));
#38448=CARTESIAN_POINT('Ctrl Pts',(-11.0148848982189,-29.8352193243662,
-5.18563023450271));
#38449=CARTESIAN_POINT('Ctrl Pts',(-10.8938416176952,-29.8463634999308,
-5.44274031416114));
#38450=CARTESIAN_POINT('Ctrl Pts',(-10.7637842986543,-29.8575076754954,
-5.69562720699591));
#38451=CARTESIAN_POINT('Ctrl Pts',(-10.6250346954393,-29.86865185106,-5.94365947634216));
#38452=CARTESIAN_POINT('Ctrl Pts',(-10.4819155853449,-29.8801469793528,
-6.19950278573525));
#38453=CARTESIAN_POINT('Ctrl Pts',(-10.329547980573,-29.8916421076457,-6.45018048931594));
#38454=CARTESIAN_POINT('Ctrl Pts',(-10.1683357975651,-29.9031372359385,
-6.69502780860221));
#38455=CARTESIAN_POINT('Ctrl Pts',(-10.0120371605734,-29.9142820070761,
-6.93241248736197));
#38456=CARTESIAN_POINT('Ctrl Pts',(-9.84742525859584,-29.9254267782137,
-7.16431669157156));
#38457=CARTESIAN_POINT('Ctrl Pts',(-9.67491234763068,-29.9365715493513,
-7.39016382197738));
#38458=CARTESIAN_POINT('Ctrl Pts',(-9.49426452765975,-29.9482418562218,
-7.62666085588776));
#38459=CARTESIAN_POINT('Ctrl Pts',(-9.30495281210028,-29.9599121630923,
-7.85651557113396));
#38460=CARTESIAN_POINT('Ctrl Pts',(-9.10749884104637,-29.9715824699628,
-8.07910360809534));
#38461=CARTESIAN_POINT('Ctrl Pts',(-8.91004486999248,-29.9832527768333,
-8.30169164505669));
#38462=CARTESIAN_POINT('Ctrl Pts',(-8.70444887265217,-29.9949230837037,
-8.51701275857697));
#38463=CARTESIAN_POINT('Ctrl Pts',(-8.49127863272491,-30.0065933905742,
-8.7244849378877));
#38464=CARTESIAN_POINT('Ctrl Pts',(-8.28766154076552,-30.0177406968213,
-8.92265932577667));
#38465=CARTESIAN_POINT('Ctrl Pts',(-8.07707334551595,-30.0288880030684,
-9.11373199757563));
#38466=CARTESIAN_POINT('Ctrl Pts',(-7.86003364885051,-30.0400353093155,
-9.29722115951523));
#38467=CARTESIAN_POINT('Ctrl Pts',(-7.64303081634977,-30.0511807221941,
-9.48067915584417));
#38468=CARTESIAN_POINT('Ctrl Pts',(-7.41957887379889,-30.0623261350727,
-9.656556041771));
#38469=CARTESIAN_POINT('Ctrl Pts',(-7.19023147912979,-30.0734715479513,
-9.82440947469776));
#38470=CARTESIAN_POINT('Ctrl Pts',(-6.96090954558389,-30.0846157235159,
-9.99224427328623));
#38471=CARTESIAN_POINT('Ctrl Pts',(-6.72569368202658,-30.0957598990805,
-10.1520572400168));
#38472=CARTESIAN_POINT('Ctrl Pts',(-6.48516857886181,-30.1069040746452,
-10.3034479061013));
#38473=CARTESIAN_POINT('Ctrl Pts',(-6.2370688515653,-30.118399202938,-10.4596061718149));
#38474=CARTESIAN_POINT('Ctrl Pts',(-5.98332031440759,-30.1298943312309,
-10.6068029039343));
#38475=CARTESIAN_POINT('Ctrl Pts',(-5.72459575688008,-30.1413894595237,
-10.7446476754853));
#38476=CARTESIAN_POINT('Ctrl Pts',(-5.47375680077022,-30.1525342306613,
-10.8782911105402));
#38477=CARTESIAN_POINT('Ctrl Pts',(-5.21824090472264,-30.1636790017989,
-11.0031440843534));
#38478=CARTESIAN_POINT('Ctrl Pts',(-4.95868598336946,-30.1748237729366,
-11.1188975878158));
#38479=CARTESIAN_POINT('Ctrl Pts',(-4.68689165538149,-30.186494079807,-11.240109489797));
#38480=CARTESIAN_POINT('Ctrl Pts',(-4.4106685032706,-30.1981643866775,-11.3513429650037));
#38481=CARTESIAN_POINT('Ctrl Pts',(-4.13077334331136,-30.2098346935479,
-11.4522994126153));
#38482=CARTESIAN_POINT('Ctrl Pts',(-3.85087818335214,-30.2215050004184,
-11.5532558602268));
#38483=CARTESIAN_POINT('Ctrl Pts',(-3.56731133412171,-30.2331753072889,
-11.643935174666));
#38484=CARTESIAN_POINT('Ctrl Pts',(-3.28084986321212,-30.2448456141593,
-11.7240980218122));
#38485=CARTESIAN_POINT('Ctrl Pts',(-3.0072260605414,-30.2559929204064,-11.8006683996693));
#38486=CARTESIAN_POINT('Ctrl Pts',(-2.73087965548585,-30.2671402266535,
-11.8676670436835));
#38487=CARTESIAN_POINT('Ctrl Pts',(-2.45249745078426,-30.2782875329007,
-11.9249195596405));
#38488=CARTESIAN_POINT('Ctrl Pts',(-2.17416252926519,-30.2894329457792,
-11.9821623512649));
#38489=CARTESIAN_POINT('Ctrl Pts',(-1.89379275963015,-30.3005783586578,
-12.0296622660804));
#38490=CARTESIAN_POINT('Ctrl Pts',(-1.61208596895547,-30.3117237715363,
-12.0672958478152));
#38491=CARTESIAN_POINT('Ctrl Pts',(-1.3304104521108,-30.3228679471009,-12.1049252516377));
#38492=CARTESIAN_POINT('Ctrl Pts',(-1.04739847494835,-30.3340121226655,
-12.1326904742396));
#38493=CARTESIAN_POINT('Ctrl Pts',(-0.763755074643579,-30.3451562982301,
-12.1505196776087));
#38494=CARTESIAN_POINT('Ctrl Pts',(-0.471179167432488,-30.3566514265229,
-12.1689103588125));
#38495=CARTESIAN_POINT('Ctrl Pts',(-0.177931718560926,-30.3681465548158,
-12.1767290407253));
#38496=CARTESIAN_POINT('Ctrl Pts',(0.115209683570617,-30.3796416831087,
-12.1739548618685));
#38497=CARTESIAN_POINT('Ctrl Pts',(0.399416501839786,-30.3907864542462,
-12.1712652365189));
#38498=CARTESIAN_POINT('Ctrl Pts',(0.683523362929896,-30.4019312253839,
-12.1586189056608));
#38499=CARTESIAN_POINT('Ctrl Pts',(0.96682226273384,-30.4130759965214,-12.136049808825));
#38500=CARTESIAN_POINT('Ctrl Pts',(1.26348022510615,-30.4247463033919,-12.1124164580266));
#38501=CARTESIAN_POINT('Ctrl Pts',(1.55925187642787,-30.4364166102624,-12.0779020256309));
#38502=CARTESIAN_POINT('Ctrl Pts',(1.85332979011717,-30.4480869171329,-12.0326064898286));
#38503=CARTESIAN_POINT('Ctrl Pts',(2.14740770380649,-30.4597572240034,-11.9873109540262));
#38504=CARTESIAN_POINT('Ctrl Pts',(2.43979154960903,-30.4714275308739,-11.9312343745664));
#38505=CARTESIAN_POINT('Ctrl Pts',(2.72968448063129,-30.4830978377444,-11.8645384607325));
#38506=CARTESIAN_POINT('Ctrl Pts',(3.00658378215355,-30.494245056166,-11.8008320023174));
#38507=CARTESIAN_POINT('Ctrl Pts',(3.28129325471924,-30.5053922745877,-11.7274182178329));
#38508=CARTESIAN_POINT('Ctrl Pts',(3.55312640247246,-30.5165394930093,-11.6444726380396));
#38509=CARTESIAN_POINT('Ctrl Pts',(3.82491258716696,-30.5276847855897,-11.5615413882799));
#38510=CARTESIAN_POINT('Ctrl Pts',(4.09382318417072,-30.5388300781702,-11.4690817088839));
#38511=CARTESIAN_POINT('Ctrl Pts',(4.35918639889116,-30.5499753707506,-11.3673191294044));
#38512=CARTESIAN_POINT('Ctrl Pts',(4.63242020081986,-30.5614512291078,-11.2625383046975));
#38513=CARTESIAN_POINT('Ctrl Pts',(4.90189269707538,-30.5729270874651,-11.147894395897));
#38514=CARTESIAN_POINT('Ctrl Pts',(5.16689067451331,-30.5844029458224,-11.0236877227009));
#38515=CARTESIAN_POINT('Ctrl Pts',(5.42422969768999,-30.5955471296698,-10.9030708626731));
#38516=CARTESIAN_POINT('Ctrl Pts',(5.67734896602108,-30.6066913135173,-10.7734363698508));
#38517=CARTESIAN_POINT('Ctrl Pts',(5.92561758210199,-30.6178354973647,-10.6351072641833));
#38518=CARTESIAN_POINT('Ctrl Pts',(6.18496969779133,-30.6294771929769,-10.4906027078578));
#38519=CARTESIAN_POINT('Ctrl Pts',(6.43902791382879,-30.6411188885891,-10.3366096758748));
#38520=CARTESIAN_POINT('Ctrl Pts',(6.68710279673228,-30.6527605842012,-10.1735493529021));
#38521=CARTESIAN_POINT('Ctrl Pts',(6.93517767963574,-30.6644022798134,-10.0104890299294));
#38522=CARTESIAN_POINT('Ctrl Pts',(7.17726895509336,-30.6760439754256,-9.8383616025104));
#38523=CARTESIAN_POINT('Ctrl Pts',(7.41272179941101,-30.6876856710377,-9.65763976210217));
#38524=CARTESIAN_POINT('Ctrl Pts',(7.412721799411,-27.6877007372717,-9.65763976210218));
#38525=CARTESIAN_POINT('Ctrl Pts',(7.63814987596554,-27.6988450042982,-9.48461243260574));
#38526=CARTESIAN_POINT('Ctrl Pts',(7.85753273411191,-27.7099892713247,-9.303676776569));
#38527=CARTESIAN_POINT('Ctrl Pts',(8.07032180364135,-27.7211335383512,-9.11528146771514));
#38528=CARTESIAN_POINT('Ctrl Pts',(8.28309854906444,-27.7322771599351,-8.926897070154));
#38529=CARTESIAN_POINT('Ctrl Pts',(8.48928206907873,-27.743420781519,-8.73105405962382));
#38530=CARTESIAN_POINT('Ctrl Pts',(8.68835826132702,-27.7545644031029,-8.5282402037484));
#38531=CARTESIAN_POINT('Ctrl Pts',(8.88745493347408,-27.7657091710832,-8.32540548346328));
#38532=CARTESIAN_POINT('Ctrl Pts',(9.07944262860806,-27.7768539390636,-8.11559867393501));
#38533=CARTESIAN_POINT('Ctrl Pts',(9.26384437461779,-27.7879987070439,-7.89934412801863));
#38534=CARTESIAN_POINT('Ctrl Pts',(9.44825126409226,-27.7991437858821,-7.68308355017654));
#38535=CARTESIAN_POINT('Ctrl Pts',(9.62507161081348,-27.8102888647202,-7.46037508148394));
#38536=CARTESIAN_POINT('Ctrl Pts',(9.79386837211311,-27.8214339435584,-7.23177658391923));
#38537=CARTESIAN_POINT('Ctrl Pts',(9.96269728861601,-27.8325811454958,-7.00313453912589));
#38538=CARTESIAN_POINT('Ctrl Pts',(10.1234994079084,-27.8437283474331,-6.76860043865689));
#38539=CARTESIAN_POINT('Ctrl Pts',(10.2758798621779,-27.8548755493705,-6.52876277008793));
#38540=CARTESIAN_POINT('Ctrl Pts',(10.309816736,-27.8573581590165,-6.47534817216571));
#38541=CARTESIAN_POINT('Ctrl Pts',(10.3433360636503,-27.8598407686624,-6.42167062675943));
#38542=CARTESIAN_POINT('Ctrl Pts',(10.3764337811701,-27.8623233783083,-6.36773682205794));
#38543=CARTESIAN_POINT('Ctrl Pts',(10.5250477180731,-27.8734706845554,-6.12556558943234));
#38544=CARTESIAN_POINT('Ctrl Pts',(10.6652022492297,-27.8846179908025,-5.87815325893287));
#38545=CARTESIAN_POINT('Ctrl Pts',(10.7965414680425,-27.8957652970496,-5.6261125636481));
#38546=CARTESIAN_POINT('Ctrl Pts',(10.9278583789056,-27.9069107099282,-5.37411467744341));
#38547=CARTESIAN_POINT('Ctrl Pts',(11.0503628435202,-27.9180561228068,-5.11749023242213));
#38548=CARTESIAN_POINT('Ctrl Pts',(11.1637449230493,-27.9292015356854,-4.85687652129331));
#38549=CARTESIAN_POINT('Ctrl Pts',(11.2771144154064,-27.94034571125,-4.59629174233473));
#38550=CARTESIAN_POINT('Ctrl Pts',(11.3813634385435,-27.9514898868146,-4.33171882614915));
#38551=CARTESIAN_POINT('Ctrl Pts',(11.4762297207818,-27.9626340623792,-4.06381614321381));
#38552=CARTESIAN_POINT('Ctrl Pts',(11.5740835349713,-27.9741291906721,-3.78747666054088));
#38553=CARTESIAN_POINT('Ctrl Pts',(11.6619539607177,-27.9856243189649,-3.50759456690943));
#38554=CARTESIAN_POINT('Ctrl Pts',(11.7396078726037,-27.9971194472578,-3.22491197515566));
#38555=CARTESIAN_POINT('Ctrl Pts',(11.8148949902296,-28.0082642183954,-2.95084519578442));
#38556=CARTESIAN_POINT('Ctrl Pts',(11.8805790712359,-28.019408989533,-2.67414637087701));
#38557=CARTESIAN_POINT('Ctrl Pts',(11.9364987602759,-28.0305537606706,-2.39550570776428));
#38558=CARTESIAN_POINT('Ctrl Pts',(11.9950553625732,-28.0422240675411,-2.10372564292783));
#38559=CARTESIAN_POINT('Ctrl Pts',(12.0429044652634,-28.0538943744115,-1.80981650877131));
#38560=CARTESIAN_POINT('Ctrl Pts',(12.0799209821079,-28.065564681282,-1.51458222491543));
#38561=CARTESIAN_POINT('Ctrl Pts',(12.1169374989523,-28.0772349881525,-1.21934794105955));
#38562=CARTESIAN_POINT('Ctrl Pts',(12.1431213969226,-28.0889052950229,-0.922788841490869));
#38563=CARTESIAN_POINT('Ctrl Pts',(12.158409857211,-28.1005756018934,-0.625715585608539));
#38564=CARTESIAN_POINT('Ctrl Pts',(12.1730131706264,-28.1117229081405,-0.34195556130913));
#38565=CARTESIAN_POINT('Ctrl Pts',(12.1776804928749,-28.1228702143876,-0.0576417030646985));
#38566=CARTESIAN_POINT('Ctrl Pts',(12.1723925340344,-28.1340175206348,0.226517653580774));
#38567=CARTESIAN_POINT('Ctrl Pts',(12.167105473353,-28.1451629335133,0.510628745795714));
#38568=CARTESIAN_POINT('Ctrl Pts',(12.1518665124317,-28.1563083463919,0.794585122204064));
#38569=CARTESIAN_POINT('Ctrl Pts',(12.126708476824,-28.1674537592705,1.07767887987282));
#38570=CARTESIAN_POINT('Ctrl Pts',(12.1015532341492,-28.1785979348351,1.36074120973675));
#38571=CARTESIAN_POINT('Ctrl Pts',(12.0664811392585,-28.1897421103997,1.64294084645477));
#38572=CARTESIAN_POINT('Ctrl Pts',(12.0215769591466,-28.2008862859643,1.92357419022913));
#38573=CARTESIAN_POINT('Ctrl Pts',(11.9752586551788,-28.2123814142571,2.21304524811395));
#38574=CARTESIAN_POINT('Ctrl Pts',(11.9184790037928,-28.22387654255,2.50084946845287));
#38575=CARTESIAN_POINT('Ctrl Pts',(11.8513884385692,-28.2353716708428,2.78622366800464));
#38576=CARTESIAN_POINT('Ctrl Pts',(11.7863427099908,-28.2465164419804,3.06290001832938));
#38577=CARTESIAN_POINT('Ctrl Pts',(11.711605351783,-28.257661213118,3.33729201072506));
#38578=CARTESIAN_POINT('Ctrl Pts',(11.6273649772611,-28.2688059842556,3.60871638336431));
#38579=CARTESIAN_POINT('Ctrl Pts',(11.5391522172666,-28.2804762911261,3.89293987092784));
#38580=CARTESIAN_POINT('Ctrl Pts',(11.4405187337417,-28.2921465979966,4.1739088224095));
#38581=CARTESIAN_POINT('Ctrl Pts',(11.3317394027964,-28.3038169048671,4.4508574855988));
#38582=CARTESIAN_POINT('Ctrl Pts',(11.2229600718511,-28.3154872117375,4.72780614878812));
#38583=CARTESIAN_POINT('Ctrl Pts',(11.1040350243111,-28.327157518608,5.00073421461789));
#38584=CARTESIAN_POINT('Ctrl Pts',(10.9752970363654,-28.3388278254785,5.26889981054376));
#38585=CARTESIAN_POINT('Ctrl Pts',(10.8523283952496,-28.3499751317256,5.52504766131596));
#38586=CARTESIAN_POINT('Ctrl Pts',(10.7203702820013,-28.3611224379727,5.77692701782369));
#38587=CARTESIAN_POINT('Ctrl Pts',(10.5797447276347,-28.3722697442198,6.02390668487535));
#38588=CARTESIAN_POINT('Ctrl Pts',(10.4391430585006,-28.3834151570984,6.27084440246207));
#38589=CARTESIAN_POINT('Ctrl Pts',(10.2898770193584,-28.394560569977,6.51288386038527));
#38590=CARTESIAN_POINT('Ctrl Pts',(10.1323141949373,-28.4057059828556,6.7494191827943));
#38591=CARTESIAN_POINT('Ctrl Pts',(9.97476886243749,-28.4168501584202,6.985928246108));
#38592=CARTESIAN_POINT('Ctrl Pts',(9.80892873173729,-28.4279943339848,7.21693417212102));
#38593=CARTESIAN_POINT('Ctrl Pts',(9.63520493625599,-28.4391385095494,7.44185971960963));
#38594=CARTESIAN_POINT('Ctrl Pts',(9.45601022552987,-28.4506336378422,7.67386862953165));
#38595=CARTESIAN_POINT('Ctrl Pts',(9.26842743224974,-28.4621287661351,7.89940774747275));
#38596=CARTESIAN_POINT('Ctrl Pts',(9.07295386254041,-28.4736238944279,8.1178789383812));
#38597=CARTESIAN_POINT('Ctrl Pts',(8.88343808312846,-28.4847686655655,8.32969140021755));
#38598=CARTESIAN_POINT('Ctrl Pts',(8.68650559273255,-28.4959134367031,8.53486019031293));
#38599=CARTESIAN_POINT('Ctrl Pts',(8.48264897592937,-28.5070582078407,8.73287562038785));
#38600=CARTESIAN_POINT('Ctrl Pts',(8.26917942628165,-28.5187285147112,8.94022854002452));
#38601=CARTESIAN_POINT('Ctrl Pts',(8.04811724601362,-28.5303988215817,9.13973700657199));
#38602=CARTESIAN_POINT('Ctrl Pts',(7.8200702391517,-28.5420691284522,9.33086018032282));
#38603=CARTESIAN_POINT('Ctrl Pts',(7.59202323228978,-28.5537394353226,9.52198335407365));
#38604=CARTESIAN_POINT('Ctrl Pts',(7.35699166160922,-28.5654097421931,9.70472102625269));
#38605=CARTESIAN_POINT('Ctrl Pts',(7.1156227436877,-28.5770800490636,9.87858103269464));
#38606=CARTESIAN_POINT('Ctrl Pts',(6.88507068739089,-28.5882273553107,10.0446495652055));
#38607=CARTESIAN_POINT('Ctrl Pts',(6.64866795349273,-28.5993746615578,10.2026682390773));
#38608=CARTESIAN_POINT('Ctrl Pts',(6.40699935977714,-28.6105219678049,10.3522369299497));
#38609=CARTESIAN_POINT('Ctrl Pts',(6.16537181344141,-28.6216673806835,10.5017802165991));
#38610=CARTESIAN_POINT('Ctrl Pts',(5.91848041970368,-28.632812793562,10.6428762453564));
#38611=CARTESIAN_POINT('Ctrl Pts',(5.66693787905207,-28.6439582064406,10.7751689232682));
#38612=CARTESIAN_POINT('Ctrl Pts',(5.41542326353004,-28.6551023820052,10.9074469146377));
#38613=CARTESIAN_POINT('Ctrl Pts',(5.15925876818901,-28.6662465575698,11.0309233825593));
#38614=CARTESIAN_POINT('Ctrl Pts',(4.89908162917456,-28.6773907331344,11.1452882170307));
#38615=CARTESIAN_POINT('Ctrl Pts',(4.63071098349467,-28.6888858614272,11.2632546324753));
#38616=CARTESIAN_POINT('Ctrl Pts',(4.35807113388033,-28.7003809897201,11.3715260989786));
#38617=CARTESIAN_POINT('Ctrl Pts',(4.0818849802408,-28.711876118013,11.4698153977335));
#38618=CARTESIAN_POINT('Ctrl Pts',(3.81411663566336,-28.7230208891506,11.5651089614059));
#38619=CARTESIAN_POINT('Ctrl Pts',(3.54301522272101,-28.7341656602882,11.6510197413072));
#38620=CARTESIAN_POINT('Ctrl Pts',(3.26925716994285,-28.7453104314257,11.7273359211194));
#38621=CARTESIAN_POINT('Ctrl Pts',(2.98258995670472,-28.7569807382962,11.8072508181233));
#38622=CARTESIAN_POINT('Ctrl Pts',(2.69300983150469,-28.7686510451667,11.8766443830866));
#38623=CARTESIAN_POINT('Ctrl Pts',(2.40130930024363,-28.7803213520372,11.9353325841622));
#38624=CARTESIAN_POINT('Ctrl Pts',(2.10960876898257,-28.7919916589077,11.9940207852378));
#38625=CARTESIAN_POINT('Ctrl Pts',(1.81578816230186,-28.8036619657782,12.0420035648568));
#38626=CARTESIAN_POINT('Ctrl Pts',(1.52065129953035,-28.8153322726487,12.0791584920158));
#38627=CARTESIAN_POINT('Ctrl Pts',(1.2387408895783,-28.8264795788958,12.114648334419));
#38628=CARTESIAN_POINT('Ctrl Pts',(0.955545409716465,-28.8376268851429,
12.1402700844111));
#38629=CARTESIAN_POINT('Ctrl Pts',(0.671769844144579,-28.84877419139,12.1559522673667));
#38630=CARTESIAN_POINT('Ctrl Pts',(0.388042477816734,-28.8599196042686,
12.1716317867055));
#38631=CARTESIAN_POINT('Ctrl Pts',(0.103735488728791,-28.8710650171472,
12.1773750948538));
#38632=CARTESIAN_POINT('Ctrl Pts',(-0.180442727021349,-28.8822104300257,
12.1731627226561));
#38633=CARTESIAN_POINT('Ctrl Pts',(-0.464589394575229,-28.8933546055903,
12.1689508180973));
#38634=CARTESIAN_POINT('Ctrl Pts',(-0.748607050688303,-28.9044987811549,
12.154785444124));
#38635=CARTESIAN_POINT('Ctrl Pts',(-1.03178776018388,-28.9156429567195,
12.1306992489277));
#38636=CARTESIAN_POINT('Ctrl Pts',(-1.32388640551171,-28.9271380850124,
12.1058545305128));
#38637=CARTESIAN_POINT('Ctrl Pts',(-1.61509423925137,-28.9386332133052,
12.0704540273367));
#38638=CARTESIAN_POINT('Ctrl Pts',(-1.90463906234965,-28.9501283415981,
12.0245914813008));
#38639=CARTESIAN_POINT('Ctrl Pts',(-2.1853589208235,-28.9612731127357,11.9801267683949));
#38640=CARTESIAN_POINT('Ctrl Pts',(-2.46451536486775,-28.9724178838733,
11.9258283526593));
#38641=CARTESIAN_POINT('Ctrl Pts',(-2.74141308359914,-28.9835626550109,
11.8618339456878));
#38642=CARTESIAN_POINT('Ctrl Pts',(-3.03136801487868,-28.9952329618814,
11.7948218592007));
#38643=CARTESIAN_POINT('Ctrl Pts',(-3.31884576343249,-29.0069032687519,
11.7171774140972));
#38644=CARTESIAN_POINT('Ctrl Pts',(-3.60306239103901,-29.0185735756223,
11.6291182665016));
#38645=CARTESIAN_POINT('Ctrl Pts',(-3.88727901864551,-29.0302438824928,
11.5410591189059));
#38646=CARTESIAN_POINT('Ctrl Pts',(-4.16823420743118,-29.0419141893633,
11.4425853764951));
#38647=CARTESIAN_POINT('Ctrl Pts',(-4.44516356389173,-29.0535844962338,
11.3339741988523));
#38648=CARTESIAN_POINT('Ctrl Pts',(-4.70968243040855,-29.0647318024809,
11.2302303922428));
#38649=CARTESIAN_POINT('Ctrl Pts',(-4.97060736729662,-29.075879108728,11.117206805338));
#38650=CARTESIAN_POINT('Ctrl Pts',(-5.22728514945102,-29.0870264149751,
10.9951780438667));
#38651=CARTESIAN_POINT('Ctrl Pts',(-5.48391933491689,-29.0981718278537,
10.873170008965));
#38652=CARTESIAN_POINT('Ctrl Pts',(-5.73630756506488,-29.1093172407323,
10.7421599676865));
#38653=CARTESIAN_POINT('Ctrl Pts',(-5.98381850576247,-29.1204626536109,
10.6024698226448));
#38654=CARTESIAN_POINT('Ctrl Pts',(-6.2313019689003,-29.1316068291754,10.4627951853795));
#38655=CARTESIAN_POINT('Ctrl Pts',(-6.47390899154312,-29.14275100474,10.3144424996335));
#38656=CARTESIAN_POINT('Ctrl Pts',(-6.71103358465277,-29.1538951803046,
10.1577792098304));
#38657=CARTESIAN_POINT('Ctrl Pts',(-6.95562571292541,-29.1653903085975,
9.99618227476502));
#38658=CARTESIAN_POINT('Ctrl Pts',(-7.19438425759036,-29.1768854368903,
9.82574297352866));
#38659=CARTESIAN_POINT('Ctrl Pts',(-7.42667603774404,-29.1883805651832,
9.64691314775864));
#38660=CARTESIAN_POINT('Ctrl Pts',(-7.65188785452438,-29.1995253363208,
9.47353383175558));
#38661=CARTESIAN_POINT('Ctrl Pts',(-7.87102104620591,-29.2106701074584,
9.29226805311522));
#38662=CARTESIAN_POINT('Ctrl Pts',(-8.08353098601621,-29.221814878596,9.10356946741858));
#38663=CARTESIAN_POINT('Ctrl Pts',(-8.30606190926227,-29.2334851854665,
8.90597273134222));
#38664=CARTESIAN_POINT('Ctrl Pts',(-8.52132966920872,-29.245155492337,8.70022553865971));
#38665=CARTESIAN_POINT('Ctrl Pts',(-8.7287500754548,-29.2568257992075,8.4868941533548));
#38666=CARTESIAN_POINT('Ctrl Pts',(-8.93617048170086,-29.2684961060779,
8.27356276804991));
#38667=CARTESIAN_POINT('Ctrl Pts',(-9.13574330666112,-29.2801664129484,
8.05264743678594));
#38668=CARTESIAN_POINT('Ctrl Pts',(-9.32692999639901,-29.2918367198189,
7.82475731842672));
#38669=CARTESIAN_POINT('Ctrl Pts',(-9.50954872309849,-29.302984026066,7.6070800141164));
#38670=CARTESIAN_POINT('Ctrl Pts',(-9.68457097741769,-29.3141313323131,
7.38297431499236));
#38671=CARTESIAN_POINT('Ctrl Pts',(-9.85155459629223,-29.3252786385603,
7.1529939386437));
#38672=CARTESIAN_POINT('Ctrl Pts',(-10.0185098530204,-29.3364240514388,
6.9230526244327));
#38673=CARTESIAN_POINT('Ctrl Pts',(-10.1774290435821,-29.3475694643174,
6.68723884089972));
#38674=CARTESIAN_POINT('Ctrl Pts',(-10.3279118601732,-29.358714877196,6.44613735957391));
#38675=CARTESIAN_POINT('Ctrl Pts',(-10.4783779708334,-29.3698590527605,
6.20506264425865));
#38676=CARTESIAN_POINT('Ctrl Pts',(-10.6204094365009,-29.3810032283251,
5.95870162955929));
#38677=CARTESIAN_POINT('Ctrl Pts',(-10.753649997694,-29.3921474038897,5.70766694693163));
#38678=CARTESIAN_POINT('Ctrl Pts',(-10.8910865748418,-29.4036425321825,
5.44872667216268));
#38679=CARTESIAN_POINT('Ctrl Pts',(-11.019169440786,-29.4151376604754,5.18481385036724));
#38680=CARTESIAN_POINT('Ctrl Pts',(-11.1375588475103,-29.4266327887682,
4.91662823164873));
#38681=CARTESIAN_POINT('Ctrl Pts',(-11.2523398929623,-29.4377775599059,
4.6566165756786));
#38682=CARTESIAN_POINT('Ctrl Pts',(-11.3580095056908,-29.4489223310435,
4.39258898024842));
#38683=CARTESIAN_POINT('Ctrl Pts',(-11.4543065619484,-29.4600671021811,
4.12520441128752));
#38684=CARTESIAN_POINT('Ctrl Pts',(-11.5551445408871,-29.4717374090516,
3.84521122581278));
#38685=CARTESIAN_POINT('Ctrl Pts',(-11.6457046540313,-29.483407715922,3.56153714931589));
#38686=CARTESIAN_POINT('Ctrl Pts',(-11.7257449261543,-29.4950780227925,
3.274958958028));
#38687=CARTESIAN_POINT('Ctrl Pts',(-11.8057851982772,-29.506748329663,2.98838076674009));
#38688=CARTESIAN_POINT('Ctrl Pts',(-11.8753055475832,-29.5184186365335,
2.69889878615673));
#38689=CARTESIAN_POINT('Ctrl Pts',(-11.9341245976263,-29.530088943404,2.4073056179742));
#38690=CARTESIAN_POINT('Ctrl Pts',(-11.9917048891097,-29.5415134677853,
2.12185354749385));
#38691=CARTESIAN_POINT('Ctrl Pts',(-12.0390440781821,-29.5529379921666,
1.83431123741328));
#38692=CARTESIAN_POINT('Ctrl Pts',(-12.0760155945832,-29.5643625165479,
1.54541179281881));
#38693=CARTESIAN_POINT('Ctrl Pts',(-12.1129779697708,-29.5757842162137,
1.25658377865915));
#38694=CARTESIAN_POINT('Ctrl Pts',(-12.1395777632545,-29.5872059158794,
0.966399535564798));
#38695=CARTESIAN_POINT('Ctrl Pts',(-12.1557400447632,-29.5986276155452,
0.675599151968931));
#38696=CARTESIAN_POINT('Ctrl Pts',(-12.168238897098,-29.6074604116736,0.450713138721019));
#38697=CARTESIAN_POINT('Ctrl Pts',(-12.1744966634544,-29.616293207802,0.225458828196562));
#38698=CARTESIAN_POINT('Ctrl Pts',(-12.1744999986658,-29.6251260039304,
0.000180241411402181));
#38699=CARTESIAN_POINT('Origin',(0.,-13.3748739960349,0.));
#38700=CARTESIAN_POINT('',(7.41272179941104,-24.687686530294,-9.65763976210214));
#38701=CARTESIAN_POINT('',(7.41272179941101,-24.9374329008951,-9.65763976210217));
#38702=CARTESIAN_POINT('',(7.41272179941101,-13.3748739960349,-9.65763976210217));
#38703=CARTESIAN_POINT('',(-12.1744999986836,-26.8748739959973,-0.000179033899940194));
#38704=CARTESIAN_POINT('Ctrl Pts',(7.41272179941101,-24.9374329008951,-9.65763976210217));
#38705=CARTESIAN_POINT('Ctrl Pts',(7.63819850586434,-24.9485801303023,-9.4845751067249));
#38706=CARTESIAN_POINT('Ctrl Pts',(7.85759282138039,-24.9597273597096,-9.30362524607513));
#38707=CARTESIAN_POINT('Ctrl Pts',(8.07036187721715,-24.9708745891168,-9.1152459879457));
#38708=CARTESIAN_POINT('Ctrl Pts',(8.19274451282144,-24.9772863641241,-9.00689212035723));
#38709=CARTESIAN_POINT('Ctrl Pts',(8.3129358372104,-24.9836981391314,-8.89608102723486));
#38710=CARTESIAN_POINT('Ctrl Pts',(8.43083778298808,-24.9901099141387,-8.78290524410578));
#38711=CARTESIAN_POINT('Ctrl Pts',(8.63581832193552,-25.0012572203849,-8.58614145985624));
#38712=CARTESIAN_POINT('Ctrl Pts',(8.83393818577717,-25.0124045266311,-8.38216922295967));
#38713=CARTESIAN_POINT('Ctrl Pts',(9.02469819859376,-25.0235518328773,-8.17149145959895));
#38714=CARTESIAN_POINT('Ctrl Pts',(9.21542581084571,-25.0346972457549,-7.96084947983034));
#38715=CARTESIAN_POINT('Ctrl Pts',(9.39879588886446,-25.0458426586325,-7.74350444513577));
#38716=CARTESIAN_POINT('Ctrl Pts',(9.57434752759173,-25.0569880715101,-7.5199946589674));
#38717=CARTESIAN_POINT('Ctrl Pts',(9.74987967736235,-25.0681322470739,-7.2965096858544));
#38718=CARTESIAN_POINT('Ctrl Pts',(9.91759495631258,-25.0792764226377,-7.06686153759513));
#38719=CARTESIAN_POINT('Ctrl Pts',(10.0770732542511,-25.0904205982015,-6.83162095541444));
#38720=CARTESIAN_POINT('Ctrl Pts',(10.2415738477981,-25.101915726495,-6.58897216937083));
#38721=CARTESIAN_POINT('Ctrl Pts',(10.3973100804441,-25.1134108547885,-6.34037324759497));
#38722=CARTESIAN_POINT('Ctrl Pts',(10.5438688836484,-25.1249059830821,-6.0864833208045));
#38723=CARTESIAN_POINT('Ctrl Pts',(10.6859607575327,-25.1360507542187,-5.8403316419611));
#38724=CARTESIAN_POINT('Ctrl Pts',(10.8194262115694,-25.1471955253553,-5.58920695028854));
#38725=CARTESIAN_POINT('Ctrl Pts',(10.9439347333876,-25.1583402964919,-5.3337362890709));
#38726=CARTESIAN_POINT('Ctrl Pts',(11.0743144998255,-25.1700106033639,-5.06621881593028));
#38727=CARTESIAN_POINT('Ctrl Pts',(11.1948721341598,-25.1816809102359,-4.79393592517866));
#38728=CARTESIAN_POINT('Ctrl Pts',(11.3052834849987,-25.1933512171079,-4.51763384680706));
#38729=CARTESIAN_POINT('Ctrl Pts',(11.4156948358375,-25.2050215239798,-4.24133176843546));
#38730=CARTESIAN_POINT('Ctrl Pts',(11.5159597868368,-25.2166918308518,-3.9610108172485));
#38731=CARTESIAN_POINT('Ctrl Pts',(11.6058127307487,-25.2283621377238,-3.67743947724378));
#38732=CARTESIAN_POINT('Ctrl Pts',(11.6916389471497,-25.2395094439717,-3.4065762853131));
#38733=CARTESIAN_POINT('Ctrl Pts',(11.7679914973803,-25.2506567502196,-3.13266673460072));
#38734=CARTESIAN_POINT('Ctrl Pts',(11.834672744551,-25.2618040564674,-2.85639130361768));
#38735=CARTESIAN_POINT('Ctrl Pts',(11.9013426659205,-25.2729494693468,-2.58016279798063));
#38736=CARTESIAN_POINT('Ctrl Pts',(11.9583445012586,-25.2840948822262,-2.30156947355845));
#38737=CARTESIAN_POINT('Ctrl Pts',(12.0055311474859,-25.2952402951056,-2.02130455813741));
#38738=CARTESIAN_POINT('Ctrl Pts',(12.0527125552623,-25.3063844706709,-1.7410707564762));
#38739=CARTESIAN_POINT('Ctrl Pts',(12.0900809054865,-25.3175286462363,-1.45916599735268));
#38740=CARTESIAN_POINT('Ctrl Pts',(12.1175404384541,-25.3286728218017,-1.17629246891674));
#38741=CARTESIAN_POINT('Ctrl Pts',(12.1458647278962,-25.340167950094,-0.884510678439701));
#38742=CARTESIAN_POINT('Ctrl Pts',(12.163645951052,-25.3516630783862,-0.591698407265157));
#38743=CARTESIAN_POINT('Ctrl Pts',(12.1708368293856,-25.3631582066785,-0.29863208546831));
#38744=CARTESIAN_POINT('Ctrl Pts',(12.1778085387284,-25.3743029778168,-0.0144980591447471));
#38745=CARTESIAN_POINT('Ctrl Pts',(12.1748258979266,-25.3854477489552,0.269874481842067));
#38746=CARTESIAN_POINT('Ctrl Pts',(12.1618987628609,-25.3965925200936,0.553776788898335));
#38747=CARTESIAN_POINT('Ctrl Pts',(12.148362044046,-25.4082628269628,0.851066612358317));
#38748=CARTESIAN_POINT('Ctrl Pts',(12.1239204060494,-25.419933133832,1.14784046916088));
#38749=CARTESIAN_POINT('Ctrl Pts',(12.088646326029,-25.4316034407012,1.44328800112304));
#38750=CARTESIAN_POINT('Ctrl Pts',(12.0533722460086,-25.4432737475704,1.73873553308519));
#38751=CARTESIAN_POINT('Ctrl Pts',(12.0072657724544,-25.4549440544397,2.03285640811261));
#38752=CARTESIAN_POINT('Ctrl Pts',(11.9504614375384,-25.4666143613089,2.32484874344699));
#38753=CARTESIAN_POINT('Ctrl Pts',(11.8962027685468,-25.4777616675556,2.60375554685274));
#38754=CARTESIAN_POINT('Ctrl Pts',(11.832167798918,-25.4889089738023,2.88080369527671));
#38755=CARTESIAN_POINT('Ctrl Pts',(11.7585086287844,-25.5000562800489,3.15530110715318));
#38756=CARTESIAN_POINT('Ctrl Pts',(11.6848619696517,-25.5112016929271,3.4297518956788));
#38757=CARTESIAN_POINT('Ctrl Pts',(11.6015944427383,-25.5223471058052,3.70165255508999));
#38758=CARTESIAN_POINT('Ctrl Pts',(11.5089086211831,-25.5334925186833,3.97032399172388));
#38759=CARTESIAN_POINT('Ctrl Pts',(11.4162330891935,-25.5446366942475,4.23896560165561));
#38760=CARTESIAN_POINT('Ctrl Pts',(11.3141414373819,-25.5557808698117,4.5043784525661));
#38761=CARTESIAN_POINT('Ctrl Pts',(11.2028856095872,-25.5669250453759,4.76590015301466));
#38762=CARTESIAN_POINT('Ctrl Pts',(11.0881261097483,-25.5784201736691,5.03565770311674));
#38763=CARTESIAN_POINT('Ctrl Pts',(10.9636159909716,-25.5899153019623,5.30127477407346));
#38764=CARTESIAN_POINT('Ctrl Pts',(10.8296852946106,-25.6014104302554,5.56204698557055));
#38765=CARTESIAN_POINT('Ctrl Pts',(10.6998366386309,-25.6125552013926,5.81487118569636));
#38766=CARTESIAN_POINT('Ctrl Pts',(10.5611332838991,-25.6236999725298,6.06314123540553));
#38767=CARTESIAN_POINT('Ctrl Pts',(10.4139230509799,-25.6348447436669,6.30623952433371));
#38768=CARTESIAN_POINT('Ctrl Pts',(10.2597710660175,-25.6465150505381,6.56080120144097));
#38769=CARTESIAN_POINT('Ctrl Pts',(10.0962907731105,-25.6581853574093,6.80969135715406));
#38770=CARTESIAN_POINT('Ctrl Pts',(9.92393360285792,-25.6698556642805,7.05223312831244));
#38771=CARTESIAN_POINT('Ctrl Pts',(9.75157643260539,-25.6815259711516,7.29477489947081));
#38772=CARTESIAN_POINT('Ctrl Pts',(9.57034258650591,-25.6931962780228,7.53096801767879));
#38773=CARTESIAN_POINT('Ctrl Pts',(9.38073392759741,-25.704866584894,7.76017275771763));
#38774=CARTESIAN_POINT('Ctrl Pts',(9.19962251284825,-25.7160138911413,7.97910576939872));
#38775=CARTESIAN_POINT('Ctrl Pts',(9.01081632348776,-25.7271611973886,8.19172838519732));
#38776=CARTESIAN_POINT('Ctrl Pts',(8.81478010379253,-25.738308503636,8.39750569941952));
#38777=CARTESIAN_POINT('Ctrl Pts',(8.61877718082411,-25.7494539165147,8.60324806239126));
#38778=CARTESIAN_POINT('Ctrl Pts',(8.41554686318432,-25.7605993293935,8.80214725200268));
#38779=CARTESIAN_POINT('Ctrl Pts',(8.20559199842757,-25.7717447422723,8.9937039202623));
#38780=CARTESIAN_POINT('Ctrl Pts',(7.99566044192338,-25.7828889178371,9.18523932275507));
#38781=CARTESIAN_POINT('Ctrl Pts',(7.77900602600685,-25.7940330934018,9.36943365184795));
#38782=CARTESIAN_POINT('Ctrl Pts',(7.55616695615428,-25.8051772689666,9.54582585116249));
#38783=CARTESIAN_POINT('Ctrl Pts',(7.3263102312941,-25.8166723972593,9.72777299917451));
#38784=CARTESIAN_POINT('Ctrl Pts',(7.08987323230984,-25.828167525552,9.90141845280191));
#38785=CARTESIAN_POINT('Ctrl Pts',(6.84748283278449,-25.8396626538447,10.0663016597319));
#38786=CARTESIAN_POINT('Ctrl Pts',(6.61248018993246,-25.8508074249825,10.2261594324257));
#38787=CARTESIAN_POINT('Ctrl Pts',(6.37188190783707,-25.8619521961203,10.3777810168332));
#38788=CARTESIAN_POINT('Ctrl Pts',(6.1262889482455,-25.8730969672581,10.5207905583471));
#38789=CARTESIAN_POINT('Ctrl Pts',(5.8691149634102,-25.8847672741282,10.6705437667524));
#38790=CARTESIAN_POINT('Ctrl Pts',(5.60646418974573,-25.8964375809984,10.8108530211069));
#38791=CARTESIAN_POINT('Ctrl Pts',(5.33905692026268,-25.9081078878686,10.9413400208656));
#38792=CARTESIAN_POINT('Ctrl Pts',(5.07164965077963,-25.9197781947387,11.0718270206242));
#38793=CARTESIAN_POINT('Ctrl Pts',(4.79948619084543,-25.9314485016089,11.192491626544));
#38794=CARTESIAN_POINT('Ctrl Pts',(4.52331334430271,-25.943118808479,11.3030122816554));
#38795=CARTESIAN_POINT('Ctrl Pts',(4.25951708497672,-25.9542661147261,11.4085799931869));
#38796=CARTESIAN_POINT('Ctrl Pts',(3.99198411281679,-25.9654134209732,11.5049244932549));
#38797=CARTESIAN_POINT('Ctrl Pts',(3.72137847838849,-25.9765607272202,11.5917985002581));
#38798=CARTESIAN_POINT('Ctrl Pts',(3.45081880629348,-25.9877061400987,11.6786577517222));
#38799=CARTESIAN_POINT('Ctrl Pts',(3.1771877677697,-25.9988515529772,11.7560496401096));
#38800=CARTESIAN_POINT('Ctrl Pts',(2.90116585463097,-26.0099969658557,11.8237763398131));
#38801=CARTESIAN_POINT('Ctrl Pts',(2.62517458421184,-26.0211411414202,11.891495520801));
#38802=CARTESIAN_POINT('Ctrl Pts',(2.34679322818403,-26.0322853169848,11.9495515921384));
#38803=CARTESIAN_POINT('Ctrl Pts',(2.06671500071761,-26.0434294925493,11.9977972709914));
#38804=CARTESIAN_POINT('Ctrl Pts',(1.7778165408784,-26.0549246208422,12.0475623042844));
#38805=CARTESIAN_POINT('Ctrl Pts',(1.48711289264152,-26.0664197491351,12.0868889741013));
#38806=CARTESIAN_POINT('Ctrl Pts',(1.19537488525744,-26.0779148774281,12.1156728716855));
#38807=CARTESIAN_POINT('Ctrl Pts',(0.912528688019575,-26.0890596485656,
12.1435794720163));
#38808=CARTESIAN_POINT('Ctrl Pts',(0.628710527637285,-26.1002044197031,
12.1615764172742));
#38809=CARTESIAN_POINT('Ctrl Pts',(0.344627949634741,-26.1113491908406,
12.1696212688124));
#38810=CARTESIAN_POINT('Ctrl Pts',(0.0471493544286068,-26.1230194977112,
12.1780454782484));
#38811=CARTESIAN_POINT('Ctrl Pts',(-0.250618878125068,-26.1346898045818,
12.1755564116312));
#38812=CARTESIAN_POINT('Ctrl Pts',(-0.547863251496386,-26.1463601114524,
12.1621665877285));
#38813=CARTESIAN_POINT('Ctrl Pts',(-0.845107624867718,-26.158030418323,
12.1487767638259));
#38814=CARTESIAN_POINT('Ctrl Pts',(-1.1418278042907,-26.1697007251936,12.124486206505));
#38815=CARTESIAN_POINT('Ctrl Pts',(-1.43721416924489,-26.1813710320642,
12.089369945606));
#38816=CARTESIAN_POINT('Ctrl Pts',(-1.71936290002593,-26.1925183383113,
12.0558274073648));
#38817=CARTESIAN_POINT('Ctrl Pts',(-2.00037900433124,-26.2036656445584,
12.0123981199221));
#38818=CARTESIAN_POINT('Ctrl Pts',(-2.27956106827263,-26.2148129508055,
11.9591827306892));
#38819=CARTESIAN_POINT('Ctrl Pts',(-2.55869571317629,-26.2259583636841,
11.9059763800834));
#38820=CARTESIAN_POINT('Ctrl Pts',(-2.83599667771849,-26.2371037765627,
11.8429872961325));
#38821=CARTESIAN_POINT('Ctrl Pts',(-3.11077177834321,-26.2482491894412,
11.770367419629));
#38822=CARTESIAN_POINT('Ctrl Pts',(-3.38551637466598,-26.2593933650059,
11.6977556050591));
#38823=CARTESIAN_POINT('Ctrl Pts',(-3.65773540917929,-26.2705375405707,
11.6155152010347));
#38824=CARTESIAN_POINT('Ctrl Pts',(-3.92674971415585,-26.2816817161354,
11.5238486163424));
#38825=CARTESIAN_POINT('Ctrl Pts',(-4.20423582610319,-26.2931768444282,
11.429295264676));
#38826=CARTESIAN_POINT('Ctrl Pts',(-4.47831180683099,-26.304671972721,11.3247124991547));
#38827=CARTESIAN_POINT('Ctrl Pts',(-4.74825085465912,-26.3161671010139,
11.2103775168916));
#38828=CARTESIAN_POINT('Ctrl Pts',(-5.00996249740978,-26.3273118721515,
11.0995273221062));
#38829=CARTESIAN_POINT('Ctrl Pts',(-5.26778539315621,-26.3384566432891,
10.9795106872944));
#38830=CARTESIAN_POINT('Ctrl Pts',(-5.52107796274188,-26.3496014144267,
10.8506289393438));
#38831=CARTESIAN_POINT('Ctrl Pts',(-5.78631463548927,-26.3612717212971,
10.7156697257349));
#38832=CARTESIAN_POINT('Ctrl Pts',(-6.04658315982579,-26.3729420281675,
10.5709893503964));
#38833=CARTESIAN_POINT('Ctrl Pts',(-6.30117522427095,-26.384612335038,10.4169880984397));
#38834=CARTESIAN_POINT('Ctrl Pts',(-6.55576728871611,-26.3962826419084,
10.262986846483));
#38835=CARTESIAN_POINT('Ctrl Pts',(-6.8046826107453,-26.4079529487789,10.0996648990647));
#38836=CARTESIAN_POINT('Ctrl Pts',(-7.04724619648092,-26.4196232556493,
9.92747557519963));
#38837=CARTESIAN_POINT('Ctrl Pts',(-7.27893938198356,-26.4307705618965,
9.76300285422281));
#38838=CARTESIAN_POINT('Ctrl Pts',(-7.50490681694821,-26.4419178681436,
9.59039094205251));
#38839=CARTESIAN_POINT('Ctrl Pts',(-7.72458077897762,-26.4530651743908,
9.41006387008343));
#38840=CARTESIAN_POINT('Ctrl Pts',(-7.9442174294129,-26.4642105872694,9.22976742664427));
#38841=CARTESIAN_POINT('Ctrl Pts',(-8.15756253496308,-26.4753560001481,
9.04175860884122));
#38842=CARTESIAN_POINT('Ctrl Pts',(-8.36408102412932,-26.4865014130267,
8.84650206984658));
#38843=CARTESIAN_POINT('Ctrl Pts',(-8.57057658653295,-26.4976455885913,
8.65126720736302));
#38844=CARTESIAN_POINT('Ctrl Pts',(-8.77024685209962,-26.5087897641558,
8.44878641357831));
#38845=CARTESIAN_POINT('Ctrl Pts',(-8.96259232915518,-26.5199339397204,
8.23956242717833));
#38846=CARTESIAN_POINT('Ctrl Pts',(-9.16099515603928,-26.5314290680132,
8.0237495524013));
#38847=CARTESIAN_POINT('Ctrl Pts',(-9.35160416569127,-26.542924196306,7.80076210097047));
#38848=CARTESIAN_POINT('Ctrl Pts',(-9.53391383017232,-26.5544193245989,
7.5711912754103));
#38849=CARTESIAN_POINT('Ctrl Pts',(-9.71066692374877,-26.5655640957365,
7.34861748192455));
#38850=CARTESIAN_POINT('Ctrl Pts',(-9.87961891449672,-26.5767088668741,
7.11985589637044));
#38851=CARTESIAN_POINT('Ctrl Pts',(-10.0403506524587,-26.5878536380117,
6.88547812614872));
#38852=CARTESIAN_POINT('Ctrl Pts',(-10.2086617539316,-26.5995239448822,
6.64004818700301));
#38853=CARTESIAN_POINT('Ctrl Pts',(-10.3679585107329,-26.6111942517526,
6.38845991414234));
#38854=CARTESIAN_POINT('Ctrl Pts',(-10.5178105333709,-26.622864558623,6.13140374091549));
#38855=CARTESIAN_POINT('Ctrl Pts',(-10.6676625560089,-26.6345348654935,
5.87434756768864));
#38856=CARTESIAN_POINT('Ctrl Pts',(-10.8080696830999,-26.6462051723639,
5.61182378836291));
#38857=CARTESIAN_POINT('Ctrl Pts',(-10.9386561591369,-26.6578754792344,
5.34455345956773));
#38858=CARTESIAN_POINT('Ctrl Pts',(-11.0629966322907,-26.6689875907038,
5.09006677648294));
#38859=CARTESIAN_POINT('Ctrl Pts',(-11.1784731441786,-26.6800997021732,
4.83119636045063));
#38860=CARTESIAN_POINT('Ctrl Pts',(-11.284791078264,-26.6912118136426,4.56858189922576));
#38861=CARTESIAN_POINT('Ctrl Pts',(-11.3910898863404,-26.7023219261046,
4.30601468089191));
#38862=CARTESIAN_POINT('Ctrl Pts',(-11.4882333044429,-26.7134320385665,
4.03970501227435));
#38863=CARTESIAN_POINT('Ctrl Pts',(-11.5759747961597,-26.7245421510285,
3.77031268844835));
#38864=CARTESIAN_POINT('Ctrl Pts',(-11.6637063953042,-26.7356510108608,
3.50095073774466));
#38865=CARTESIAN_POINT('Ctrl Pts',(-11.742038101081,-26.7467598706931,3.22850708261955));
#38866=CARTESIAN_POINT('Ctrl Pts',(-11.8107728310722,-26.7578687305254,
2.95365796645564));
#38867=CARTESIAN_POINT('Ctrl Pts',(-11.8795114701164,-26.7689782221362,
2.67879321918694));
#38868=CARTESIAN_POINT('Ctrl Pts',(-11.938651974578,-26.780087713747,2.40152299895952));
#38869=CARTESIAN_POINT('Ctrl Pts',(-11.9880477658973,-26.7911972053578,
2.12253645729935));
#38870=CARTESIAN_POINT('Ctrl Pts',(-12.0374432737353,-26.8023066332115,
1.84355151673624));
#38871=CARTESIAN_POINT('Ctrl Pts',(-12.0770941352764,-26.8134160610651,
1.56285054084612));
#38872=CARTESIAN_POINT('Ctrl Pts',(-12.1069051509043,-26.8245254889188,
1.28113149871751));
#38873=CARTESIAN_POINT('Ctrl Pts',(-12.136721994767,-26.8356370887331,0.9993573788041));
#38874=CARTESIAN_POINT('Ctrl Pts',(-12.1566951200387,-26.8467486885475,
0.716565063644844));
#38875=CARTESIAN_POINT('Ctrl Pts',(-12.1667811943891,-26.8578602883618,
0.433457746337774));
#38876=CARTESIAN_POINT('Ctrl Pts',(-12.1719290135767,-26.8635315242403,
0.288962947910597));
#38877=CARTESIAN_POINT('Ctrl Pts',(-12.1745021246081,-26.8692027601188,
0.144386144645321));
#38878=CARTESIAN_POINT('Ctrl Pts',(-12.1744999986836,-26.8748739959973,
-0.000179033899942618));
#38879=CARTESIAN_POINT('Ctrl Pts',(-12.1744999986836,-26.8748739960349,
-0.000179034858391824));
#38880=CARTESIAN_POINT('Ctrl Pts',(-12.1744973429416,-26.8819585649631,
-0.180771412597766));
#38881=CARTESIAN_POINT('Ctrl Pts',(-12.170475924864,-26.8890431338913,-0.361351713761423));
#38882=CARTESIAN_POINT('Ctrl Pts',(-12.1624403133837,-26.8961277028195,
-0.541752594251753));
#38883=CARTESIAN_POINT('Ctrl Pts',(-12.1497965769811,-26.9072750090666,
-0.825606683675804));
#38884=CARTESIAN_POINT('Ctrl Pts',(-12.127209485585,-26.9184223153137,-1.109060343361));
#38885=CARTESIAN_POINT('Ctrl Pts',(-12.094727685764,-26.9295696215608,-1.39140664696373));
#38886=CARTESIAN_POINT('Ctrl Pts',(-12.0622514029725,-26.9407150344394,
-1.67370499408291));
#38887=CARTESIAN_POINT('Ctrl Pts',(-12.0198837975782,-26.9518604473179,
-1.95489609573094));
#38888=CARTESIAN_POINT('Ctrl Pts',(-11.9677253505645,-26.9630058601965,
-2.23427844805787));
#38889=CARTESIAN_POINT('Ctrl Pts',(-11.9155726939485,-26.9741500357611,
-2.51362978460458));
#38890=CARTESIAN_POINT('Ctrl Pts',(-11.8536314150918,-26.9852942113258,
-2.79117251064493));
#38891=CARTESIAN_POINT('Ctrl Pts',(-11.7820532854202,-26.9964383868904,
-3.0662143808806));
#38892=CARTESIAN_POINT('Ctrl Pts',(-11.7082210150325,-27.0079335151833,
-3.3499178783647));
#38893=CARTESIAN_POINT('Ctrl Pts',(-11.6241351555881,-27.0194286434761,
-3.63096016396926));
#38894=CARTESIAN_POINT('Ctrl Pts',(-11.530018550358,-27.030923771769,-3.90859597277591));
#38895=CARTESIAN_POINT('Ctrl Pts',(-11.4387705017224,-27.0420685429066,
-4.17776978884194));
#38896=CARTESIAN_POINT('Ctrl Pts',(-11.3380941917879,-27.0532133140442,
-4.44374143924996));
#38897=CARTESIAN_POINT('Ctrl Pts',(-11.2282428127532,-27.0643580851818,
-4.70584887006112));
#38898=CARTESIAN_POINT('Ctrl Pts',(-11.1132113520216,-27.0760283920523,
-4.98031607201867));
#38899=CARTESIAN_POINT('Ctrl Pts',(-10.9881188167639,-27.0876986989227,
-5.25054555485061));
#38900=CARTESIAN_POINT('Ctrl Pts',(-10.8533121666699,-27.0993690057932,
-5.51580141618739));
#38901=CARTESIAN_POINT('Ctrl Pts',(-10.7185055165759,-27.1110393126637,
-5.78105727752418));
#38902=CARTESIAN_POINT('Ctrl Pts',(-10.5739849114736,-27.1227096195341,
-6.04133922225082));
#38903=CARTESIAN_POINT('Ctrl Pts',(-10.4201526576011,-27.1343799264046,
-6.29594066381572));
#38904=CARTESIAN_POINT('Ctrl Pts',(-10.2732143410997,-27.1455272326517,
-6.53913223294777));
#38905=CARTESIAN_POINT('Ctrl Pts',(-10.1177367424751,-27.1566745388988,
-6.77721387905434));
#38906=CARTESIAN_POINT('Ctrl Pts',(-9.95410087098509,-27.167821845146,-7.00958815482435));
#38907=CARTESIAN_POINT('Ctrl Pts',(-9.79049279302736,-27.1789672580245,
-7.24192296185269));
#38908=CARTESIAN_POINT('Ctrl Pts',(-9.61872936224129,-27.190112670903,-7.46855211592874));
#38909=CARTESIAN_POINT('Ctrl Pts',(-9.43923450693786,-27.2012580837816,
-7.68890773602035));
#38910=CARTESIAN_POINT('Ctrl Pts',(-9.2597595783524,-27.2124022593461,-7.9092388932142));
#38911=CARTESIAN_POINT('Ctrl Pts',(-9.07255510757798,-27.2235464349107,
-8.12329770037941));
#38912=CARTESIAN_POINT('Ctrl Pts',(-8.87808562861877,-27.2346906104752,
-8.33054895075426));
#38913=CARTESIAN_POINT('Ctrl Pts',(-8.67749191069513,-27.2461857387681,
-8.54432696404207));
#38914=CARTESIAN_POINT('Ctrl Pts',(-8.46916838599521,-27.257680867061,-8.75086148201259));
#38915=CARTESIAN_POINT('Ctrl Pts',(-8.25366736632376,-27.2691759953538,
-8.94960475418229));
#38916=CARTESIAN_POINT('Ctrl Pts',(-8.04473454861487,-27.2803207664914,
-9.14229057960626));
#38917=CARTESIAN_POINT('Ctrl Pts',(-7.82905548443714,-27.291465537629,-9.32765287209847));
#38918=CARTESIAN_POINT('Ctrl Pts',(-7.60716931389788,-27.3026103087666,
-9.50523146902223));
#38919=CARTESIAN_POINT('Ctrl Pts',(-7.37482002035491,-27.3142806156371,
-9.69118384921479));
#38920=CARTESIAN_POINT('Ctrl Pts',(-7.13566438620726,-27.3259509225076,
-9.86860058581242));
#38921=CARTESIAN_POINT('Ctrl Pts',(-6.89035922507428,-27.3376212293782,
-10.0370015442578));
#38922=CARTESIAN_POINT('Ctrl Pts',(-6.64505406394129,-27.3492915362487,
-10.2054025027032));
#38923=CARTESIAN_POINT('Ctrl Pts',(-6.39359965738751,-27.3609618431192,
-10.3647875003511));
#38924=CARTESIAN_POINT('Ctrl Pts',(-6.13668738798872,-27.3726321499897,
-10.5147286295035));
#38925=CARTESIAN_POINT('Ctrl Pts',(-5.89128854994562,-27.3837794562368,
-10.6579502006452));
#38926=CARTESIAN_POINT('Ctrl Pts',(-5.64083698966155,-27.3949267624839,
-10.7925985197516));
#38927=CARTESIAN_POINT('Ctrl Pts',(-5.38595316180751,-27.4060740687311,
-10.9183313188791));
#38928=CARTESIAN_POINT('Ctrl Pts',(-5.13111262593913,-27.4172194816096,
-11.0440427623067));
#38929=CARTESIAN_POINT('Ctrl Pts',(-4.87184156463934,-27.4283648944882,
-11.1608415910916));
#38930=CARTESIAN_POINT('Ctrl Pts',(-4.60878396953977,-27.4395103073668,
-11.2684320369834));
#38931=CARTESIAN_POINT('Ctrl Pts',(-4.3457555779199,-27.4506544829314,-11.3760105386643));
#38932=CARTESIAN_POINT('Ctrl Pts',(-4.07894173873217,-27.461798658496,-11.4743825978158));
#38933=CARTESIAN_POINT('Ctrl Pts',(-3.80900646198326,-27.4729428340606,
-11.5633005678556));
#38934=CARTESIAN_POINT('Ctrl Pts',(-3.53057037498807,-27.4844379623534,
-11.6550187454114));
#38935=CARTESIAN_POINT('Ctrl Pts',(-3.24881334259174,-27.4959330906463,
-11.7366776258322));
#38936=CARTESIAN_POINT('Ctrl Pts',(-2.96448245205888,-27.5074282189391,
-11.8080605537673));
#38937=CARTESIAN_POINT('Ctrl Pts',(-2.68881761199677,-27.5185729900768,
-11.877267819202));
#38938=CARTESIAN_POINT('Ctrl Pts',(-2.41073375712401,-27.5297177612144,
-11.9368161849391));
#38939=CARTESIAN_POINT('Ctrl Pts',(-2.13092449458315,-27.540862532352,-11.9865596001682));
#38940=CARTESIAN_POINT('Ctrl Pts',(-1.83792072458815,-27.5525328392224,
-12.0386486842186));
#38941=CARTESIAN_POINT('Ctrl Pts',(-1.5430252199813,-27.5642031460929,-12.0799857998834));
#38942=CARTESIAN_POINT('Ctrl Pts',(-1.24704447022982,-27.5758734529634,
-12.1104636715226));
#38943=CARTESIAN_POINT('Ctrl Pts',(-0.951063720478334,-27.5875437598338,
-12.1409415431618));
#38944=CARTESIAN_POINT('Ctrl Pts',(-0.653998060217559,-27.5992140667043,
-12.1605601451418));
#38945=CARTESIAN_POINT('Ctrl Pts',(-0.356659339898103,-27.6108843735748,
-12.1692746030839));
#38946=CARTESIAN_POINT('Ctrl Pts',(-0.0726457478549768,-27.6220316798219,
-12.177598525714));
#38947=CARTESIAN_POINT('Ctrl Pts',(0.211701791907702,-27.633178986069,-12.175976638602));
#38948=CARTESIAN_POINT('Ctrl Pts',(0.495674690478524,-27.6443262923161,
-12.1644053225474));
#38949=CARTESIAN_POINT('Ctrl Pts',(0.779599356289084,-27.6554717051947,
-12.1528359718793));
#38950=CARTESIAN_POINT('Ctrl Pts',(1.06314924152558,-27.6666171180733,-12.1313205770283));
#38951=CARTESIAN_POINT('Ctrl Pts',(1.34561734240108,-27.6777625309519,-12.0999076119543));
#38952=CARTESIAN_POINT('Ctrl Pts',(1.6280540849292,-27.6889067065165,-12.0684981342074));
#38953=CARTESIAN_POINT('Ctrl Pts',(1.90940901786181,-27.7000508820811,-12.02719330981));
#38954=CARTESIAN_POINT('Ctrl Pts',(2.18898058826488,-27.7111950576458,-11.9760934462871));
#38955=CARTESIAN_POINT('Ctrl Pts',(2.4773564353774,-27.7226901859386,-11.923384344251));
#38956=CARTESIAN_POINT('Ctrl Pts',(2.76383448278513,-27.7341853142314,-11.8602533185206));
#38957=CARTESIAN_POINT('Ctrl Pts',(3.04765506100921,-27.7456804425243,-11.7868676449303));
#38958=CARTESIAN_POINT('Ctrl Pts',(3.32282514244449,-27.7568252136619,-11.7157186750269));
#38959=CARTESIAN_POINT('Ctrl Pts',(3.59549707841157,-27.7679699847995,-11.6349309684199));
#38960=CARTESIAN_POINT('Ctrl Pts',(3.86499194570396,-27.7791147559371,-11.5447082037461));
#38961=CARTESIAN_POINT('Ctrl Pts',(4.14719494139433,-27.7907850628076,-11.4502309518185));
#38962=CARTESIAN_POINT('Ctrl Pts',(4.42591372566347,-27.8024553696781,-11.3454075047072));
#38963=CARTESIAN_POINT('Ctrl Pts',(4.70038881294249,-27.8141256765485,-11.2305296071541));
#38964=CARTESIAN_POINT('Ctrl Pts',(4.97486390022151,-27.825795983419,-11.115651709601));
#38965=CARTESIAN_POINT('Ctrl Pts',(5.24509498441225,-27.8374662902895,-10.9907194992353));
#38966=CARTESIAN_POINT('Ctrl Pts',(5.5103477343262,-27.8491365971599,-10.8560820785773));
#38967=CARTESIAN_POINT('Ctrl Pts',(5.76371078034282,-27.8602837935513,-10.7274796530913));
#38968=CARTESIAN_POINT('Ctrl Pts',(6.01260764731629,-27.8714309899427,-10.5899845344328));
#38969=CARTESIAN_POINT('Ctrl Pts',(6.25641443501615,-27.8825781863341,-10.4439326246066));
#38970=CARTESIAN_POINT('Ctrl Pts',(6.50018381863798,-27.8937236725574,-10.2979031216095));
#38971=CARTESIAN_POINT('Ctrl Pts',(6.73886445297898,-27.9048691587806,-10.1433195848208));
#38972=CARTESIAN_POINT('Ctrl Pts',(6.97185872814829,-27.9160146450039,-9.98056291622584));
#38973=CARTESIAN_POINT('Ctrl Pts',(7.12119904837047,-27.923158470664,-9.87624218564734));
#38974=CARTESIAN_POINT('Ctrl Pts',(7.26820376898424,-27.9303022963241,-9.76856458234202));
#38975=CARTESIAN_POINT('Ctrl Pts',(7.41272179941101,-27.9374461219842,-9.65763976210217));
#38976=CARTESIAN_POINT('',(-12.174499996235,-26.6251260039329,-0.000302777009382115));
#38977=CARTESIAN_POINT('Ctrl Pts',(-12.174499996235,-26.6251260039651,-0.000302777830488094));
#38978=CARTESIAN_POINT('Ctrl Pts',(-12.1744924727439,-26.6369913152146,
-0.302817471666667));
#38979=CARTESIAN_POINT('Ctrl Pts',(-12.1632051823574,-26.648856626464,-0.605278801658912));
#38980=CARTESIAN_POINT('Ctrl Pts',(-12.1406760102577,-26.6607219377135,
-0.906882717860236));
#38981=CARTESIAN_POINT('Ctrl Pts',(-12.1341314731588,-26.6641687119366,
-0.994496146796198));
#38982=CARTESIAN_POINT('Ctrl Pts',(-12.1266386202186,-26.6676154861597,
-1.08203724349874));
#38983=CARTESIAN_POINT('Ctrl Pts',(-12.1181992022146,-26.6710622603828,
-1.16948635966588));
#38984=CARTESIAN_POINT('Ctrl Pts',(-12.0909050509449,-26.6822095666301,
-1.45230792437143));
#38985=CARTESIAN_POINT('Ctrl Pts',(-12.0537015189063,-26.6933568728774,
-1.73421580133404));
#38986=CARTESIAN_POINT('Ctrl Pts',(-12.0066737159719,-26.7045041791248,
-2.01450652225056));
#38987=CARTESIAN_POINT('Ctrl Pts',(-11.9596539007038,-26.7156495920035,
-2.29474963582362));
#38988=CARTESIAN_POINT('Ctrl Pts',(-11.9028131901233,-26.7267950048823,
-2.57337587876628));
#38989=CARTESIAN_POINT('Ctrl Pts',(-11.8362881790818,-26.737940417761,-2.84968987641259));
#38990=CARTESIAN_POINT('Ctrl Pts',(-11.7697705533498,-26.7490845933258,
-3.12597319891336));
#38991=CARTESIAN_POINT('Ctrl Pts',(-11.6935708363978,-26.7602287688906,
-3.39994452942677));
#38992=CARTESIAN_POINT('Ctrl Pts',(-11.6078763665936,-26.7713729444554,
-3.67092038974925));
#38993=CARTESIAN_POINT('Ctrl Pts',(-11.5194832038473,-26.7828680727481,
-3.95042983039985));
#38994=CARTESIAN_POINT('Ctrl Pts',(-11.4209876598191,-26.7943632010408,
-4.22675179091095));
#38995=CARTESIAN_POINT('Ctrl Pts',(-11.3126507894069,-26.8058583293335,
-4.49915351671094));
#38996=CARTESIAN_POINT('Ctrl Pts',(-11.2076158915104,-26.8170031004714,
-4.763252778092));
#38997=CARTESIAN_POINT('Ctrl Pts',(-11.0933307897004,-26.8281478716092,
-5.02366697453654));
#38998=CARTESIAN_POINT('Ctrl Pts',(-10.9700825475829,-26.839292642747,-5.27974801948126));
#38999=CARTESIAN_POINT('Ctrl Pts',(-10.8410224898273,-26.8509629496171,
-5.54790465914499));
#39000=CARTESIAN_POINT('Ctrl Pts',(-10.7021337694083,-26.8626332564873,
-5.81130936507168));
#39001=CARTESIAN_POINT('Ctrl Pts',(-10.553800908055,-26.8743035633574,-6.06924514607354));
#39002=CARTESIAN_POINT('Ctrl Pts',(-10.4054680467018,-26.8859738702276,
-6.32718092707538));
#39003=CARTESIAN_POINT('Ctrl Pts',(-10.2476912192782,-26.8976441770977,
-6.57964749669029));
#39004=CARTESIAN_POINT('Ctrl Pts',(-10.0809087053182,-26.9093144839679,
-6.82596000025198));
#39005=CARTESIAN_POINT('Ctrl Pts',(-9.92160048999432,-26.9204617902149,
-7.06123409717429));
#39006=CARTESIAN_POINT('Ctrl Pts',(-9.75402843997352,-26.931609096462,-7.29096385566852));
#39007=CARTESIAN_POINT('Ctrl Pts',(-9.57860392681835,-26.9427564027091,
-7.51457231405355));
#39008=CARTESIAN_POINT('Ctrl Pts',(-9.40320920949447,-26.9539018155876,
-7.73814279257031));
#39009=CARTESIAN_POINT('Ctrl Pts',(-9.2199648564318,-26.9650472284661,-7.95559383695199));
#39010=CARTESIAN_POINT('Ctrl Pts',(-9.02932357316257,-26.9761926413446,
-8.16638023001199));
#39011=CARTESIAN_POINT('Ctrl Pts',(-8.83870345403747,-26.9873368169091,
-8.37714322250773));
#39012=CARTESIAN_POINT('Ctrl Pts',(-8.64068822334226,-26.9984809924736,
-8.58124284331955));
#39013=CARTESIAN_POINT('Ctrl Pts',(-8.43576944971309,-27.0096251680382,
-8.77816860405902));
#39014=CARTESIAN_POINT('Ctrl Pts',(-8.22439736760149,-27.0211202963311,
-8.98129595706688));
#39015=CARTESIAN_POINT('Ctrl Pts',(-8.00568009069493,-27.032615424624,-9.17679007677322));
#39016=CARTESIAN_POINT('Ctrl Pts',(-7.78019749632778,-27.0441105529169,
-9.36413248347838));
#39017=CARTESIAN_POINT('Ctrl Pts',(-7.56158732985657,-27.0552553240544,
-9.54576492757846));
#39018=CARTESIAN_POINT('Ctrl Pts',(-7.3366183506728,-27.066400095192,-9.71973503020182));
#39019=CARTESIAN_POINT('Ctrl Pts',(-7.10585275617098,-27.0775448663295,
-9.88561110188022));
#39020=CARTESIAN_POINT('Ctrl Pts',(-6.86420532619913,-27.0892151732001,
-10.0593091199987));
#39021=CARTESIAN_POINT('Ctrl Pts',(-6.61620170182717,-27.1008854800707,
-10.2241312000397));
#39022=CARTESIAN_POINT('Ctrl Pts',(-6.3625226287518,-27.1125557869413,-10.3796317877187));
#39023=CARTESIAN_POINT('Ctrl Pts',(-6.10884355567643,-27.1242260938118,
-10.5351323753978));
#39024=CARTESIAN_POINT('Ctrl Pts',(-5.84948932452369,-27.1358964006824,
-10.6813113028628));
#39025=CARTESIAN_POINT('Ctrl Pts',(-5.58517250510067,-27.147566707553,-10.8177769591662));
#39026=CARTESIAN_POINT('Ctrl Pts',(-5.33270094929267,-27.1587140138001,
-10.9481269559485));
#39027=CARTESIAN_POINT('Ctrl Pts',(-5.07562641811087,-27.1698613200473,
-11.0696540694031));
#39028=CARTESIAN_POINT('Ctrl Pts',(-4.81458622303291,-27.1810086262944,
-11.1820485489458));
#39029=CARTESIAN_POINT('Ctrl Pts',(-4.55359036559887,-27.192154039173,-11.2944239383005));
#39030=CARTESIAN_POINT('Ctrl Pts',(-4.28863043395543,-27.2032994520515,
-11.397669685218));
#39031=CARTESIAN_POINT('Ctrl Pts',(-4.02036484236643,-27.2144448649301,
-11.4915236928905));
#39032=CARTESIAN_POINT('Ctrl Pts',(-3.75212903242545,-27.2255890404947,
-11.5853672813102));
#39033=CARTESIAN_POINT('Ctrl Pts',(-3.48058854705728,-27.2367332160593,
-11.6698211243842));
#39034=CARTESIAN_POINT('Ctrl Pts',(-3.20641930561617,-27.2478773916239,
-11.7446722170766));
#39035=CARTESIAN_POINT('Ctrl Pts',(-2.92361591777954,-27.2593725199168,
-11.8218805227401));
#39036=CARTESIAN_POINT('Ctrl Pts',(-2.63801580485302,-27.2708676482096,
-11.8888713695227));
#39037=CARTESIAN_POINT('Ctrl Pts',(-2.35037625108813,-27.2823627765025,
-11.9454669949869));
#39038=CARTESIAN_POINT('Ctrl Pts',(-2.07150359171745,-27.2935075476401,
-12.0003376564636));
#39039=CARTESIAN_POINT('Ctrl Pts',(-1.79071424363557,-27.3046523187777,
-12.0454373261581));
#39040=CARTESIAN_POINT('Ctrl Pts',(-1.50870843413845,-27.3157970899153,
-12.0806559884288));
#39041=CARTESIAN_POINT('Ctrl Pts',(-1.21340453821725,-27.3274673967858,
-12.1175353995168));
#39042=CARTESIAN_POINT('Ctrl Pts',(-0.916767010429212,-27.3391377036562,
-12.1435794559706));
#39043=CARTESIAN_POINT('Ctrl Pts',(-0.619606806006443,-27.3508080105267,
-12.1587226983738));
#39044=CARTESIAN_POINT('Ctrl Pts',(-0.322446601583674,-27.3624783173972,
-12.173865940777));
#39045=CARTESIAN_POINT('Ctrl Pts',(-0.0247640560390245,-27.3741486242676,
-12.1781083608214));
#39046=CARTESIAN_POINT('Ctrl Pts',(0.272627745971015,-27.3858189311381,
-12.1714470940035));
#39047=CARTESIAN_POINT('Ctrl Pts',(0.556692040867883,-27.3969662373852,
-12.1650843494728));
#39048=CARTESIAN_POINT('Ctrl Pts',(0.840575917591387,-27.4081135436323,
-12.1487718259602));
#39049=CARTESIAN_POINT('Ctrl Pts',(1.12357154681536,-27.4192608498795,-12.1225425232988));
#39050=CARTESIAN_POINT('Ctrl Pts',(1.40651910926765,-27.430406262758,-12.0963176756811));
#39051=CARTESIAN_POINT('Ctrl Pts',(1.68857845992167,-27.4415516756366,-12.0601794363548));
#39052=CARTESIAN_POINT('Ctrl Pts',(1.96904604421539,-27.4526970885152,-12.0142127468162));
#39053=CARTESIAN_POINT('Ctrl Pts',(2.2494824922499,-27.4638412640798,-11.9682511602942));
#39054=CARTESIAN_POINT('Ctrl Pts',(2.52832726361971,-27.4749854396444,-11.9124633454658));
#39055=CARTESIAN_POINT('Ctrl Pts',(2.80488492567743,-27.4861296152089,-11.8469857264921));
#39056=CARTESIAN_POINT('Ctrl Pts',(3.09015195034886,-27.4976247435018,-11.7794460842771));
#39057=CARTESIAN_POINT('Ctrl Pts',(3.37298518903556,-27.5091198717946,-11.7015965039929));
#39058=CARTESIAN_POINT('Ctrl Pts',(3.65263463056829,-27.5206150000875,-11.6136432916451));
#39059=CARTESIAN_POINT('Ctrl Pts',(3.9237607063493,-27.5317597712251,-11.5283707833737));
#39060=CARTESIAN_POINT('Ctrl Pts',(4.19189392120769,-27.5429045423627,-11.4336014988325));
#39061=CARTESIAN_POINT('Ctrl Pts',(4.45636678338372,-27.5540493135003,-11.3295739258789));
#39062=CARTESIAN_POINT('Ctrl Pts',(4.73331095948211,-27.5657196203708,-11.2206408949202));
#39063=CARTESIAN_POINT('Ctrl Pts',(5.00624097019293,-27.5773899272413,-11.1015555262875));
#39064=CARTESIAN_POINT('Ctrl Pts',(5.27441341956734,-27.5890602341118,-10.9726484191141));
#39065=CARTESIAN_POINT('Ctrl Pts',(5.54258586894173,-27.6007305409822,-10.8437413119408));
#39066=CARTESIAN_POINT('Ctrl Pts',(5.80600045840204,-27.6124008478527,-10.7050126194888));
#39067=CARTESIAN_POINT('Ctrl Pts',(6.06394187656684,-27.6240711547232,-10.5568489222693));
#39068=CARTESIAN_POINT('Ctrl Pts',(6.31032521085729,-27.6352185274073,-10.4153242846153));
#39069=CARTESIAN_POINT('Ctrl Pts',(6.55178867359637,-27.6463659000913,-10.2651493360808));
#39070=CARTESIAN_POINT('Ctrl Pts',(6.78772652621512,-27.6575132727754,-10.1066917859068));
#39071=CARTESIAN_POINT('Ctrl Pts',(7.00070243695533,-27.6675757609408,-9.9636556402125));
#39072=CARTESIAN_POINT('Ctrl Pts',(7.20917612457296,-27.6776382491063,-9.81387125325476));
#39073=CARTESIAN_POINT('Ctrl Pts',(7.412721799411,-27.6877007372717,-9.65763976210218));
#39074=CARTESIAN_POINT('Ctrl Pts',(7.41272179941105,-24.687686530294,-9.65763976210214));
#39075=CARTESIAN_POINT('Ctrl Pts',(7.63817646864223,-24.6988315538967,-9.48459202139565));
#39076=CARTESIAN_POINT('Ctrl Pts',(7.85755693299465,-24.7099765774995,-9.30365524582674));
#39077=CARTESIAN_POINT('Ctrl Pts',(8.07031925845228,-24.7211216011022,-9.11528372112763));
#39078=CARTESIAN_POINT('Ctrl Pts',(8.28312306581052,-24.7322687976309,-8.92687546995992));
#39079=CARTESIAN_POINT('Ctrl Pts',(8.48930595663865,-24.7434159941595,-8.73102975054912));
#39080=CARTESIAN_POINT('Ctrl Pts',(8.68835882844288,-24.7545631906881,-8.52823962598488));
#39081=CARTESIAN_POINT('Ctrl Pts',(8.7507460866994,-24.7580569510261,-8.46468103595607));
#39082=CARTESIAN_POINT('Ctrl Pts',(8.8124332169472,-24.761550711364,-8.40044055336482));
#39083=CARTESIAN_POINT('Ctrl Pts',(8.87340530149632,-24.765044471702,-8.33553409238886));
#39084=CARTESIAN_POINT('Ctrl Pts',(9.0679448319984,-24.7761917778973,-8.12844141156305));
#39085=CARTESIAN_POINT('Ctrl Pts',(9.25526037748929,-24.7873390840926,-7.91450441257048));
#39086=CARTESIAN_POINT('Ctrl Pts',(9.43487941609193,-24.7984863902879,-7.69425114314608));
#39087=CARTESIAN_POINT('Ctrl Pts',(9.61446794641304,-24.8096318031139,-7.47403528372458));
#39088=CARTESIAN_POINT('Ctrl Pts',(9.78636241125291,-24.82077721594,-7.24750550239521));
#39089=CARTESIAN_POINT('Ctrl Pts',(9.95013033648356,-24.8319226287661,-7.01522319937076));
#39090=CARTESIAN_POINT('Ctrl Pts',(10.1138800809248,-24.8430668042778,-6.78296668329837));
#39091=CARTESIAN_POINT('Ctrl Pts',(10.2695049335853,-24.8542109797896,-6.54495913870715));
#39092=CARTESIAN_POINT('Ctrl Pts',(10.4166148368308,-24.8653551553013,-6.30179225229755));
#39093=CARTESIAN_POINT('Ctrl Pts',(10.5683575310261,-24.8768502836335,-6.05096754458694));
#39094=CARTESIAN_POINT('Ctrl Pts',(10.711040117134,-24.8883454119656,-5.79465352177919));
#39095=CARTESIAN_POINT('Ctrl Pts',(10.8442841370161,-24.8998405402978,-5.53352977814894));
#39096=CARTESIAN_POINT('Ctrl Pts',(10.9734670445058,-24.9109853113819,-5.28036476221359));
#39097=CARTESIAN_POINT('Ctrl Pts',(11.0937780907114,-24.922130082466,-5.02267912115243));
#39098=CARTESIAN_POINT('Ctrl Pts',(11.2049196053662,-24.9332748535501,-4.76111613881459));
#39099=CARTESIAN_POINT('Ctrl Pts',(11.321302039945,-24.9449451605063,-4.4872190556702));
#39100=CARTESIAN_POINT('Ctrl Pts',(11.4276292249518,-24.9566154674625,-4.20907045001993));
#39101=CARTESIAN_POINT('Ctrl Pts',(11.5236160012056,-24.9682857744186,-3.92743230454166));
#39102=CARTESIAN_POINT('Ctrl Pts',(11.6196027774595,-24.9799560813748,-3.64579415906338));
#39103=CARTESIAN_POINT('Ctrl Pts',(11.7052490450382,-24.991626388331,-3.36066679415295));
#39104=CARTESIAN_POINT('Ctrl Pts',(11.7803292606082,-25.0032966952871,-3.07283139167434));
#39105=CARTESIAN_POINT('Ctrl Pts',(11.8520447828511,-25.0144440015614,-2.79789523103511));
#39106=CARTESIAN_POINT('Ctrl Pts',(11.9141418832278,-25.0255913078357,-2.52040630438659));
#39107=CARTESIAN_POINT('Ctrl Pts',(11.9664583505487,-25.03673861411,-2.24105439349054));
#39108=CARTESIAN_POINT('Ctrl Pts',(12.0187659319259,-25.047884027016,-1.96174993047246));
#39109=CARTESIAN_POINT('Ctrl Pts',(12.0612961478269,-25.0590294399221,-1.680583377044));
#39110=CARTESIAN_POINT('Ctrl Pts',(12.0939379121453,-25.0701748528282,-1.39825463602789));
#39111=CARTESIAN_POINT('Ctrl Pts',(12.1265760527213,-25.0813190284204,-1.11595723788416));
#39112=CARTESIAN_POINT('Ctrl Pts',(12.1493279031616,-25.0924632040126,-0.832498174701055));
#39113=CARTESIAN_POINT('Ctrl Pts',(12.1621341151456,-25.1036073796049,-0.548583644680526));
#39114=CARTESIAN_POINT('Ctrl Pts',(12.1753436207048,-25.1151025078772,-0.255728070579462));
#39115=CARTESIAN_POINT('Ctrl Pts',(12.1779708973995,-25.1265976361494,0.0376118263910138));
#39116=CARTESIAN_POINT('Ctrl Pts',(12.1700088495403,-25.1380927644217,0.330658210410661));
#39117=CARTESIAN_POINT('Ctrl Pts',(12.1622894749236,-25.1492375355872,0.61477290782209));
#39118=CARTESIAN_POINT('Ctrl Pts',(12.1446167235003,-25.1603823067528,0.898611440186133));
#39119=CARTESIAN_POINT('Ctrl Pts',(12.1170370604352,-25.1715270779183,1.18146651498856));
#39120=CARTESIAN_POINT('Ctrl Pts',(12.0881568685195,-25.1831973847439,1.47765972174982));
#39121=CARTESIAN_POINT('Ctrl Pts',(12.0484129862963,-25.1948676915696,1.77277417226269));
#39122=CARTESIAN_POINT('Ctrl Pts',(11.9979196669199,-25.2065379983952,2.06600433594332));
#39123=CARTESIAN_POINT('Ctrl Pts',(11.9474263475436,-25.2182083052209,2.35923449962396));
#39124=CARTESIAN_POINT('Ctrl Pts',(11.8861836565992,-25.2298786120466,2.65058004732725));
#39125=CARTESIAN_POINT('Ctrl Pts',(11.814367381413,-25.2415489188722,2.93924711907746));
#39126=CARTESIAN_POINT('Ctrl Pts',(11.7457695266862,-25.2526962251084,3.21497768016523));
#39127=CARTESIAN_POINT('Ctrl Pts',(11.6675044717985,-25.2638435313446,3.48834690833357));
#39128=CARTESIAN_POINT('Ctrl Pts',(11.5797598749238,-25.2749908375808,3.75867150587886));
#39129=CARTESIAN_POINT('Ctrl Pts',(11.4920301814584,-25.2861362504483,4.02895018882332));
#39130=CARTESIAN_POINT('Ctrl Pts',(11.3948242428908,-25.2972816633159,4.29618501997487));
#39131=CARTESIAN_POINT('Ctrl Pts',(11.2883794518641,-25.3084270761834,4.55970828022289));
#39132=CARTESIAN_POINT('Ctrl Pts',(11.1819464778628,-25.319571251737,4.82320228529501));
#39133=CARTESIAN_POINT('Ctrl Pts',(11.0662767993538,-25.3307154272905,5.08298529497744));
#39134=CARTESIAN_POINT('Ctrl Pts',(10.9416562506894,-25.3418596028441,5.33840882115168));
#39135=CARTESIAN_POINT('Ctrl Pts',(10.8131111475577,-25.3533547311452,5.60187615351543));
#39136=CARTESIAN_POINT('Ctrl Pts',(10.6750423980179,-25.3648498594463,5.86070470407446));
#39137=CARTESIAN_POINT('Ctrl Pts',(10.5278159992574,-25.3763449877474,6.11420808737982));
#39138=CARTESIAN_POINT('Ctrl Pts',(10.3850768775203,-25.3874897588738,6.35998500371434));
#39139=CARTESIAN_POINT('Ctrl Pts',(10.233730207958,-25.3986345300003,6.60075631358498));
#39140=CARTESIAN_POINT('Ctrl Pts',(10.0741552596408,-25.4097793011267,6.83592320426813));
#39141=CARTESIAN_POINT('Ctrl Pts',(9.90705549622338,-25.4214496080151,7.08217947576419));
#39142=CARTESIAN_POINT('Ctrl Pts',(9.7309329452156,-25.4331199149036,7.322289790146));
#39143=CARTESIAN_POINT('Ctrl Pts',(9.54627340902399,-25.444790221792,7.55560151478104));
#39144=CARTESIAN_POINT('Ctrl Pts',(9.36161387283237,-25.4564605286804,7.7889132394161));
#39145=CARTESIAN_POINT('Ctrl Pts',(9.16841756655482,-25.4681308355689,8.01542611667906));
#39146=CARTESIAN_POINT('Ctrl Pts',(8.96721873867355,-25.4798011424573,8.2345272082119));
#39147=CARTESIAN_POINT('Ctrl Pts',(8.77503656446375,-25.4909484487072,8.44380936251634));
#39148=CARTESIAN_POINT('Ctrl Pts',(8.57549596571777,-25.5020957549571,8.64639194661431));
#39149=CARTESIAN_POINT('Ctrl Pts',(8.36908870550682,-25.513243061207,8.84176478364802));
#39150=CARTESIAN_POINT('Ctrl Pts',(8.16271650354294,-25.5243884740884,9.03710443663004));
#39151=CARTESIAN_POINT('Ctrl Pts',(7.94948016228736,-25.5355338869697,9.22523660411083));
#39152=CARTESIAN_POINT('Ctrl Pts',(7.72990765985017,-25.5466792998511,9.405688588306));
#39153=CARTESIAN_POINT('Ctrl Pts',(7.51035953337008,-25.5578234754185,9.58612053952902));
#39154=CARTESIAN_POINT('Ctrl Pts',(7.28447685633972,-25.568967650986,9.75887384069091));
#39155=CARTESIAN_POINT('Ctrl Pts',(7.05282093895285,-25.5801118265534,9.92351586148116));
#39156=CARTESIAN_POINT('Ctrl Pts',(6.81386970621674,-25.5916069548442,10.0933427939065));
#39157=CARTESIAN_POINT('Ctrl Pts',(6.56877595494297,-25.6031020831349,10.2545391062418));
#39158=CARTESIAN_POINT('Ctrl Pts',(6.31818951893443,-25.6145972114257,10.4066772532268));
#39159=CARTESIAN_POINT('Ctrl Pts',(6.07524064445653,-25.6257419825661,10.5541784195464));
#39160=CARTESIAN_POINT('Ctrl Pts',(5.82712918612301,-25.6368867537066,10.6931652624018));
#39161=CARTESIAN_POINT('Ctrl Pts',(5.57447472401811,-25.648031524847,10.8232934821746));
#39162=CARTESIAN_POINT('Ctrl Pts',(5.30990624911238,-25.6597018317129,10.9595579453496));
#39163=CARTESIAN_POINT('Ctrl Pts',(5.04035628966013,-25.6713721385788,11.086108073986));
#39164=CARTESIAN_POINT('Ctrl Pts',(4.76656372398074,-25.6830424454447,11.2026032918796));
#39165=CARTESIAN_POINT('Ctrl Pts',(4.49277115830137,-25.6947127523106,11.3190985097732));
#39166=CARTESIAN_POINT('Ctrl Pts',(4.21473629854935,-25.7063830591765,11.4255386936459));
#39167=CARTESIAN_POINT('Ctrl Pts',(3.9332215664071,-25.7180533660424,11.5216413049335));
#39168=CARTESIAN_POINT('Ctrl Pts',(3.66432281606581,-25.7292006722898,11.613437112148));
#39169=CARTESIAN_POINT('Ctrl Pts',(3.39216892641119,-25.7403479785372,11.6958289457042));
#39170=CARTESIAN_POINT('Ctrl Pts',(3.11743583844296,-25.7514952847845,11.7686041671556));
#39171=CARTESIAN_POINT('Ctrl Pts',(2.84274941385565,-25.7626406976633,11.8413670277446));
#39172=CARTESIAN_POINT('Ctrl Pts',(2.56548492333052,-25.7737861105421,11.9045164689942));
#39173=CARTESIAN_POINT('Ctrl Pts',(2.28633217166219,-25.7849315234209,11.9578900919361));
#39174=CARTESIAN_POINT('Ctrl Pts',(2.00721041028548,-25.7960756989858,12.0112577895767));
#39175=CARTESIAN_POINT('Ctrl Pts',(1.72620106829005,-25.8072198745506,12.0548517859353));
#39176=CARTESIAN_POINT('Ctrl Pts',(1.44400404418548,-25.8183640501154,12.0885608146866));
#39177=CARTESIAN_POINT('Ctrl Pts',(1.15292006251107,-25.8298591784081,12.1233314092329));
#39178=CARTESIAN_POINT('Ctrl Pts',(0.860572674978458,-25.8413543067008,
12.1475843071283));
#39179=CARTESIAN_POINT('Ctrl Pts',(0.567737076103554,-25.8528494349934,
12.1612550693758));
#39180=CARTESIAN_POINT('Ctrl Pts',(0.283826740576818,-25.8639942061314,
12.1745091638625));
#39181=CARTESIAN_POINT('Ctrl Pts',(-0.000542208066812766,-25.8751389772693,
12.177816618211));
#39182=CARTESIAN_POINT('Ctrl Pts',(-0.284660976616601,-25.8862837484072,
12.1711716107527));
#39183=CARTESIAN_POINT('Ctrl Pts',(-0.58217746892358,-25.8979540552772,
12.1642132555533));
#39184=CARTESIAN_POINT('Ctrl Pts',(-0.879419300969854,-25.9096243621473,
12.1463412370951));
#39185=CARTESIAN_POINT('Ctrl Pts',(-1.1755747098368,-25.9212946690173,12.1176100924065));
#39186=CARTESIAN_POINT('Ctrl Pts',(-1.47173011870375,-25.9329649758874,
12.0888789477179));
#39187=CARTESIAN_POINT('Ctrl Pts',(-1.76679877130586,-25.9446352827574,
12.049288717932));
#39188=CARTESIAN_POINT('Ctrl Pts',(-2.05997600562754,-25.9563055896275,
11.9989561673605));
#39189=CARTESIAN_POINT('Ctrl Pts',(-2.34001460716483,-25.9674528958737,
11.9508792520214));
#39190=CARTESIAN_POINT('Ctrl Pts',(-2.61841122729086,-25.9786002021199,
11.8929873201505));
#39191=CARTESIAN_POINT('Ctrl Pts',(-2.89447058978094,-25.9897475083661,
11.8254171281563));
#39192=CARTESIAN_POINT('Ctrl Pts',(-3.1704830636217,-26.0008929212437,11.7578584129511));
#39193=CARTESIAN_POINT('Ctrl Pts',(-3.44415881340236,-26.0120383341213,
11.6806247829658));
#39194=CARTESIAN_POINT('Ctrl Pts',(-3.71481443133084,-26.0231837469989,
11.5939037425181));
#39195=CARTESIAN_POINT('Ctrl Pts',(-3.98544000228493,-26.0343279225626,
11.5071923294519));
#39196=CARTESIAN_POINT('Ctrl Pts',(-4.2530458569297,-26.0454720981264,11.4109956904676));
#39197=CARTESIAN_POINT('Ctrl Pts',(-4.51696419369567,-26.0566162736902,
11.3055510579039));
#39198=CARTESIAN_POINT('Ctrl Pts',(-4.78919385508069,-26.0681114019837,
11.1967857596322));
#39199=CARTESIAN_POINT('Ctrl Pts',(-5.05749970103818,-26.0796065302773,
11.0781806539576));
#39200=CARTESIAN_POINT('Ctrl Pts',(-5.32117022414081,-26.0911016585708,
10.9500501229774));
#39201=CARTESIAN_POINT('Ctrl Pts',(-5.57680439893524,-26.1022464297075,
10.8258248505894));
#39202=CARTESIAN_POINT('Ctrl Pts',(-5.82808137347083,-26.1133912008442,
10.6926463228217));
#39203=CARTESIAN_POINT('Ctrl Pts',(-6.07437599582975,-26.1245359719809,
10.5508486156938));
#39204=CARTESIAN_POINT('Ctrl Pts',(-6.33228473065996,-26.1362062788529,
10.4023643861279));
#39205=CARTESIAN_POINT('Ctrl Pts',(-6.58472964220962,-26.1478765857248,
10.2444286953403));
#39206=CARTESIAN_POINT('Ctrl Pts',(-6.83102404875189,-26.1595468925968,
10.0774778935691));
#39207=CARTESIAN_POINT('Ctrl Pts',(-7.07731845529416,-26.1712171994687,
9.91052709179783));
#39208=CARTESIAN_POINT('Ctrl Pts',(-7.31746208404252,-26.1828875063407,
9.73456137455619));
#39209=CARTESIAN_POINT('Ctrl Pts',(-7.55080426673173,-26.1945578132126,
9.55006833355165));
#39210=CARTESIAN_POINT('Ctrl Pts',(-7.77368930304789,-26.2057051194604,
9.37384328212515));
#39211=CARTESIAN_POINT('Ctrl Pts',(-7.99043566959423,-26.2168524257083,
9.18978577348594));
#39212=CARTESIAN_POINT('Ctrl Pts',(-8.20049831293366,-26.2279997319561,
8.99834860791536));
#39213=CARTESIAN_POINT('Ctrl Pts',(-8.41052527716152,-26.2391451448355,
8.80694395792146));
#39214=CARTESIAN_POINT('Ctrl Pts',(-8.61387058758587,-26.2502905577149,
8.60816233308373));
#39215=CARTESIAN_POINT('Ctrl Pts',(-8.81002389705792,-26.2614359705943,
8.40249541405816));
#39216=CARTESIAN_POINT('Ctrl Pts',(-9.00615543046492,-26.2725801461596,
8.19685132725613));
#39217=CARTESIAN_POINT('Ctrl Pts',(-9.19509637319099,-26.283724321725,7.98432366558186));
#39218=CARTESIAN_POINT('Ctrl Pts',(-9.37637387833569,-26.2948684972904,
7.76544030584642));
#39219=CARTESIAN_POINT('Ctrl Pts',(-9.56336018036558,-26.3063636255827,
7.53966386447199));
#39220=CARTESIAN_POINT('Ctrl Pts',(-9.74219235219411,-26.3178587538749,
7.30712515292804));
#39221=CARTESIAN_POINT('Ctrl Pts',(-9.91239608982264,-26.3293538821672,
7.06844070559192));
#39222=CARTESIAN_POINT('Ctrl Pts',(-10.0774122300974,-26.3404986533055,
6.83703106211519));
#39223=CARTESIAN_POINT('Ctrl Pts',(-10.2343179534282,-26.3516434244438,
6.59984499127896));
#39224=CARTESIAN_POINT('Ctrl Pts',(-10.3827242058869,-26.3627881955821,
6.35747499519189));
#39225=CARTESIAN_POINT('Ctrl Pts',(-10.5381286090834,-26.3744585024514,
6.10367595390744));
#39226=CARTESIAN_POINT('Ctrl Pts',(-10.6842124964244,-26.3861288093207,
5.84419259488536));
#39227=CARTESIAN_POINT('Ctrl Pts',(-10.8205817294359,-26.3977991161899,
5.57973666821271));
#39228=CARTESIAN_POINT('Ctrl Pts',(-10.9569509624474,-26.4094694230592,
5.31528074154007));
#39229=CARTESIAN_POINT('Ctrl Pts',(-11.0836053951668,-26.4211397299285,
5.04585254943003));
#39230=CARTESIAN_POINT('Ctrl Pts',(-11.2002070324854,-26.4328100367977,
4.77219160129437));
#39231=CARTESIAN_POINT('Ctrl Pts',(-11.311144830923,-26.4439134670834,4.51182353269197));
#39232=CARTESIAN_POINT('Ctrl Pts',(-11.4130186487047,-26.4550168973691,
4.24754059388121));
#39233=CARTESIAN_POINT('Ctrl Pts',(-11.5055675162661,-26.4661203276549,
3.97999577620921));
#39234=CARTESIAN_POINT('Ctrl Pts',(-11.5980993129953,-26.4772217098896,
3.71250030773821));
#39235=CARTESIAN_POINT('Ctrl Pts',(-11.6813095047598,-26.4883230921244,
3.44174441751769));
#39236=CARTESIAN_POINT('Ctrl Pts',(-11.7549861724547,-26.4994244743592,
3.16839870208905));
#39237=CARTESIAN_POINT('Ctrl Pts',(-11.8286604607754,-26.5105254980769,
2.89506181430902));
#39238=CARTESIAN_POINT('Ctrl Pts',(-11.8928017662328,-26.5216265217947,
2.61913552911646));
#39239=CARTESIAN_POINT('Ctrl Pts',(-11.9472483674234,-26.5327275455124,
2.34130448619971));
#39240=CARTESIAN_POINT('Ctrl Pts',(-12.0016914005901,-26.5438278417519,
2.06349165025601));
#39241=CARTESIAN_POINT('Ctrl Pts',(-12.0464409474768,-26.5549281379914,
1.78377457205652));
#39242=CARTESIAN_POINT('Ctrl Pts',(-12.0813864435219,-26.5660284342308,
1.50284791389073));
#39243=CARTESIAN_POINT('Ctrl Pts',(-12.1163370539098,-26.5771303550208,
1.22188014154935));
#39244=CARTESIAN_POINT('Ctrl Pts',(-12.1414807111354,-26.5882322758107,
0.939702704299309));
#39245=CARTESIAN_POINT('Ctrl Pts',(-12.1567585846212,-26.5993341966006,
0.657016716103665));
#39246=CARTESIAN_POINT('Ctrl Pts',(-12.1685896895518,-26.6079314657114,
0.438106172572895));
#39247=CARTESIAN_POINT('Ctrl Pts',(-12.1745054475292,-26.6165287348221,
0.218890818353648));
#39248=CARTESIAN_POINT('Ctrl Pts',(-12.174499996235,-26.6251260039329,-0.000302777009381836));
#39249=CARTESIAN_POINT('Origin',(0.,-13.3748739960349,0.));
#39250=CARTESIAN_POINT('',(7.41324263166141,-21.6876995907947,-9.65831743152016));
#39251=CARTESIAN_POINT('',(7.41272179941102,-21.9374490664136,-9.65763976210216));
#39252=CARTESIAN_POINT('',(7.41272179941101,-13.3748739960349,-9.65763976210217));
#39253=CARTESIAN_POINT('',(-12.1737246773372,-20.6251260039651,-0.000249401258526419));
#39254=CARTESIAN_POINT('Ctrl Pts',(-12.1737246773372,-20.6251260039651,
-0.000249401258526419));
#39255=CARTESIAN_POINT('Ctrl Pts',(-12.1741911104616,-20.6550028928951,
-0.762156362199578));
#39256=CARTESIAN_POINT('Ctrl Pts',(-11.9165818304369,-20.7642971896869,
-3.54900219940989));
#39257=CARTESIAN_POINT('Ctrl Pts',(-9.8146932898574,-20.9530088943404,-8.04643346012397));
#39258=CARTESIAN_POINT('Ctrl Pts',(-4.76736202235426,-21.1912611179255,
-11.7619196070543));
#39259=CARTESIAN_POINT('Ctrl Pts',(1.44252672235886,-21.4295133415106,-12.6091655852676));
#39260=CARTESIAN_POINT('Ctrl Pts',(5.51132592543989,-21.594992832467,-11.0618012110311));
#39261=CARTESIAN_POINT('Ctrl Pts',(7.27894291850697,-21.6810549155617,-9.7615477464203));
#39262=CARTESIAN_POINT('Ctrl Pts',(7.41324263166141,-21.6876995907947,-9.65831743152016));
#39263=CARTESIAN_POINT('',(-3.14788895504393,-20.,11.7604951161383));
#39264=CARTESIAN_POINT('Ctrl Pts',(-3.14788895504386,-20.,11.7604951161383));
#39265=CARTESIAN_POINT('Ctrl Pts',(-5.10402892604601,-20.0794174078617,
11.2369022445433));
#39266=CARTESIAN_POINT('Ctrl Pts',(-8.7479903792511,-20.2382522235851,9.19518133472436));
#39267=CARTESIAN_POINT('Ctrl Pts',(-11.6635919119852,-20.4466275582401,
4.5523794220281));
#39268=CARTESIAN_POINT('Ctrl Pts',(-12.1729512588234,-20.5755854850334,
1.26311059284835));
#39269=CARTESIAN_POINT('Ctrl Pts',(-12.1737246773372,-20.6251260039651,
-0.000249401258526419));
#39270=CARTESIAN_POINT('',(3.14799128255578,-20.,11.7604677260283));
#39271=CARTESIAN_POINT('Origin',(0.,-20.,0.));
#39272=CARTESIAN_POINT('',(-12.1744999960254,-20.8748739960726,-0.000311090449405607));
#39273=CARTESIAN_POINT('Ctrl Pts',(3.14799128255578,-20.,11.7604677260283));
#39274=CARTESIAN_POINT('Ctrl Pts',(2.87408896340417,-20.0111238078539,11.8337847175841));
#39275=CARTESIAN_POINT('Ctrl Pts',(2.59758120573957,-20.0222476157078,11.8975402035724));
#39276=CARTESIAN_POINT('Ctrl Pts',(2.3191538849406,-20.0333714235617,11.9515679100261));
#39277=CARTESIAN_POINT('Ctrl Pts',(2.04077383251934,-20.0444933429358,12.0055864442404));
#39278=CARTESIAN_POINT('Ctrl Pts',(1.76047513153612,-20.05561526231,12.0498804447393));
#39279=CARTESIAN_POINT('Ctrl Pts',(1.47895412675117,-20.0667371816841,12.0843346916976));
#39280=CARTESIAN_POINT('Ctrl Pts',(1.19746278684058,-20.0778579291019,12.1187853080887));
#39281=CARTESIAN_POINT('Ctrl Pts',(0.914749667258382,-20.0889786765196,
12.1433982086866));
#39282=CARTESIAN_POINT('Ctrl Pts',(0.631517738404003,-20.1000994239374,
12.1581098693868));
#39283=CARTESIAN_POINT('Ctrl Pts',(0.348264204419321,-20.1112210196536,
12.1728226523028));
#39284=CARTESIAN_POINT('Ctrl Pts',(0.0644920506102684,-20.1223426153698,
12.1776326690876));
#39285=CARTESIAN_POINT('Ctrl Pts',(-0.219092759740573,-20.1334642110859,
12.1725284395901));
#39286=CARTESIAN_POINT('Ctrl Pts',(-0.502675706866799,-20.1445857337304,
12.1674242436287));
#39287=CARTESIAN_POINT('Ctrl Pts',(-0.786071044024664,-20.1557072563748,
12.1524059386502));
#39288=CARTESIAN_POINT('Ctrl Pts',(-1.06857402377094,-20.1668287790193,
12.1275141643175));
#39289=CARTESIAN_POINT('Ctrl Pts',(-1.3511407675224,-20.1779528119128,12.1026167716397));
#39290=CARTESIAN_POINT('Ctrl Pts',(-1.63281448316961,-20.1890768448062,
12.0678414788482));
#39291=CARTESIAN_POINT('Ctrl Pts',(-1.91289517693805,-20.2002008776997,
12.0232808455948));
#39292=CARTESIAN_POINT('Ctrl Pts',(-2.12157502678727,-20.2084890659454,
11.9900800343165));
#39293=CARTESIAN_POINT('Ctrl Pts',(-2.32937062841864,-20.216777254191,11.9514481621977));
#39294=CARTESIAN_POINT('Ctrl Pts',(-2.53599567615223,-20.2250654424367,
11.90744205027));
#39295=CARTESIAN_POINT('Ctrl Pts',(-2.8138996165917,-20.2362127849193,11.8482552670494));
#39296=CARTESIAN_POINT('Ctrl Pts',(-3.08977208840528,-20.2473601274019,
11.7793265425912));
#39297=CARTESIAN_POINT('Ctrl Pts',(-3.36292380790864,-20.2585074698845,
11.700820215361));
#39298=CARTESIAN_POINT('Ctrl Pts',(-3.63602920899082,-20.2696529221088,
11.6223272004729));
#39299=CARTESIAN_POINT('Ctrl Pts',(-3.90641452259799,-20.2807983743331,
11.5342598989376));
#39300=CARTESIAN_POINT('Ctrl Pts',(-4.17340434525454,-20.2919438265575,
11.4368328841953));
#39301=CARTESIAN_POINT('Ctrl Pts',(-4.44036459984081,-20.3030880444669,
11.3394166591108));
#39302=CARTESIAN_POINT('Ctrl Pts',(-4.70392986384688,-20.3142322623763,
11.2326428820654));
#39303=CARTESIAN_POINT('Ctrl Pts',(-4.96344230817088,-20.3253764802857,
11.1167751935289));
#39304=CARTESIAN_POINT('Ctrl Pts',(-5.23112562291956,-20.3368715790971,
10.997259356743));
#39305=CARTESIAN_POINT('Ctrl Pts',(-5.49449649858205,-20.3483666779084,
10.8680677908846));
#39306=CARTESIAN_POINT('Ctrl Pts',(-5.75285652074203,-20.3598617767197,
10.7295429586612));
#39307=CARTESIAN_POINT('Ctrl Pts',(-6.00334380137697,-20.3710065971057,
10.5952392524068));
#39308=CARTESIAN_POINT('Ctrl Pts',(-6.24912084279396,-20.3821514174916,
10.4521627969437));
#39309=CARTESIAN_POINT('Ctrl Pts',(-6.48957628823896,-20.3932962378776,
10.300672300832));
#39310=CARTESIAN_POINT('Ctrl Pts',(-6.74136789952925,-20.4049664759016,
10.1420398521446));
#39311=CARTESIAN_POINT('Ctrl Pts',(-6.98732380660455,-20.4166367139256,
9.97418109459479));
#39312=CARTESIAN_POINT('Ctrl Pts',(-7.22677526496622,-20.4283069519497,
9.79755936545793));
#39313=CARTESIAN_POINT('Ctrl Pts',(-7.4662267233279,-20.4399771899737,9.62093763632107));
#39314=CARTESIAN_POINT('Ctrl Pts',(-7.69917346821438,-20.4516474279977,
9.43555314181049));
#39315=CARTESIAN_POINT('Ctrl Pts',(-7.9249847794445,-20.4633176660218,9.24191898339155));
#39316=CARTESIAN_POINT('Ctrl Pts',(-8.14066853729478,-20.474464498208,9.05696924500836));
#39317=CARTESIAN_POINT('Ctrl Pts',(-8.34990739550198,-20.4856113303942,
8.86443818228698));
#39318=CARTESIAN_POINT('Ctrl Pts',(-8.55217478046388,-20.4967581625804,
8.66479986926402));
#39319=CARTESIAN_POINT('Ctrl Pts',(-8.75440768931906,-20.5079030948094,
8.46519558422725));
#39320=CARTESIAN_POINT('Ctrl Pts',(-8.9496713075049,-20.5190480270384,8.25848665482182));
#39321=CARTESIAN_POINT('Ctrl Pts',(-9.13747528589881,-20.5301929592674,
8.04518462495352));
#39322=CARTESIAN_POINT('Ctrl Pts',(-9.3252583249383,-20.5413366488833,7.83190637736524));
#39323=CARTESIAN_POINT('Ctrl Pts',(-9.5055832087329,-20.5524803384992,7.61203669738287));
#39324=CARTESIAN_POINT('Ctrl Pts',(-9.67799849801041,-20.5636240281151,
7.38612180528512));
#39325=CARTESIAN_POINT('Ctrl Pts',(-9.85585682286771,-20.5751195165727,
7.15307493086235));
#39326=CARTESIAN_POINT('Ctrl Pts',(-10.0252978522716,-20.5866150050304,
6.91359518794776));
#39327=CARTESIAN_POINT('Ctrl Pts',(-10.1858721211816,-20.598110493488,6.66831758248921));
#39328=CARTESIAN_POINT('Ctrl Pts',(-10.3415405228375,-20.6092547716255,
6.43053370177853));
#39329=CARTESIAN_POINT('Ctrl Pts',(-10.4888757631469,-20.620399049763,6.18730120579808));
#39330=CARTESIAN_POINT('Ctrl Pts',(-10.6275127035771,-20.6315433279005,
5.93922755796635));
#39331=CARTESIAN_POINT('Ctrl Pts',(-10.7727033288179,-20.6432144215182,
5.67942690221995));
#39332=CARTESIAN_POINT('Ctrl Pts',(-10.9083532859157,-20.654885515136,5.41431662760413));
#39333=CARTESIAN_POINT('Ctrl Pts',(-11.0340969861489,-20.6665566087537,
5.14462379093558));
#39334=CARTESIAN_POINT('Ctrl Pts',(-11.159840686382,-20.6782277023714,4.87493095426703));
#39335=CARTESIAN_POINT('Ctrl Pts',(-11.2756779958382,-20.6898987959892,
4.60065586355721));
#39336=CARTESIAN_POINT('Ctrl Pts',(-11.3813005554201,-20.7015698896069,
4.32255108902081));
#39337=CARTESIAN_POINT('Ctrl Pts',(-11.4819409370545,-20.7126904619584,
4.05756441614999));
#39338=CARTESIAN_POINT('Ctrl Pts',(-11.5733394354702,-20.7238110343099,
3.7890178396337));
#39339=CARTESIAN_POINT('Ctrl Pts',(-11.6552609185346,-20.7349316066614,
3.51757632054809));
#39340=CARTESIAN_POINT('Ctrl Pts',(-11.7411699266226,-20.7465934724425,
3.23292239600646));
#39341=CARTESIAN_POINT('Ctrl Pts',(-11.8166563253145,-20.7582553382236,
2.94508500430039));
#39342=CARTESIAN_POINT('Ctrl Pts',(-11.8815075908379,-20.7699172040048,
2.65484982981369));
#39343=CARTESIAN_POINT('Ctrl Pts',(-11.9433326930578,-20.7810348905784,
2.37815793821194));
#39344=CARTESIAN_POINT('Ctrl Pts',(-11.995492397791,-20.792152577152,2.09928720024168));
#39345=CARTESIAN_POINT('Ctrl Pts',(-12.0378545291329,-20.8032702637256,
1.81893061589332));
#39346=CARTESIAN_POINT('Ctrl Pts',(-12.0802138904517,-20.8143872233234,
1.53859236381978));
#39347=CARTESIAN_POINT('Ctrl Pts',(-12.1127769187808,-20.8255041829211,
1.25676872584638));
#39348=CARTESIAN_POINT('Ctrl Pts',(-12.1354629727721,-20.8366211425188,
0.974160503447343));
#39349=CARTESIAN_POINT('Ctrl Pts',(-12.1581504142312,-20.8477387820242,
0.691534996870884));
#39350=CARTESIAN_POINT('Ctrl Pts',(-12.1709596530285,-20.8588564215296,
0.408125078448854));
#39351=CARTESIAN_POINT('Ctrl Pts',(-12.1738620090751,-20.869974061035,0.124635604858819));
#39352=CARTESIAN_POINT('Ctrl Pts',(-12.1742883992265,-20.8716073727016,
0.0829876755153614));
#39353=CARTESIAN_POINT('Ctrl Pts',(-12.1745010602666,-20.8732406843683,
0.0413380318515849));
#39354=CARTESIAN_POINT('Ctrl Pts',(-12.1744999960254,-20.8748739960349,
-0.000311089488517879));
#39355=CARTESIAN_POINT('Ctrl Pts',(-12.1744999960254,-20.8748739960726,
-0.000311090449404772));
#39356=CARTESIAN_POINT('Ctrl Pts',(-12.1744923950652,-20.8865393020214,
-0.297774062673808));
#39357=CARTESIAN_POINT('Ctrl Pts',(-12.1635784601364,-20.8982046079702,
-0.595182841827181));
#39358=CARTESIAN_POINT('Ctrl Pts',(-12.1417960711354,-20.909869913919,-0.891761412577232));
#39359=CARTESIAN_POINT('Ctrl Pts',(-12.1231530265705,-20.9198539803433,
-1.14559617382575));
#39360=CARTESIAN_POINT('Ctrl Pts',(-12.0965494250141,-20.9298380467676,
-1.39882274221339));
#39361=CARTESIAN_POINT('Ctrl Pts',(-12.0620392196327,-20.939822113192,-1.65095733259334));
#39362=CARTESIAN_POINT('Ctrl Pts',(-12.0235090635879,-20.9509691820964,
-1.9324620354562));
#39363=CARTESIAN_POINT('Ctrl Pts',(-11.9751141751885,-20.9621162510008,
-2.2126594358091));
#39364=CARTESIAN_POINT('Ctrl Pts',(-11.9169675814257,-20.9732633199052,
-2.49085003829017));
#39365=CARTESIAN_POINT('Ctrl Pts',(-11.8588308783237,-20.9844084927074,
-2.76899332090735));
#39366=CARTESIAN_POINT('Ctrl Pts',(-11.7909458361135,-20.9955536655097,
-3.04513022613635));
#39367=CARTESIAN_POINT('Ctrl Pts',(-11.7134766039781,-21.006698838312,-3.31857139414821));
#39368=CARTESIAN_POINT('Ctrl Pts',(-11.6360159868468,-21.0178427717099,
-3.591982154));
#39369=CARTESIAN_POINT('Ctrl Pts',(-11.5489733807489,-21.0289867051078,
-3.86269751864585));
#39370=CARTESIAN_POINT('Ctrl Pts',(-11.4525631648402,-21.0401306385056,
-4.1300420343315));
#39371=CARTESIAN_POINT('Ctrl Pts',(-11.3531130779724,-21.0516259466949,
-4.40581608024554));
#39372=CARTESIAN_POINT('Ctrl Pts',(-11.2436951564039,-21.0631212548842,
-4.67800297633621));
#39373=CARTESIAN_POINT('Ctrl Pts',(-11.1245994311076,-21.0746165630735,
-4.94588088689978));
#39374=CARTESIAN_POINT('Ctrl Pts',(-11.0091379329855,-21.0857610898951,
-5.20558445552521));
#39375=CARTESIAN_POINT('Ctrl Pts',(-10.8845806273897,-21.0969056167168,
-5.46123786352323));
#39376=CARTESIAN_POINT('Ctrl Pts',(-10.7512401330826,-21.1080501435385,
-5.71220499026376));
#39377=CARTESIAN_POINT('Ctrl Pts',(-10.6116041681331,-21.1197208424116,
-5.97502115196405));
#39378=CARTESIAN_POINT('Ctrl Pts',(-10.4623358132792,-21.1313915412847,
-6.23269757967499));
#39379=CARTESIAN_POINT('Ctrl Pts',(-10.3038478790065,-21.1430622401578,
-6.48453307002857));
#39380=CARTESIAN_POINT('Ctrl Pts',(-10.1453599447337,-21.1547329390309,
-6.73636856038215));
#39381=CARTESIAN_POINT('Ctrl Pts',(-9.97765261724218,-21.166403637904,-6.98236283400452));
#39382=CARTESIAN_POINT('Ctrl Pts',(-9.80119115426147,-21.1780743367771,
-7.22184894660825));
#39383=CARTESIAN_POINT('Ctrl Pts',(-9.63264179299859,-21.1892217499704,
-7.45059708588386));
#39384=CARTESIAN_POINT('Ctrl Pts',(-9.45605571647231,-21.2003691631638,
-7.67347617436341));
#39385=CARTESIAN_POINT('Ctrl Pts',(-9.27186695090699,-21.2115165763572,
-7.88992607662954));
#39386=CARTESIAN_POINT('Ctrl Pts',(-9.08770945043724,-21.2226620973345,
-8.10633923763807));
#39387=CARTESIAN_POINT('Ctrl Pts',(-8.89595201024563,-21.2338076183118,
-8.31632518819218));
#39388=CARTESIAN_POINT('Ctrl Pts',(-8.69706869375794,-21.2449531392891,
-8.51935715802874));
#39389=CARTESIAN_POINT('Ctrl Pts',(-8.49820744079386,-21.2560974238155,
-8.72236660410243));
#39390=CARTESIAN_POINT('Ctrl Pts',(-8.29222207669095,-21.2672417083419,
-8.91842341943104));
#39391=CARTESIAN_POINT('Ctrl Pts',(-8.07962411441024,-21.2783859928682,
-9.10703708237979));
#39392=CARTESIAN_POINT('Ctrl Pts',(-7.86033469976557,-21.2898810401594,
-9.30158729959874));
#39393=CARTESIAN_POINT('Ctrl Pts',(-7.63400990204134,-21.3013760874505,
-9.48821803027954));
#39394=CARTESIAN_POINT('Ctrl Pts',(-7.40124976128749,-21.3128711347417,
-9.66643430749115));
#39395=CARTESIAN_POINT('Ctrl Pts',(-7.17558004674712,-21.3240160156153,
-9.83922169400216));
#39396=CARTESIAN_POINT('Ctrl Pts',(-6.94386147980823,-21.3351608964889,
-10.0040995187547));
#39397=CARTESIAN_POINT('Ctrl Pts',(-6.70667300845964,-21.3463057773625,
-10.1606588077545));
#39398=CARTESIAN_POINT('Ctrl Pts',(-6.45830602768054,-21.3579759078624,
-10.3245966151054));
#39399=CARTESIAN_POINT('Ctrl Pts',(-6.20394142385836,-21.3696460383624,
-10.4794127629059));
#39400=CARTESIAN_POINT('Ctrl Pts',(-5.94427710028753,-21.3813161688623,
-10.6246891721592));
#39401=CARTESIAN_POINT('Ctrl Pts',(-5.68461277671671,-21.3929862993622,
-10.7699655814125));
#39402=CARTESIAN_POINT('Ctrl Pts',(-5.41964903042489,-21.4046564298622,
-10.9057020959921));
#39403=CARTESIAN_POINT('Ctrl Pts',(-5.15011341352574,-21.4163265603621,
-11.031535798692));
#39404=CARTESIAN_POINT('Ctrl Pts',(-4.89265384818702,-21.4274738319566,
-11.1517317519199));
#39405=CARTESIAN_POINT('Ctrl Pts',(-4.63094619394671,-21.4386211035511,
-11.262928642111));
#39406=CARTESIAN_POINT('Ctrl Pts',(-4.36563958289154,-21.4497683751456,
-11.3648423342469));
#39407=CARTESIAN_POINT('Ctrl Pts',(-4.10037804211338,-21.460913753042,-11.4667387132886));
#39408=CARTESIAN_POINT('Ctrl Pts',(-3.83151901407759,-21.4720591309384,
-11.5593549471958));
#39409=CARTESIAN_POINT('Ctrl Pts',(-3.55973082007956,-21.4832045088348,
-11.6424553569501));
#39410=CARTESIAN_POINT('Ctrl Pts',(-3.28797280464175,-21.4943486491813,
-11.7255465394797));
#39411=CARTESIAN_POINT('Ctrl Pts',(-3.01328652773389,-21.5054927895278,
-11.7991239297607));
#39412=CARTESIAN_POINT('Ctrl Pts',(-2.73635584774457,-21.5166369298742,
-11.8630015984368));
#39413=CARTESIAN_POINT('Ctrl Pts',(-2.45070250392632,-21.5281320843803,
-11.9288912631476));
#39414=CARTESIAN_POINT('Ctrl Pts',(-2.16266136567062,-21.5396272388864,
-11.9844601901464));
#39415=CARTESIAN_POINT('Ctrl Pts',(-1.87299620102137,-21.5511223933925,
-12.0295609014195));
#39416=CARTESIAN_POINT('Ctrl Pts',(-1.59216120034856,-21.5622671291682,
-12.0732867608822));
#39417=CARTESIAN_POINT('Ctrl Pts',(-1.30979999634929,-21.573411864944,-12.1071731361329));
#39418=CARTESIAN_POINT('Ctrl Pts',(-1.02661663648201,-21.5845566007197,
-12.1311379734837));
#39419=CARTESIAN_POINT('Ctrl Pts',(-0.730077273105364,-21.596226964591,
-12.156233083644));
#39420=CARTESIAN_POINT('Ctrl Pts',(-0.432636652240616,-21.6078973284622,
-12.1704482314372));
#39421=CARTESIAN_POINT('Ctrl Pts',(-0.135107706832327,-21.6195676923335,
-12.1737502914079));
#39422=CARTESIAN_POINT('Ctrl Pts',(0.162421238575963,-21.6312380562048,
-12.1770523513786));
#39423=CARTESIAN_POINT('Ctrl Pts',(0.460038172932362,-21.642908420076,-12.1694413285824));
#39424=CARTESIAN_POINT('Ctrl Pts',(0.756930527455535,-21.6545787839473,
-12.1509467296423));
#39425=CARTESIAN_POINT('Ctrl Pts',(1.04051646831786,-21.665726093968,-12.1332810398346));
#39426=CARTESIAN_POINT('Ctrl Pts',(1.3235260540737,-21.6768734039887,-12.1056806331005));
#39427=CARTESIAN_POINT('Ctrl Pts',(1.60525332965216,-21.6880207140093,-12.06820666038));
#39428=CARTESIAN_POINT('Ctrl Pts',(1.88693275396258,-21.6991661306637,-12.0307390525992));
#39429=CARTESIAN_POINT('Ctrl Pts',(2.16733003861535,-21.7103115473181,-11.983401262163));
#39430=CARTESIAN_POINT('Ctrl Pts',(2.44574556760614,-21.7214569639726,-11.9263061703335));
#39431=CARTESIAN_POINT('Ctrl Pts',(2.72413018796538,-21.7326011433053,-11.8692174169836));
#39432=CARTESIAN_POINT('Ctrl Pts',(3.00053323073972,-21.743745322638,-11.8023735788288));
#39433=CARTESIAN_POINT('Ctrl Pts',(3.27426524481699,-21.7548895019707,-11.725938655672));
#39434=CARTESIAN_POINT('Ctrl Pts',(3.55661747114512,-21.7663846274341,-11.6470966875695));
#39435=CARTESIAN_POINT('Ctrl Pts',(3.83612742536457,-21.7778797528976,-11.5580498424949));
#39436=CARTESIAN_POINT('Ctrl Pts',(4.11205390419248,-21.7893748783611,-11.4590341189393));
#39437=CARTESIAN_POINT('Ctrl Pts',(4.37957064322365,-21.8005196532004,-11.3630362154728));
#39438=CARTESIAN_POINT('Ctrl Pts',(4.64371884535657,-21.8116644280397,-11.2576681964017));
#39439=CARTESIAN_POINT('Ctrl Pts',(4.90384104113911,-21.8228092028791,-11.1431949320309));
#39440=CARTESIAN_POINT('Ctrl Pts',(5.17622916085864,-21.8344795036546,-11.0233237416993));
#39441=CARTESIAN_POINT('Ctrl Pts',(5.4442021591021,-21.8461498044302,-10.8934680664644));
#39442=CARTESIAN_POINT('Ctrl Pts',(5.70703039091341,-21.8578201052057,-10.7539878355516));
#39443=CARTESIAN_POINT('Ctrl Pts',(5.96985862272471,-21.8694904059813,-10.6145076046387));
#39444=CARTESIAN_POINT('Ctrl Pts',(6.22754179586539,-21.8811607067569,-10.465402983073));
#39445=CARTESIAN_POINT('Ctrl Pts',(6.47938055605088,-21.8928310075324,-10.3070887189288));
#39446=CARTESIAN_POINT('Ctrl Pts',(6.71993112197717,-21.9039782092341,-10.1558705910837));
#39447=CARTESIAN_POINT('Ctrl Pts',(6.95522152552982,-21.9151254109358,-9.99620511839035));
#39448=CARTESIAN_POINT('Ctrl Pts',(7.18466117342611,-21.9262726126375,-9.82848381354232));
#39449=CARTESIAN_POINT('Ctrl Pts',(7.26134175173749,-21.9299980972295,-9.77243000257806));
#39450=CARTESIAN_POINT('Ctrl Pts',(7.33736906532864,-21.9337235818215,-9.71547675626813));
#39451=CARTESIAN_POINT('Ctrl Pts',(7.41272179941102,-21.9374490664136,-9.65763976210216));
#39452=CARTESIAN_POINT('Origin',(0.,-20.,0.));
#39453=CARTESIAN_POINT('',(10.3559140620128,-38.4202905549692,1.73955308634279));
#39454=CARTESIAN_POINT('',(10.355914065439,-39.2383818084129,1.73955306594595));
#39455=CARTESIAN_POINT('',(10.355914065439,-20.,1.73955306594593));
#39456=CARTESIAN_POINT('',(-1.99079507083261,-40.,10.3105642903746));
#39457=CARTESIAN_POINT('Ctrl Pts',(10.355914065439,-39.2383818084129,1.73955306594595));
#39458=CARTESIAN_POINT('Ctrl Pts',(10.3137968728013,-39.2499421539653,1.99028530066326));
#39459=CARTESIAN_POINT('Ctrl Pts',(10.2625736848822,-39.2615024995176,2.23946228145483));
#39460=CARTESIAN_POINT('Ctrl Pts',(10.2023884912638,-39.27306284507,2.48641711571641));
#39461=CARTESIAN_POINT('Ctrl Pts',(10.1812505764525,-39.2771230064615,2.57315124308255));
#39462=CARTESIAN_POINT('Ctrl Pts',(10.1590076417178,-39.2811831678531,2.65961136916614));
#39463=CARTESIAN_POINT('Ctrl Pts',(10.1356674049065,-39.2852433292447,2.74576897373338));
#39464=CARTESIAN_POINT('Ctrl Pts',(10.0690759979193,-39.296827267396,2.99158293685373));
#39465=CARTESIAN_POINT('Ctrl Pts',(9.99352834835741,-39.3084112055473,3.2350090451317));
#39466=CARTESIAN_POINT('Ctrl Pts',(9.90922078800109,-39.3199951436986,3.47539125490169));
#39467=CARTESIAN_POINT('Ctrl Pts',(9.82492758520526,-39.3315771091076,3.71573252762991));
#39468=CARTESIAN_POINT('Ctrl Pts',(9.73187754086394,-39.3431590745166,3.95303067716415));
#39469=CARTESIAN_POINT('Ctrl Pts',(9.63031632810827,-39.3547410399256,4.18664644083677));
#39470=CARTESIAN_POINT('Ctrl Pts',(9.52876641285088,-39.3663217169763,4.42023621748527));
#39471=CARTESIAN_POINT('Ctrl Pts',(9.41870732932391,-39.3779023940269,4.65014417391184));
#39472=CARTESIAN_POINT('Ctrl Pts',(9.30043265936412,-39.3894830710776,4.87575156756713));
#39473=CARTESIAN_POINT('Ctrl Pts',(9.18214987722267,-39.4010645424197,5.10137443510336));
#39474=CARTESIAN_POINT('Ctrl Pts',(9.05565050760297,-39.4126460137618,5.32269590522329));
#39475=CARTESIAN_POINT('Ctrl Pts',(8.92127444893441,-39.4242274851039,5.53912115834182));
#39476=CARTESIAN_POINT('Ctrl Pts',(8.78690188205367,-39.4358086554992,5.75554078760838));
#39477=CARTESIAN_POINT('Ctrl Pts',(8.64465318193135,-39.4473898258945,5.96706422131404));
#39478=CARTESIAN_POINT('Ctrl Pts',(8.49491242743426,-39.4589709962898,6.17312431838393));
#39479=CARTESIAN_POINT('Ctrl Pts',(8.34514009761779,-39.4705546087668,6.37922786663983));
#39480=CARTESIAN_POINT('Ctrl Pts',(8.18787271707229,-39.4821382212438,6.57986555252027));
#39481=CARTESIAN_POINT('Ctrl Pts',(8.02353650941463,-39.4937218337208,6.77450093232635));
#39482=CARTESIAN_POINT('Ctrl Pts',(7.88273702232455,-39.5036464067571,6.94126005398848));
#39483=CARTESIAN_POINT('Ctrl Pts',(7.73674929148784,-39.5135709797935,7.10361351542306));
#39484=CARTESIAN_POINT('Ctrl Pts',(7.58586439719135,-39.5234955528298,7.26124385676619));
#39485=CARTESIAN_POINT('Ctrl Pts',(7.41051234539617,-39.5350294724659,7.44443518223697));
#39486=CARTESIAN_POINT('Ctrl Pts',(7.22849149706608,-39.5465633921019,7.62130277938994));
#39487=CARTESIAN_POINT('Ctrl Pts',(7.04028338094605,-39.558097311738,7.79136771792828));
#39488=CARTESIAN_POINT('Ctrl Pts',(6.85210898568282,-39.5696291648657,7.96140218628521));
#39489=CARTESIAN_POINT('Ctrl Pts',(6.65774974306552,-39.5811610179933,8.12463624128184));
#39490=CARTESIAN_POINT('Ctrl Pts',(6.45772254452777,-39.592692871121,8.28062923562563));
#39491=CARTESIAN_POINT('Ctrl Pts',(6.2577168989946,-39.6042234816872,8.43660542166661));
#39492=CARTESIAN_POINT('Ctrl Pts',(6.05204473760968,-39.6157540922535,8.58534193270929));
#39493=CARTESIAN_POINT('Ctrl Pts',(5.84125523482977,-39.6272847028197,8.72643903786498));
#39494=CARTESIAN_POINT('Ctrl Pts',(5.63044338606736,-39.6388165357562,8.86755110085016));
#39495=CARTESIAN_POINT('Ctrl Pts',(5.41451334264833,-39.6503483686927,9.00102198096848));
#39496=CARTESIAN_POINT('Ctrl Pts',(5.19404353388615,-39.6618802016292,9.12649509768649));
#39497=CARTESIAN_POINT('Ctrl Pts',(4.97357359805668,-39.6734120412121,9.25196828672065));
#39498=CARTESIAN_POINT('Ctrl Pts',(4.74856413637869,-39.6849438807949,9.36944356696252));
#39499=CARTESIAN_POINT('Ctrl Pts',(4.51961908132821,-39.6964757203778,9.47860983265447));
#39500=CARTESIAN_POINT('Ctrl Pts',(4.2906085924439,-39.7080108558277,9.58780729870271));
#39501=CARTESIAN_POINT('Ctrl Pts',(4.05766051472073,-39.7195459912777,9.68869088273747));
#39502=CARTESIAN_POINT('Ctrl Pts',(3.82140107039531,-39.7310811267276,9.7809966189127));
#39503=CARTESIAN_POINT('Ctrl Pts',(3.61203246650753,-39.74130334329,9.86279619805342));
#39504=CARTESIAN_POINT('Ctrl Pts',(3.40006381849039,-39.7515255598525,9.93786007685317));
#39505=CARTESIAN_POINT('Ctrl Pts',(3.18594275547069,-39.7617477764149,10.0060366658764));
#39506=CARTESIAN_POINT('Ctrl Pts',(2.94219156771723,-39.7733845457893,10.0836475478562));
#39507=CARTESIAN_POINT('Ctrl Pts',(2.69557041193126,-39.7850213151637,10.1523578833729));
#39508=CARTESIAN_POINT('Ctrl Pts',(2.44674288382941,-39.7966580845381,10.2119758254919));
#39509=CARTESIAN_POINT('Ctrl Pts',(2.19796065802866,-39.8082927352867,10.2715829133858));
#39510=CARTESIAN_POINT('Ctrl Pts',(1.94697312436059,-39.8199273860353,10.3221008501457));
#39511=CARTESIAN_POINT('Ctrl Pts',(1.69445649222457,-39.8315620367839,10.3633883549715));
#39512=CARTESIAN_POINT('Ctrl Pts',(1.44197452343055,-39.8431950904262,10.4046701921987));
#39513=CARTESIAN_POINT('Ctrl Pts',(1.18796414163377,-39.8548281440686,10.4367240840553));
#39514=CARTESIAN_POINT('Ctrl Pts',(0.933110299572317,-39.866461197711,10.4594601279814));
#39515=CARTESIAN_POINT('Ctrl Pts',(0.678258384732152,-39.8780941633835,
10.482195999976));
#39516=CARTESIAN_POINT('Ctrl Pts',(0.422563290990595,-39.8897271290559,
10.4956141379029));
#39517=CARTESIAN_POINT('Ctrl Pts',(0.166714969412438,-39.9013600947284,
10.4996765244923));
#39518=CARTESIAN_POINT('Ctrl Pts',(-0.0891139888816756,-39.912992179987,
10.5037386036294));
#39519=CARTESIAN_POINT('Ctrl Pts',(-0.345095881899718,-39.9246242652456,
10.4984463426919));
#39520=CARTESIAN_POINT('Ctrl Pts',(-0.600539942610578,-39.9362563505041,
10.4838138469418));
#39521=CARTESIAN_POINT('Ctrl Pts',(-0.856008621241452,-39.9478895567821,
10.4691799410137));
#39522=CARTESIAN_POINT('Ctrl Pts',(-1.11093909430189,-39.9595227630601,
10.4452040152679));
#39523=CARTESIAN_POINT('Ctrl Pts',(-1.36464347042229,-39.971155969338,10.411952228023));
#39524=CARTESIAN_POINT('Ctrl Pts',(-1.57432647122329,-39.9807706462253,
10.3844701063579));
#39525=CARTESIAN_POINT('Ctrl Pts',(-1.7831719369394,-39.9903853231127,10.3506527957081));
#39526=CARTESIAN_POINT('Ctrl Pts',(-1.99079507083262,-40.,10.3105642903746));
#39527=CARTESIAN_POINT('',(-9.92805791774733,-40.,-3.42120840959077));
#39528=CARTESIAN_POINT('Origin',(0.,-40.,0.));
#39529=CARTESIAN_POINT('Ctrl Pts',(-9.92805791774733,-40.,-3.42120840959077));
#39530=CARTESIAN_POINT('Ctrl Pts',(-10.1111316554273,-39.974275356352,-2.88994388159232));
#39531=CARTESIAN_POINT('Ctrl Pts',(-10.2512699108423,-39.9482650884727,
-2.34483397106979));
#39532=CARTESIAN_POINT('Ctrl Pts',(-10.4258103297589,-39.9013712674295,
-1.33653471943939));
#39533=CARTESIAN_POINT('Ctrl Pts',(-10.4744594655408,-39.8804422906188,
-0.87724558207502));
#39534=CARTESIAN_POINT('Ctrl Pts',(-10.5012056208305,-39.8500482605621,
-0.20301881929045));
#39535=CARTESIAN_POINT('Ctrl Pts',(-10.5031627804929,-39.8404701108489,
0.0104120456919794));
#39536=CARTESIAN_POINT('Ctrl Pts',(-10.4917955435466,-39.8165343692672,
0.543764874022827));
#39537=CARTESIAN_POINT('Ctrl Pts',(-10.4703474461067,-39.8021969428684,
0.863292901457895));
#39538=CARTESIAN_POINT('Ctrl Pts',(-10.3665187504896,-39.7604692508409,
1.78037491566855));
#39539=CARTESIAN_POINT('Ctrl Pts',(-10.2472399091455,-39.7325893674282,
2.37244076548405));
#39540=CARTESIAN_POINT('Ctrl Pts',(-9.92787464628935,-39.6803008606321,
3.46310075736266));
#39541=CARTESIAN_POINT('Ctrl Pts',(-9.73909313925916,-39.6559657510241,
3.96306068770059));
#39542=CARTESIAN_POINT('Ctrl Pts',(-9.24174827762745,-39.6029350754466,
5.02710969464659));
#39543=CARTESIAN_POINT('Ctrl Pts',(-8.91779324410202,-39.5744790473274,
5.58163838000466));
#39544=CARTESIAN_POINT('Ctrl Pts',(-8.32975921606371,-39.5286586219976,
6.4049721887172));
#39545=CARTESIAN_POINT('Ctrl Pts',(-8.09836911571393,-39.5116161086541,
6.69514443400181));
#39546=CARTESIAN_POINT('Ctrl Pts',(-7.54702162497352,-39.473359561036,7.31605142355112));
#39547=CARTESIAN_POINT('Ctrl Pts',(-7.21969293083172,-39.4521939186461,
7.63925312036954));
#39548=CARTESIAN_POINT('Ctrl Pts',(-6.44208798764159,-39.4052526783258,
8.31228952144449));
#39549=CARTESIAN_POINT('Ctrl Pts',(-5.98238039401832,-39.3796778943089,
8.64903454742865));
#39550=CARTESIAN_POINT('Ctrl Pts',(-5.22609734299015,-39.3398554548815,
9.11375315455387));
#39551=CARTESIAN_POINT('Ctrl Pts',(-4.94708413805671,-39.3255793506384,
9.26816836557142));
#39552=CARTESIAN_POINT('Ctrl Pts',(-4.12321987217292,-39.2840130284288,
9.67630563918418));
#39553=CARTESIAN_POINT('Ctrl Pts',(-3.56308446885428,-39.2562352744204,
9.89627289381794));
#39554=CARTESIAN_POINT('Ctrl Pts',(-2.47387356679438,-39.2039578764649,
10.2194768411937));
#39555=CARTESIAN_POINT('Ctrl Pts',(-1.94959154804844,-39.1795354772728,
10.3323217948457));
#39556=CARTESIAN_POINT('Ctrl Pts',(-0.784081167148053,-39.1264227880154,
10.4912734210105));
#39557=CARTESIAN_POINT('Ctrl Pts',(-0.142594206303842,-39.0979698678402,
10.5195650321403));
#39558=CARTESIAN_POINT('Ctrl Pts',(0.875743842932602,-39.0517984256466,
10.4712702322068));
#39559=CARTESIAN_POINT('Ctrl Pts',(1.25277714357594,-39.0343907046705,10.4328788093865));
#39560=CARTESIAN_POINT('Ctrl Pts',(2.07834302600836,-38.9958879636132,10.3034122761422));
#39561=CARTESIAN_POINT('Ctrl Pts',(2.52469037367328,-38.9748444752928,10.2032231797783));
#39562=CARTESIAN_POINT('Ctrl Pts',(3.49511560285828,-38.9286845765588,9.91779724428442));
#39563=CARTESIAN_POINT('Ctrl Pts',(4.01391229306815,-38.9037481075462,9.71941672261518));
#39564=CARTESIAN_POINT('Ctrl Pts',(4.80712973622315,-38.8643327691386,9.34170587069367));
#39565=CARTESIAN_POINT('Ctrl Pts',(5.09303602013273,-38.8498249264354,9.18895778939308));
#39566=CARTESIAN_POINT('Ctrl Pts',(5.67977192444265,-38.8189616826282,8.83968135322782));
#39567=CARTESIAN_POINT('Ctrl Pts',(5.9785021257871,-38.8025202094301,8.64044397520996));
#39568=CARTESIAN_POINT('Ctrl Pts',(6.64744313636834,-38.7641356919823,8.142969347724));
#39569=CARTESIAN_POINT('Ctrl Pts',(7.00879760375971,-38.7422381579637,7.83410596090346));
#39570=CARTESIAN_POINT('Ctrl Pts',(7.81805924234976,-38.6904747292404,7.04143980606615));
#39571=CARTESIAN_POINT('Ctrl Pts',(8.24380081964105,-38.6609603045329,6.53786641116099));
#39572=CARTESIAN_POINT('Ctrl Pts',(8.78267329648197,-38.6186340103273,5.76343210837005));
#39573=CARTESIAN_POINT('Ctrl Pts',(8.93610319106947,-38.605826340659,5.52254980062014));
#39574=CARTESIAN_POINT('Ctrl Pts',(9.25387399812242,-38.5771868840938,4.97566542339877));
#39575=CARTESIAN_POINT('Ctrl Pts',(9.41323590069673,-38.5612587613568,4.66716255801877));
#39576=CARTESIAN_POINT('Ctrl Pts',(9.75105795401619,-38.5237102398987,3.92519125036772));
#39577=CARTESIAN_POINT('Ctrl Pts',(9.91636962789157,-38.5021257350487,3.486528524834));
#39578=CARTESIAN_POINT('Ctrl Pts',(10.1806866381941,-38.460399479918,2.61206653098461));
#39579=CARTESIAN_POINT('Ctrl Pts',(10.2822193710206,-38.4402881546397,2.17827260156447));
#39580=CARTESIAN_POINT('Ctrl Pts',(10.3559140620128,-38.4202905549692,1.73955308634279));
#39581=CARTESIAN_POINT('Origin',(0.,-20.,0.));
#39582=CARTESIAN_POINT('',(10.3559140316505,-35.4203776493892,1.73955326709568));
#39583=CARTESIAN_POINT('',(10.3560200556488,-36.2384037331188,1.73957079674365));
#39584=CARTESIAN_POINT('',(10.355914065439,-20.,1.73955306594593));
#39585=CARTESIAN_POINT('',(-10.5009999970343,-37.6589303301852,0.000249570010058437));
#39586=CARTESIAN_POINT('Ctrl Pts',(10.3560200556488,-36.2384037331188,1.73957079674365));
#39587=CARTESIAN_POINT('Ctrl Pts',(10.1265052529798,-36.301008037487,3.09711120286187));
#39588=CARTESIAN_POINT('Ctrl Pts',(8.99979051820545,-36.443029749717,6.07621426388429));
#39589=CARTESIAN_POINT('Ctrl Pts',(5.36308582307284,-36.6644688698086,9.54309573608895));
#39590=CARTESIAN_POINT('Ctrl Pts',(0.142355108328082,-36.9027210933937,
10.9459171808689));
#39591=CARTESIAN_POINT('Ctrl Pts',(-5.1130915350103,-37.1409733169788,9.67934169719463));
#39592=CARTESIAN_POINT('Ctrl Pts',(-9.12160202863017,-37.3792255405639,
6.05225196529256));
#39593=CARTESIAN_POINT('Ctrl Pts',(-10.414406757941,-37.5518778777297,2.35425632961265));
#39594=CARTESIAN_POINT('Ctrl Pts',(-10.5016202439438,-37.6451128070338,
0.304109569145099));
#39595=CARTESIAN_POINT('Ctrl Pts',(-10.5013147911428,-37.6589303284762,
0.000249615072858407));
#39596=CARTESIAN_POINT('Ctrl Pts',(-10.5009999970343,-37.6589303301852,
0.000249570010058437));
#39597=CARTESIAN_POINT('Ctrl Pts',(-10.501006017267,-37.6704495017968,-0.253059966089447));
#39598=CARTESIAN_POINT('Ctrl Pts',(-10.4918420359383,-37.6819686734084,
-0.506405209212665));
#39599=CARTESIAN_POINT('Ctrl Pts',(-10.473526383441,-37.69348784502,-0.759108750684794));
#39600=CARTESIAN_POINT('Ctrl Pts',(-10.4552132077971,-37.7050054588767,
-1.01177811867446));
#39601=CARTESIAN_POINT('Ctrl Pts',(-10.4277508520089,-37.7165230727333,
-1.26380567781993));
#39602=CARTESIAN_POINT('Ctrl Pts',(-10.3912096537856,-37.7280406865899,
-1.51451739213295));
#39603=CARTESIAN_POINT('Ctrl Pts',(-10.3546663419992,-37.7395589666317,
-1.76524360775025));
#39604=CARTESIAN_POINT('Ctrl Pts',(-10.3090431757426,-37.7510772466734,
-2.01465354761341));
#39605=CARTESIAN_POINT('Ctrl Pts',(-10.2544621246906,-37.7625955267152,
-2.26208035517882));
#39606=CARTESIAN_POINT('Ctrl Pts',(-10.1998819030225,-37.7741136317315,
-2.50950340298135));
#39607=CARTESIAN_POINT('Ctrl Pts',(-10.1363441312941,-37.7856317367478,
-2.75494310446557));
#39608=CARTESIAN_POINT('Ctrl Pts',(-10.0640216334083,-37.797149841764,-2.9977440788516));
#39609=CARTESIAN_POINT('Ctrl Pts',(-9.99168235613647,-37.8086706190709,
-3.24060138496548));
#39610=CARTESIAN_POINT('Ctrl Pts',(-9.91055435963564,-37.8201913963777,
-3.48081847072262));
#39611=CARTESIAN_POINT('Ctrl Pts',(-9.82086037821651,-37.8317121736846,
-3.71775502576181));
#39612=CARTESIAN_POINT('Ctrl Pts',(-9.75853086376023,-37.8397181117011,
-3.88240532000537));
#39613=CARTESIAN_POINT('Ctrl Pts',(-9.69206584041268,-37.8477240497176,
-4.04547175410928));
#39614=CARTESIAN_POINT('Ctrl Pts',(-9.62155384401236,-37.8557299877341,
-4.20674489680217));
#39615=CARTESIAN_POINT('Ctrl Pts',(-9.51967913321632,-37.8672968509874,
-4.43974999678158));
#39616=CARTESIAN_POINT('Ctrl Pts',(-9.40932061872502,-37.8788637142408,
-4.66908884410403));
#39617=CARTESIAN_POINT('Ctrl Pts',(-9.29076776060954,-37.8904305774941,
-4.89414297077828));
#39618=CARTESIAN_POINT('Ctrl Pts',(-9.17223566898868,-37.90199541462,-5.1191576754986));
#39619=CARTESIAN_POINT('Ctrl Pts',(-9.04551222811135,-37.9135602517458,
-5.33988891303472));
#39620=CARTESIAN_POINT('Ctrl Pts',(-8.91093325131977,-37.9251250888717,
-5.5557420377951));
#39621=CARTESIAN_POINT('Ctrl Pts',(-8.77636931441983,-37.9366886335676,
-5.77157103986051));
#39622=CARTESIAN_POINT('Ctrl Pts',(-8.63395174090438,-37.9482521782636,
-5.98252278281262));
#39623=CARTESIAN_POINT('Ctrl Pts',(-8.48406072464804,-37.9598157229595,
-6.18802994663767));
#39624=CARTESIAN_POINT('Ctrl Pts',(-8.33415787571558,-37.9713801805032,
-6.39355333358115));
#39625=CARTESIAN_POINT('Ctrl Pts',(-8.17678056561849,-37.9829446380469,
-6.59363105689501));
#39626=CARTESIAN_POINT('Ctrl Pts',(-8.01235129322131,-37.9945090955906,
-6.78772625803478));
#39627=CARTESIAN_POINT('Ctrl Pts',(-7.84792499971694,-38.0060733436261,
-6.98181794283716));
#39628=CARTESIAN_POINT('Ctrl Pts',(-7.6764471798126,-38.0176375916616,-7.16992711216603));
#39629=CARTESIAN_POINT('Ctrl Pts',(-7.49837995428331,-38.0292018396971,
-7.35155079294173));
#39630=CARTESIAN_POINT('Ctrl Pts',(-7.32027095783739,-38.0407688004679,
-7.53321707890549));
#39631=CARTESIAN_POINT('Ctrl Pts',(-7.13556965973494,-38.0523357612386,
-7.70839463730362));
#39632=CARTESIAN_POINT('Ctrl Pts',(-6.94477534909365,-38.0639027220094,
-7.87661706258602));
#39633=CARTESIAN_POINT('Ctrl Pts',(-6.77939063709508,-38.073929218446,-8.02243596705712));
#39634=CARTESIAN_POINT('Ctrl Pts',(-6.60942841200286,-38.0839557148826,
-8.16302942840194));
#39635=CARTESIAN_POINT('Ctrl Pts',(-6.43523447667231,-38.0939822113192,
-8.2981177522525));
#39636=CARTESIAN_POINT('Ctrl Pts',(-6.23426730180032,-38.1055497590579,
-8.45396886584565));
#39637=CARTESIAN_POINT('Ctrl Pts',(-6.02760467181233,-38.1171173067966,
-8.60254000476339));
#39638=CARTESIAN_POINT('Ctrl Pts',(-5.81579678690838,-38.1286848545354,
-8.74342660136094));
#39639=CARTESIAN_POINT('Ctrl Pts',(-5.6040259696663,-38.1402503778832,-8.88428854195134));
#39640=CARTESIAN_POINT('Ctrl Pts',(-5.38711192540109,-38.151815901231,-9.01746847168526));
#39641=CARTESIAN_POINT('Ctrl Pts',(-5.16563415427181,-38.1633814245789,
-9.14260492333671));
#39642=CARTESIAN_POINT('Ctrl Pts',(-4.94418113678743,-38.1749456552965,
-9.26772738900991));
#39643=CARTESIAN_POINT('Ctrl Pts',(-4.71816565177371,-38.1865098860141,
-9.38480803549227));
#39644=CARTESIAN_POINT('Ctrl Pts',(-4.48819309123835,-38.1980741167318,
-9.49353062752527));
#39645=CARTESIAN_POINT('Ctrl Pts',(-4.25820248152583,-38.209639255057,-9.60226175254725));
#39646=CARTESIAN_POINT('Ctrl Pts',(-4.0242544245351,-38.2212043933823,-9.70263339102094));
#39647=CARTESIAN_POINT('Ctrl Pts',(-3.78697688107134,-38.2327695317075,
-9.79437629980752));
#39648=CARTESIAN_POINT('Ctrl Pts',(-3.54970371597984,-38.2443344566267,
-9.88611751570483));
#39649=CARTESIAN_POINT('Ctrl Pts',(-3.30910144613982,-38.2558993815458,
-9.969230222245));
#39650=CARTESIAN_POINT('Ctrl Pts',(-3.06581660782314,-38.2674643064649,
-10.0434938904345));
#39651=CARTESIAN_POINT('Ctrl Pts',(-2.82247493856302,-38.2790319329318,
-10.1177749064964));
#39652=CARTESIAN_POINT('Ctrl Pts',(-2.57644971301954,-38.2905995593986,
-10.1832026711533));
#39653=CARTESIAN_POINT('Ctrl Pts',(-2.32840260480898,-38.3021671858654,
-10.2396065505428));
#39654=CARTESIAN_POINT('Ctrl Pts',(-2.11348977034709,-38.3121896022117,
-10.2884759676535));
#39655=CARTESIAN_POINT('Ctrl Pts',(-1.8970594779061,-38.322212018558,-10.3305720727984));
#39656=CARTESIAN_POINT('Ctrl Pts',(-1.67954864780435,-38.3322344349043,
-10.3658148420497));
#39657=CARTESIAN_POINT('Ctrl Pts',(-1.42852518973776,-38.3438010387753,
-10.406487583748));
#39658=CARTESIAN_POINT('Ctrl Pts',(-1.17598466307407,-38.3553676426462,
-10.4380439947674));
#39659=CARTESIAN_POINT('Ctrl Pts',(-0.922603674343791,-38.3669342465172,
-10.4603921274533));
#39660=CARTESIAN_POINT('Ctrl Pts',(-0.669267061252899,-38.3784988246819,
-10.4827363462202));
#39661=CARTESIAN_POINT('Ctrl Pts',(-0.415090555598662,-38.3900634028467,
-10.4958754816972));
#39662=CARTESIAN_POINT('Ctrl Pts',(-0.160755867377762,-38.4016279810114,
-10.4997694522834));
#39663=CARTESIAN_POINT('Ctrl Pts',(0.0935504220672181,-38.4131912678861,
-10.5036629880725));
#39664=CARTESIAN_POINT('Ctrl Pts',(0.348014582076939,-38.4247545547607,
-10.4983134159245));
#39665=CARTESIAN_POINT('Ctrl Pts',(0.601953812652019,-38.4363178416354,
-10.4837327611607));
#39666=CARTESIAN_POINT('Ctrl Pts',(0.855913169215033,-38.4478820449599,
-10.4691509508051));
#39667=CARTESIAN_POINT('Ctrl Pts',(1.10934723657866,-38.4594462482844,-10.4453366084573));
#39668=CARTESIAN_POINT('Ctrl Pts',(1.36157588496065,-38.4710104516089,-10.4123538217587));
#39669=CARTESIAN_POINT('Ctrl Pts',(1.61380001522755,-38.4825744477865,-10.3793716258734));
#39670=CARTESIAN_POINT('Ctrl Pts',(1.8648184953714,-38.494138443964,-10.3372213518512));
#39671=CARTESIAN_POINT('Ctrl Pts',(2.11395819808633,-38.5057024401416,-10.2860187505538));
#39672=CARTESIAN_POINT('Ctrl Pts',(2.36315646670326,-38.517269154697,-10.2348041129309));
#39673=CARTESIAN_POINT('Ctrl Pts',(2.61047480368251,-38.5288358692525,-10.1745329500001));
#39674=CARTESIAN_POINT('Ctrl Pts',(2.85525066777235,-38.5404025838079,-10.105372067578));
#39675=CARTESIAN_POINT('Ctrl Pts',(3.06746464147513,-38.5504306087018,-10.0454114757192));
#39676=CARTESIAN_POINT('Ctrl Pts',(3.2777676572117,-38.5604586335956,-9.97876982858072));
#39677=CARTESIAN_POINT('Ctrl Pts',(3.48573704249832,-38.5704866584894,-9.90558621539155));
#39678=CARTESIAN_POINT('Ctrl Pts',(3.7256265304417,-38.5820538310016,-9.82117004293616));
#39679=CARTESIAN_POINT('Ctrl Pts',(3.96248524580083,-38.5936210035138,-9.7280223607574));
#39680=CARTESIAN_POINT('Ctrl Pts',(4.19567502657272,-38.605188176026,-9.62638624154433));
#39681=CARTESIAN_POINT('Ctrl Pts',(4.42882392223932,-38.6167533204687,-9.52476794216635));
#39682=CARTESIAN_POINT('Ctrl Pts',(4.65830491383272,-38.6283184649115,-9.41466428731077));
#39683=CARTESIAN_POINT('Ctrl Pts',(4.88350017832237,-38.6398836093542,-9.29636633359107));
#39684=CARTESIAN_POINT('Ctrl Pts',(5.10867022262449,-38.6514474585872,-9.17808162835856));
#39685=CARTESIAN_POINT('Ctrl Pts',(5.32955525319949,-38.6630113078201,-9.0516045853062));
#39686=CARTESIAN_POINT('Ctrl Pts',(5.54556142486565,-38.6745751570531,-8.91727253609768));
#39687=CARTESIAN_POINT('Ctrl Pts',(5.76158452743253,-38.6861399126786,-8.78292995773359));
#39688=CARTESIAN_POINT('Ctrl Pts',(5.97272777009596,-38.6977046683041,-8.64073128630361));
#39689=CARTESIAN_POINT('Ctrl Pts',(6.17842456612679,-38.7092694239296,-8.4910582897941));
#39690=CARTESIAN_POINT('Ctrl Pts',(6.38411756461389,-38.7208339660483,-8.34138805652523));
#39691=CARTESIAN_POINT('Ctrl Pts',(6.58436409479135,-38.732398508167,-8.18424393853169));
#39692=CARTESIAN_POINT('Ctrl Pts',(6.77862844023465,-38.7439630502857,-8.02004971737968));
#39693=CARTESIAN_POINT('Ctrl Pts',(6.9729382103727,-38.7555302965331,-7.85581710280887));
#39694=CARTESIAN_POINT('Ctrl Pts',(7.16126278800572,-38.7670975427805,-7.68453126845112));
#39695=CARTESIAN_POINT('Ctrl Pts',(7.34310018304362,-38.7786647890279,-7.50665576017609));
#39696=CARTESIAN_POINT('Ctrl Pts',(7.50068867675949,-38.7886894867101,-7.35250081634749));
#39697=CARTESIAN_POINT('Ctrl Pts',(7.65340527614783,-38.7987141843923,-7.19339723453153));
#39698=CARTESIAN_POINT('Ctrl Pts',(7.80094570771884,-38.8087388820745,-7.02966905801567));
#39699=CARTESIAN_POINT('Ctrl Pts',(7.97121434138562,-38.8203078571622,-6.8407190013345));
#39700=CARTESIAN_POINT('Ctrl Pts',(8.13464093951674,-38.8318768322498,-6.64555079086006));
#39701=CARTESIAN_POINT('Ctrl Pts',(8.29078139631834,-38.8434458073375,-6.44468345525688));
#39702=CARTESIAN_POINT('Ctrl Pts',(8.44689466556722,-38.8550127680073,-6.24385109515837));
#39703=CARTESIAN_POINT('Ctrl Pts',(8.5957241564423,-38.8665797286772,-6.03732180924652));
#39704=CARTESIAN_POINT('Ctrl Pts',(8.73686658849581,-38.878146689347,-5.82564702113212));
#39705=CARTESIAN_POINT('Ctrl Pts',(8.87799331885999,-38.8897123632258,-5.61399578122867));
#39706=CARTESIAN_POINT('Ctrl Pts',(9.0114345444902,-38.9012780371045,-5.39720041215733));
#39707=CARTESIAN_POINT('Ctrl Pts',(9.1368301862523,-38.9128437109833,-5.17584149173725));
#39708=CARTESIAN_POINT('Ctrl Pts',(9.26223565280195,-38.9244102910362,-4.95446522777686));
#39709=CARTESIAN_POINT('Ctrl Pts',(9.37959413660443,-38.9359768710891,-4.72852493708071));
#39710=CARTESIAN_POINT('Ctrl Pts',(9.48859075957821,-38.947543451142,-4.49862716806439));
#39711=CARTESIAN_POINT('Ctrl Pts',(9.59758534383839,-38.9591098148492,-4.26873369914191));
#39712=CARTESIAN_POINT('Ctrl Pts',(9.69821826319968,-38.9706761785565,-4.03488315072507));
#39713=CARTESIAN_POINT('Ctrl Pts',(9.79022185148165,-38.9822425422638,-3.79770418789712));
#39714=CARTESIAN_POINT('Ctrl Pts',(9.88224680885504,-38.9938115924172,-3.56047013701188));
#39715=CARTESIAN_POINT('Ctrl Pts',(9.9656383284593,-39.0053806425706,-3.31990638438798));
#39716=CARTESIAN_POINT('Ctrl Pts',(10.040177387235,-39.0169496927239,-3.07666037008559));
#39717=CARTESIAN_POINT('Ctrl Pts',(10.1046960415995,-39.0269634970358,-2.86611430497433));
#39718=CARTESIAN_POINT('Ctrl Pts',(10.1625830940347,-39.0369773013477,-2.65355905600627));
#39719=CARTESIAN_POINT('Ctrl Pts',(10.2137267948667,-39.0469911056596,-2.43942328426641));
#39720=CARTESIAN_POINT('Ctrl Pts',(10.2727684666407,-39.0585513122495,-2.19221915659396));
#39721=CARTESIAN_POINT('Ctrl Pts',(10.3228406406017,-39.0701115188394,-1.94283118836035));
#39722=CARTESIAN_POINT('Ctrl Pts',(10.3638016850672,-39.0816717254294,-1.69192660378597));
#39723=CARTESIAN_POINT('Ctrl Pts',(10.4047552723966,-39.0932298274335,-1.44106769748098));
#39724=CARTESIAN_POINT('Ctrl Pts',(10.4366009969215,-39.1047879294375,-1.18869299974049));
#39725=CARTESIAN_POINT('Ctrl Pts',(10.459248571689,-39.1163460314416,-0.935478655887372));
#39726=CARTESIAN_POINT('Ctrl Pts',(10.4818951135829,-39.1279036063227,-0.682275860220792));
#39727=CARTESIAN_POINT('Ctrl Pts',(10.4953443160468,-39.1394611812037,-0.428233770982764));
#39728=CARTESIAN_POINT('Ctrl Pts',(10.4995577670001,-39.1510187560848,-0.17403361005399));
#39729=CARTESIAN_POINT('Ctrl Pts',(10.5037709145365,-39.1625754986876,0.080148245542318));
#39730=CARTESIAN_POINT('Ctrl Pts',(10.4987496354465,-39.1741322412905,0.334487872675474));
#39731=CARTESIAN_POINT('Ctrl Pts',(10.484507635958,-39.1856889838933,0.588303179948864));
#39732=CARTESIAN_POINT('Ctrl Pts',(10.4702642162973,-39.1972468789021,0.842143796971907));
#39733=CARTESIAN_POINT('Ctrl Pts',(10.4467982537258,-39.2088047739108,1.09545971255835));
#39734=CARTESIAN_POINT('Ctrl Pts',(10.4141754984657,-39.2203626689196,1.34757177439928));
#39735=CARTESIAN_POINT('Ctrl Pts',(10.3972221813537,-39.2263690487507,1.47858878072037));
#39736=CARTESIAN_POINT('Ctrl Pts',(10.3777967899006,-39.2323754285818,1.60928074572872));
#39737=CARTESIAN_POINT('Ctrl Pts',(10.355914065439,-39.2383818084129,1.73955306594595));
#39738=CARTESIAN_POINT('Ctrl Pts',(10.3559140620128,-38.4202905549692,1.73955308634279));
#39739=CARTESIAN_POINT('Ctrl Pts',(10.3901797572621,-38.4109923050301,1.53556241881902));
#39740=CARTESIAN_POINT('Ctrl Pts',(10.4184269277223,-38.4017146247187,1.33050703383214));
#39741=CARTESIAN_POINT('Ctrl Pts',(10.4708508938559,-38.3797544179074,0.843834465812173));
#39742=CARTESIAN_POINT('Ctrl Pts',(10.48975813854,-38.3670808333518,0.561912731734641));
#39743=CARTESIAN_POINT('Ctrl Pts',(10.5071834954046,-38.3374403158734,-0.0923601063283838));
#39744=CARTESIAN_POINT('Ctrl Pts',(10.4973145956709,-38.3203433791977,-0.464548735667981));
#39745=CARTESIAN_POINT('Ctrl Pts',(10.4311838802339,-38.2820461086368,-1.29316339726322));
#39746=CARTESIAN_POINT('Ctrl Pts',(10.3646647484045,-38.2608948484542,-1.74802854183711));
#39747=CARTESIAN_POINT('Ctrl Pts',(10.1494117631921,-38.2139371231176,-2.7540656563222));
#39748=CARTESIAN_POINT('Ctrl Pts',(9.98511715635084,-38.1883329299172,-3.30043803410304));
#39749=CARTESIAN_POINT('Ctrl Pts',(9.66125723547714,-38.1485061445656,-4.12702485845205));
#39750=CARTESIAN_POINT('Ctrl Pts',(9.53179053499893,-38.134255539071,-4.41782651024056));
#39751=CARTESIAN_POINT('Ctrl Pts',(9.22254818339391,-38.1030341661345,-5.03530683296236));
#39752=CARTESIAN_POINT('Ctrl Pts',(9.03818034631058,-38.0859550084952,-5.35919663522209));
#39753=CARTESIAN_POINT('Ctrl Pts',(8.58400673720119,-38.0472321860406,-6.06672692249711));
#39754=CARTESIAN_POINT('Ctrl Pts',(8.30492167449681,-38.0256431348001,-6.44349543122926));
#39755=CARTESIAN_POINT('Ctrl Pts',(7.5791323067497,-37.9744519958695,-7.29749083215433));
#39756=CARTESIAN_POINT('Ctrl Pts',(7.1112360631156,-37.9451973819484,-7.75415782841438));
#39757=CARTESIAN_POINT('Ctrl Pts',(6.38436993163142,-37.9032550207047,-8.3420988044031));
#39758=CARTESIAN_POINT('Ctrl Pts',(6.15767308116984,-37.8905801002946,-8.51080788101325));
#39759=CARTESIAN_POINT('Ctrl Pts',(5.61721526489458,-37.8609360383146,-8.88011059507597));
#39760=CARTESIAN_POINT('Ctrl Pts',(5.29904365851014,-37.8438368511782,-9.07356554315724));
#39761=CARTESIAN_POINT('Ctrl Pts',(4.56681816543273,-37.8055381882346,-9.46710216779307));
#39762=CARTESIAN_POINT('Ctrl Pts',(4.14852033770569,-37.7843878111762,-9.65772442316781));
#39763=CARTESIAN_POINT('Ctrl Pts',(3.18639661109217,-37.7374301037312,-10.0220923706011));
#39764=CARTESIAN_POINT('Ctrl Pts',(2.63816848148224,-37.71182509799,-10.1801544672134));
#39765=CARTESIAN_POINT('Ctrl Pts',(1.76798949562244,-37.6719984312672,-10.355984995539));
#39766=CARTESIAN_POINT('Ctrl Pts',(1.45345538753827,-37.6577487729046,-10.4047910044558));
#39767=CARTESIAN_POINT('Ctrl Pts',(0.539891428658019,-37.6162023955407,
-10.5043097723675));
#39768=CARTESIAN_POINT('Ctrl Pts',(-0.0618767836849815,-37.5884173526605,
-10.5179909215598));
#39769=CARTESIAN_POINT('Ctrl Pts',(-1.19571668625076,-37.5361427183569,
-10.4464254414296));
#39770=CARTESIAN_POINT('Ctrl Pts',(-1.72659960155281,-37.5117296979594,
-10.3719053329147));
#39771=CARTESIAN_POINT('Ctrl Pts',(-2.87514527786277,-37.4586378897675,
-10.1200203023151));
#39772=CARTESIAN_POINT('Ctrl Pts',(-3.48692410041871,-37.4301961809479,
-9.92585572806258));
#39773=CARTESIAN_POINT('Ctrl Pts',(-4.42628879678326,-37.3840315895262,
-9.53008277645777));
#39774=CARTESIAN_POINT('Ctrl Pts',(-4.76716988270606,-37.3666188462688,
-9.36421832320812));
#39775=CARTESIAN_POINT('Ctrl Pts',(-5.49783622126238,-37.3281103637103,
-8.95843881850812));
#39776=CARTESIAN_POINT('Ctrl Pts',(-5.88243714631961,-37.3070662058718,
-8.71072745963657));
#39777=CARTESIAN_POINT('Ctrl Pts',(-6.6956376647593,-37.2608882563748,-8.10847682085518));
#39778=CARTESIAN_POINT('Ctrl Pts',(-7.11471826927713,-37.2359349976971,
-7.74336891273555));
#39779=CARTESIAN_POINT('Ctrl Pts',(-7.72945554692772,-37.1965151316267,
-7.11556738192073));
#39780=CARTESIAN_POINT('Ctrl Pts',(-7.94510908897947,-37.1820197022894,
-6.87393774098279));
#39781=CARTESIAN_POINT('Ctrl Pts',(-8.37604325490965,-37.1511351788362,
-6.34367471658154));
#39782=CARTESIAN_POINT('Ctrl Pts',(-8.5883401321292,-37.1346588352614,-6.05315681473701));
#39783=CARTESIAN_POINT('Ctrl Pts',(-9.04519498908136,-37.0962573772053,
-5.35542040341359));
#39784=CARTESIAN_POINT('Ctrl Pts',(-9.27788650950018,-37.0743783528394,
-4.94134718687087));
#39785=CARTESIAN_POINT('Ctrl Pts',(-9.76438598141428,-37.0226517828781,
-3.91920603860562));
#39786=CARTESIAN_POINT('Ctrl Pts',(-9.99059659457535,-36.9931553545202,
-3.30021415839559));
#39787=CARTESIAN_POINT('Ctrl Pts',(-10.2298337347066,-36.9508509584716,
-2.3880845333065));
#39788=CARTESIAN_POINT('Ctrl Pts',(-10.2909528004217,-36.9380474976631,
-2.1092020007096));
#39789=CARTESIAN_POINT('Ctrl Pts',(-10.4009929830534,-36.9094277615045,
-1.48678774644738));
#39790=CARTESIAN_POINT('Ctrl Pts',(-10.4444045131096,-36.8935155138551,
-1.14262562704172));
#39791=CARTESIAN_POINT('Ctrl Pts',(-10.5062602940058,-36.8559775006701,
-0.329943163467894));
#39792=CARTESIAN_POINT('Ctrl Pts',(-10.5105221300925,-36.834387397892,0.138933740486254));
#39793=CARTESIAN_POINT('Ctrl Pts',(-10.4457864132672,-36.7831944355856,
1.25784986902689));
#39794=CARTESIAN_POINT('Ctrl Pts',(-10.3474877776306,-36.7539390575865,
1.90424782655247));
#39795=CARTESIAN_POINT('Ctrl Pts',(-10.1215866452411,-36.7119955421712,
2.81145531001605));
#39796=CARTESIAN_POINT('Ctrl Pts',(-10.042298693671,-36.6993202048601,3.08269862297014));
#39797=CARTESIAN_POINT('Ctrl Pts',(-9.83344905793512,-36.6696760554708,
3.70307247067268));
#39798=CARTESIAN_POINT('Ctrl Pts',(-9.69606756687218,-36.6525772137359,
4.04916333147445));
#39799=CARTESIAN_POINT('Ctrl Pts',(-9.34876826955589,-36.6142787224382,
4.80441326606464));
#39800=CARTESIAN_POINT('Ctrl Pts',(-9.12976287408725,-36.5931281699535,
5.20857900645486));
#39801=CARTESIAN_POINT('Ctrl Pts',(-8.58141072505961,-36.546171337583,6.07904782579627));
#39802=CARTESIAN_POINT('Ctrl Pts',(-8.23910469668343,-36.5205673396163,
6.53548815025067));
#39803=CARTESIAN_POINT('Ctrl Pts',(-7.65053971510121,-36.4807408661328,
7.20010181020881));
#39804=CARTESIAN_POINT('Ctrl Pts',(-7.42889621411317,-36.4664903803013,
7.42857465298755));
#39805=CARTESIAN_POINT('Ctrl Pts',(-6.75982720062115,-36.4249506467354,
8.05832144825503));
#39806=CARTESIAN_POINT('Ctrl Pts',(-6.28792466078623,-36.3971733939983,
8.43171198698677));
#39807=CARTESIAN_POINT('Ctrl Pts',(-5.33995959978761,-36.3449021903794,
9.05772967191153));
#39808=CARTESIAN_POINT('Ctrl Pts',(-4.87128559642516,-36.3204850678521,
9.3181669606982));
#39809=CARTESIAN_POINT('Ctrl Pts',(-3.80269483284357,-36.2673849985505,
9.80922536149846));
#39810=CARTESIAN_POINT('Ctrl Pts',(-3.19735136539581,-36.2389392339463,
10.0228895411061));
#39811=CARTESIAN_POINT('Ctrl Pts',(-2.20908252818157,-36.1927704963497,
10.2729968211003));
#39812=CARTESIAN_POINT('Ctrl Pts',(-1.83708616009955,-36.1753578108648,
10.345994732251));
#39813=CARTESIAN_POINT('Ctrl Pts',(-1.00944489913079,-36.1368493503702,
10.4623539838356));
#39814=CARTESIAN_POINT('Ctrl Pts',(-0.553240485444117,-36.1158051563287,
10.4963691497786));
#39815=CARTESIAN_POINT('Ctrl Pts',(0.45864787437623,-36.0696271333995,10.505646249391));
#39816=CARTESIAN_POINT('Ctrl Pts',(1.01310200751067,-36.0446738379394,10.4667379536435));
#39817=CARTESIAN_POINT('Ctrl Pts',(1.88198526065261,-36.0052539457356,10.3360492225335));
#39818=CARTESIAN_POINT('Ctrl Pts',(2.19968348208914,-35.9907585271613,10.2731285845492));
#39819=CARTESIAN_POINT('Ctrl Pts',(2.8631048523538,-35.9598738800818,10.1095470843209));
#39820=CARTESIAN_POINT('Ctrl Pts',(3.20758192647379,-35.9433973981256,10.0055841389362));
#39821=CARTESIAN_POINT('Ctrl Pts',(3.99259124586388,-35.9049958727585,9.72395463586053));
#39822=CARTESIAN_POINT('Ctrl Pts',(4.42778265998368,-35.8831169218686,9.53366820008739));
#39823=CARTESIAN_POINT('Ctrl Pts',(5.43189959854408,-35.8313904989882,9.01098630818926));
#39824=CARTESIAN_POINT('Ctrl Pts',(5.98538066855198,-35.8018941428165,8.65324505530073));
#39825=CARTESIAN_POINT('Ctrl Pts',(6.72587203654103,-35.7595898261739,8.06939224653938));
#39826=CARTESIAN_POINT('Ctrl Pts',(6.94267731440192,-35.7467863732648,7.88363331407993));
#39827=CARTESIAN_POINT('Ctrl Pts',(7.40550657974443,-35.7181664382889,7.45316498574046));
#39828=CARTESIAN_POINT('Ctrl Pts',(7.64751271967655,-35.702253978042,7.20463262975789));
#39829=CARTESIAN_POINT('Ctrl Pts',(8.18651819305307,-35.6647158186083,6.59327584552595));
#39830=CARTESIAN_POINT('Ctrl Pts',(8.47241349625441,-35.6431257851068,6.22162247519114));
#39831=CARTESIAN_POINT('Ctrl Pts',(9.09488367700752,-35.5919329236896,5.28958695475419));
#39832=CARTESIAN_POINT('Ctrl Pts',(9.40587874698015,-35.5626775776679,4.71445725990754));
#39833=CARTESIAN_POINT('Ctrl Pts',(9.77216655635944,-35.5207341467763,3.85429075895417));
#39834=CARTESIAN_POINT('Ctrl Pts',(9.87230658321486,-35.5080588653303,3.59003563526119));
#39835=CARTESIAN_POINT('Ctrl Pts',(10.0793929160753,-35.4784142164439,2.96905938871876));
#39836=CARTESIAN_POINT('Ctrl Pts',(10.1782653227449,-35.46131480269,2.61005250471027));
#39837=CARTESIAN_POINT('Ctrl Pts',(10.294712872304,-35.4362376597028,2.07835083893602));
#39838=CARTESIAN_POINT('Ctrl Pts',(10.327401447064,-35.4283013538438,1.90929447616562));
#39839=CARTESIAN_POINT('Ctrl Pts',(10.3559140316505,-35.4203776493892,1.73955326709568));
#39840=CARTESIAN_POINT('Origin',(0.,-20.,0.));
#39841=CARTESIAN_POINT('',(10.3559140635165,-32.4208472785242,1.73955307739134));
#39842=CARTESIAN_POINT('',(10.3559140834541,-33.2387841926166,1.73955295869885));
#39843=CARTESIAN_POINT('',(10.355914065439,-20.,1.73955306594593));
#39844=CARTESIAN_POINT('',(-10.500269380848,-34.6589705026193,-0.000127306663085271));
#39845=CARTESIAN_POINT('Ctrl Pts',(10.3559140834541,-33.2387841926166,1.73955295869885));
#39846=CARTESIAN_POINT('Ctrl Pts',(10.2973924631457,-33.2547151709991,2.08794411799455));
#39847=CARTESIAN_POINT('Ctrl Pts',(10.2213159167763,-33.2705378423875,2.43322854355677));
#39848=CARTESIAN_POINT('Ctrl Pts',(10.0296902369874,-33.3030904856052,3.13283812117875));
#39849=CARTESIAN_POINT('Ctrl Pts',(9.91243744699974,-33.3198119228177,3.48610686019093));
#39850=CARTESIAN_POINT('Ctrl Pts',(9.67358767019652,-33.3497085214299,4.09542518246441));
#39851=CARTESIAN_POINT('Ctrl Pts',(9.55991772275114,-33.3627182664138,4.35416770444813));
#39852=CARTESIAN_POINT('Ctrl Pts',(9.14963705242817,-33.4058031174883,5.19431141293116));
#39853=CARTESIAN_POINT('Ctrl Pts',(8.80928925113612,-33.4357290612841,5.75266827127988));
#39854=CARTESIAN_POINT('Ctrl Pts',(8.13937141192271,-33.4864346431677,6.65139524394489));
#39855=CARTESIAN_POINT('Ctrl Pts',(7.83460309708945,-33.5073853499531,7.00781165521474));
#39856=CARTESIAN_POINT('Ctrl Pts',(7.26791133697995,-33.5437698631007,7.58718900440697));
#39857=CARTESIAN_POINT('Ctrl Pts',(7.01697012116098,-33.559164073229,7.81985289790815));
#39858=CARTESIAN_POINT('Ctrl Pts',(6.54052725549038,-33.5875875969846,8.22016201556931));
#39859=CARTESIAN_POINT('Ctrl Pts',(6.3188026777928,-33.6004940022986,8.39179900171593));
#39860=CARTESIAN_POINT('Ctrl Pts',(5.55946885917057,-33.6434471797072,8.93242487697804));
#39861=CARTESIAN_POINT('Ctrl Pts',(4.99439341476788,-33.6733510363649,9.26023662951819));
#39862=CARTESIAN_POINT('Ctrl Pts',(3.97960705825934,-33.7239224104242,9.72886321093979));
#39863=CARTESIAN_POINT('Ctrl Pts',(3.54411172102808,-33.7447639699962,9.89582378205501));
#39864=CARTESIAN_POINT('Ctrl Pts',(2.7605913941199,-33.7815751124668,10.1378281231161));
#39865=CARTESIAN_POINT('Ctrl Pts',(2.41715301412927,-33.7975121448548,10.2251548548626));
#39866=CARTESIAN_POINT('Ctrl Pts',(1.44212485624575,-33.8429520293784,10.4211987459417));
#39867=CARTESIAN_POINT('Ctrl Pts',(0.804060321109531,-33.872630919863,10.489738223794));
#39868=CARTESIAN_POINT('Ctrl Pts',(-0.374906274071377,-33.9265817583329,
10.5081229569328));
#39869=CARTESIAN_POINT('Ctrl Pts',(-0.9133998943455,-33.9509036209578,10.4750619973005));
#39870=CARTESIAN_POINT('Ctrl Pts',(-2.02696949219551,-34.0013955259621,
10.3201400141025));
#39871=CARTESIAN_POINT('Ctrl Pts',(-2.59917281747731,-34.0274921551402,
10.1910837431792));
#39872=CARTESIAN_POINT('Ctrl Pts',(-3.45010919296377,-34.0682987209603,
9.92279147991276));
#39873=CARTESIAN_POINT('Ctrl Pts',(-3.7383994157272,-34.0824360279519,9.81781093406341));
#39874=CARTESIAN_POINT('Ctrl Pts',(-4.57485464171308,-34.1241623004757,
9.47102458040724));
#39875=CARTESIAN_POINT('Ctrl Pts',(-5.10741188418669,-34.1515996155695,
9.1947798699861));
#39876=CARTESIAN_POINT('Ctrl Pts',(-6.00522751287061,-34.1996724107393,
8.62688039775064));
#39877=CARTESIAN_POINT('Ctrl Pts',(-6.38010065476171,-34.2204111088318,
8.35345098065261));
#39878=CARTESIAN_POINT('Ctrl Pts',(-7.01202317295036,-34.2573823172053,
7.82510558741575));
#39879=CARTESIAN_POINT('Ctrl Pts',(-7.27628399454426,-34.2735856944686,
7.58000225246598));
#39880=CARTESIAN_POINT('Ctrl Pts',(-7.97398417276742,-34.3193013815474,
6.86270757933141));
#39881=CARTESIAN_POINT('Ctrl Pts',(-8.37760370138294,-34.34898349091,6.36372128408552));
#39882=CARTESIAN_POINT('Ctrl Pts',(-9.0317606425054,-34.4028879542649,5.38398572717683));
#39883=CARTESIAN_POINT('Ctrl Pts',(-9.29550818257294,-34.4271617497354,
4.91462619281569));
#39884=CARTESIAN_POINT('Ctrl Pts',(-9.77180125519483,-34.4779006412457,
3.89018436110101));
#39885=CARTESIAN_POINT('Ctrl Pts',(-9.97557337595318,-34.5042885065916,
3.33310095202253));
#39886=CARTESIAN_POINT('Ctrl Pts',(-10.3766738294454,-34.5740556996699,
1.8617215613258));
#39887=CARTESIAN_POINT('Ctrl Pts',(-10.5010096203886,-34.6172210591878,
0.932883464836268));
#39888=CARTESIAN_POINT('Ctrl Pts',(-10.5009999994417,-34.6593914973464,
-0.000108285591527979));
#39889=CARTESIAN_POINT('Ctrl Pts',(-10.5001996603171,-34.6589303284762,
-0.000129121781424066));
#39890=CARTESIAN_POINT('Ctrl Pts',(-10.5005152891847,-34.6921039126934,
-0.729869341253787));
#39891=CARTESIAN_POINT('Ctrl Pts',(-10.2460312877903,-34.8046949047723,
-3.20638726464124));
#39892=CARTESIAN_POINT('Ctrl Pts',(-8.31997857721865,-34.9967033047129,
-7.11416351656478));
#39893=CARTESIAN_POINT('Ctrl Pts',(-3.90104496745925,-35.234955528298,-10.2281579100833));
#39894=CARTESIAN_POINT('Ctrl Pts',(1.46924208544258,-35.4732077518831,-10.847796722189));
#39895=CARTESIAN_POINT('Ctrl Pts',(6.48122296440533,-35.7114599754682,-8.82196775299734));
#39896=CARTESIAN_POINT('Ctrl Pts',(9.91261866563249,-35.9497121990533,-4.64471280984987));
#39897=CARTESIAN_POINT('Ctrl Pts',(10.6601686118332,-36.1253601182702,-0.730017845395118));
#39898=CARTESIAN_POINT('Ctrl Pts',(10.4176588865487,-36.2215906296253,1.37498776088105));
#39899=CARTESIAN_POINT('Ctrl Pts',(10.3560200556488,-36.2384037331188,1.73957079674365));
#39900=CARTESIAN_POINT('Ctrl Pts',(10.3559140316505,-35.4203776493892,1.73955326709568));
#39901=CARTESIAN_POINT('Ctrl Pts',(10.4034304843784,-35.4071727318551,1.45667816988187));
#39902=CARTESIAN_POINT('Ctrl Pts',(10.4393491507733,-35.3940054952443,1.1719009550135));
#39903=CARTESIAN_POINT('Ctrl Pts',(10.5116180404197,-35.3549077588437,0.318352847184844));
#39904=CARTESIAN_POINT('Ctrl Pts',(10.5134139691215,-35.3293026198815,-0.252206546139801));
#39905=CARTESIAN_POINT('Ctrl Pts',(10.4440818854216,-35.2894759087867,-1.13726178195156));
#39906=CARTESIAN_POINT('Ctrl Pts',(10.4048365005968,-35.2752263409407,-1.45312921361135));
#39907=CARTESIAN_POINT('Ctrl Pts',(10.2502270180083,-35.233680194394,-2.3589931954694));
#39908=CARTESIAN_POINT('Ctrl Pts',(10.0984985832242,-35.2058952957441,-2.9414765672684));
#39909=CARTESIAN_POINT('Ctrl Pts',(9.7189969494072,-35.1536207816812,-4.01231125877075));
#39910=CARTESIAN_POINT('Ctrl Pts',(9.50186491486644,-35.1292077395162,-4.50245821762584));
#39911=CARTESIAN_POINT('Ctrl Pts',(8.94491295605328,-35.0761157967444,-5.53803274620426));
#39912=CARTESIAN_POINT('Ctrl Pts',(8.59054820514668,-35.0476739799937,-6.07319819802585));
#39913=CARTESIAN_POINT('Ctrl Pts',(7.95252901874559,-35.0015091557408,-6.86817256939595));
#39914=CARTESIAN_POINT('Ctrl Pts',(7.69960773783804,-34.9840962893052,-7.15056194832371));
#39915=CARTESIAN_POINT('Ctrl Pts',(7.10915040816292,-34.9455877054709,-7.74208042091357));
#39916=CARTESIAN_POINT('Ctrl Pts',(6.76553720762311,-34.9245435703629,-8.04408761375559));
#39917=CARTESIAN_POINT('Ctrl Pts',(5.96350937284006,-34.878365307719,-8.66115028556577));
#39918=CARTESIAN_POINT('Ctrl Pts',(5.49753811294207,-34.8534117254717,-8.96415423137284));
#39919=CARTESIAN_POINT('Ctrl Pts',(4.72532047071464,-34.8139917942495,-9.38334294513234));
#39920=CARTESIAN_POINT('Ctrl Pts',(4.43385347036161,-34.7994966265131,-9.52453243285095));
#39921=CARTESIAN_POINT('Ctrl Pts',(3.80579782369832,-34.7686116746212,-9.7936828310673));
#39922=CARTESIAN_POINT('Ctrl Pts',(3.46821353185075,-34.7521346167262,-9.91825586971638));
#39923=CARTESIAN_POINT('Ctrl Pts',(2.67199181621678,-34.7137327959388,-10.1664414903612));
#39924=CARTESIAN_POINT('Ctrl Pts',(2.21001433240182,-34.6918541348475,-10.2767660044488));
#39925=CARTESIAN_POINT('Ctrl Pts',(1.09370362756925,-34.6401282866476,-10.4645693604838));
#39926=CARTESIAN_POINT('Ctrl Pts',(0.436426405672702,-34.6106322098475,
-10.5125142452268));
#39927=CARTESIAN_POINT('Ctrl Pts',(-0.506336637879259,-34.5683282613747,
-10.4926673374378));
#39928=CARTESIAN_POINT('Ctrl Pts',(-0.791290451375485,-34.5555249039931,
-10.4750322533597));
#39929=CARTESIAN_POINT('Ctrl Pts',(-1.42001494035827,-34.5269060974491,
-10.4103188109693));
#39930=CARTESIAN_POINT('Ctrl Pts',(-1.76288243823466,-34.5109946972992,
-10.3577706002858));
#39931=CARTESIAN_POINT('Ctrl Pts',(-2.56139976309308,-34.4734572615843,
-10.1945870267306));
#39932=CARTESIAN_POINT('Ctrl Pts',(-3.01350602193879,-34.4518668767639,
-10.0702117665141));
#39933=CARTESIAN_POINT('Ctrl Pts',(-4.07187183734195,-34.4006734594418,
-9.70136611575844));
#39934=CARTESIAN_POINT('Ctrl Pts',(-4.66660095032496,-34.3714179089478,
-9.42971385312827));
#39935=CARTESIAN_POINT('Ctrl Pts',(-5.47719771372925,-34.3294740674089,
-8.96387775873138));
#39936=CARTESIAN_POINT('Ctrl Pts',(-5.71633828839724,-34.3167985665749,
-8.81330088655491));
#39937=CARTESIAN_POINT('Ctrl Pts',(-6.25572641135615,-34.2871554022145,
-8.44247205014709));
#39938=CARTESIAN_POINT('Ctrl Pts',(-6.55090970155185,-34.2700577442309,
-8.21553486900428));
#39939=CARTESIAN_POINT('Ctrl Pts',(-7.18208544873548,-34.2317600323225,
-7.67460171699667));
#39940=CARTESIAN_POINT('Ctrl Pts',(-7.5107832298162,-34.2106090653874,-7.35323116707836));
#39941=CARTESIAN_POINT('Ctrl Pts',(-8.19765991623217,-34.1636543634845,
-6.58739254236621));
#39942=CARTESIAN_POINT('Ctrl Pts',(-8.54281049591999,-34.1380528074637,
-6.13317018380521));
#39943=CARTESIAN_POINT('Ctrl Pts',(-9.02072917736931,-34.0982268464365,
-5.38504385855398));
#39944=CARTESIAN_POINT('Ctrl Pts',(-9.17975325764311,-34.0839744000038,
-5.1092444357065));
#39945=CARTESIAN_POINT('Ctrl Pts',(-9.60193117811469,-34.0424492306008,
-4.29351694970631));
#39946=CARTESIAN_POINT('Ctrl Pts',(-9.8316221518757,-34.014689211405,-3.73771738646204));
#39947=CARTESIAN_POINT('Ctrl Pts',(-10.1740057745545,-33.9624254866379,
-2.6547031755924));
#39948=CARTESIAN_POINT('Ctrl Pts',(-10.296146051545,-33.9379991811499,-2.13242643317201));
#39949=CARTESIAN_POINT('Ctrl Pts',(-10.4757628900599,-33.8848742327228,
-0.969654362529974));
#39950=CARTESIAN_POINT('Ctrl Pts',(-10.5154101758528,-33.8564132653698,
-0.328583048387017));
#39951=CARTESIAN_POINT('Ctrl Pts',(-10.4850561816332,-33.8101568923869,
0.692317100695039));
#39952=CARTESIAN_POINT('Ctrl Pts',(-10.4530984977893,-33.792670546092,1.071644069824));
#39953=CARTESIAN_POINT('Ctrl Pts',(-10.3376718048425,-33.754111913925,1.90050423182263));
#39954=CARTESIAN_POINT('Ctrl Pts',(-10.245295955518,-33.7330917338209,2.3480408756075));
#39955=CARTESIAN_POINT('Ctrl Pts',(-9.97603185027046,-33.6868155929063,
3.32577058738486));
#39956=CARTESIAN_POINT('Ctrl Pts',(-9.78538152204616,-33.6617450340211,
3.85075162473856));
#39957=CARTESIAN_POINT('Ctrl Pts',(-9.42056376507948,-33.622308830007,4.65051258649645));
#39958=CARTESIAN_POINT('Ctrl Pts',(-9.27383127641737,-33.6079156844688,
4.93663232644258));
#39959=CARTESIAN_POINT('Ctrl Pts',(-8.93286593476369,-33.57688328798,5.53246954001651));
#39960=CARTESIAN_POINT('Ctrl Pts',(-8.7351223270134,-33.56014779091,5.83968615944232));
#39961=CARTESIAN_POINT('Ctrl Pts',(-8.24611489485502,-33.5216091080782,
6.51883189001247));
#39962=CARTESIAN_POINT('Ctrl Pts',(-7.94494948766482,-33.4998559812311,
6.88268608859146));
#39963=CARTESIAN_POINT('Ctrl Pts',(-7.16964126349981,-33.4483743654112,
7.70041144061197));
#39964=CARTESIAN_POINT('Ctrl Pts',(-6.67544960018752,-33.4189948270847,
8.13255731919555));
#39965=CARTESIAN_POINT('Ctrl Pts',(-5.91363380191436,-33.376850463152,8.68221075323397));
#39966=CARTESIAN_POINT('Ctrl Pts',(-5.67638980168292,-33.3640932965017,
8.83914270618776));
#39967=CARTESIAN_POINT('Ctrl Pts',(-5.12453884880811,-33.33489203208,9.17279090510368));
#39968=CARTESIAN_POINT('Ctrl Pts',(-4.80661127922917,-33.3183338833939,
9.34331120445838));
#39969=CARTESIAN_POINT('Ctrl Pts',(-4.06149293300488,-33.2803813268329,
9.694842779255));
#39970=CARTESIAN_POINT('Ctrl Pts',(-3.62979863535035,-33.2590307431067,
9.86459697759156));
#39971=CARTESIAN_POINT('Ctrl Pts',(-2.61783051914968,-33.2105362469365,
10.1870727448933));
#39972=CARTESIAN_POINT('Ctrl Pts',(-2.03284907472676,-33.1836409446823,
10.3197399799795));
#39973=CARTESIAN_POINT('Ctrl Pts',(-1.13606991607934,-33.1430286348071,
10.4438658339172));
#39974=CARTESIAN_POINT('Ctrl Pts',(-0.830699212903186,-33.1292897620925,
10.4725796083236));
#39975=CARTESIAN_POINT('Ctrl Pts',(0.060114311591093,-33.0889460452616,
10.5171304286933));
#39976=CARTESIAN_POINT('Ctrl Pts',(0.646146550315748,-33.0618783915075,
10.4974330077627));
#39977=CARTESIAN_POINT('Ctrl Pts',(1.76254461393008,-33.010148515081,10.3660369150008));
#39978=CARTESIAN_POINT('Ctrl Pts',(2.29200124002334,-32.985570223744,10.2619705275232));
#39979=CARTESIAN_POINT('Ctrl Pts',(3.42871971173839,-32.9322940999666,9.94614158870403));
#39980=CARTESIAN_POINT('Ctrl Pts',(4.02928450183857,-32.9038312804666,9.71836913395691));
#39981=CARTESIAN_POINT('Ctrl Pts',(4.92583995362263,-32.8586592000492,9.28085670850687));
#39982=CARTESIAN_POINT('Ctrl Pts',(5.23817635121195,-32.8422830250682,9.10822124185743));
#39983=CARTESIAN_POINT('Ctrl Pts',(5.9360015240174,-32.8044418227782,8.67473324104618));
#39984=CARTESIAN_POINT('Ctrl Pts',(6.31416943620977,-32.7830185409868,8.40347460828719));
#39985=CARTESIAN_POINT('Ctrl Pts',(7.13503851943344,-32.7344713780611,7.72787977332649));
#39986=CARTESIAN_POINT('Ctrl Pts',(7.56363051133854,-32.7075935546774,7.30892707934504));
#39987=CARTESIAN_POINT('Ctrl Pts',(8.15569447950756,-32.666912001127,6.62200001851131));
#39988=CARTESIAN_POINT('Ctrl Pts',(8.34676680538963,-32.6530835085583,6.37947623164878));
#39989=CARTESIAN_POINT('Ctrl Pts',(8.87134935273919,-32.6124326314509,5.64964597992332));
#39990=CARTESIAN_POINT('Ctrl Pts',(9.1747927854714,-32.5851389945684,5.14222466064249));
#39991=CARTESIAN_POINT('Ctrl Pts',(9.66988887554798,-32.5332666650535,4.12949538277679));
#39992=CARTESIAN_POINT('Ctrl Pts',(9.8684211523254,-32.508767778717,3.62956893963857));
#39993=CARTESIAN_POINT('Ctrl Pts',(10.1681068586645,-32.4631728371292,2.6653267239165));
#39994=CARTESIAN_POINT('Ctrl Pts',(10.2776883767546,-32.4420714192779,2.20524653635747));
#39995=CARTESIAN_POINT('Ctrl Pts',(10.3559140635165,-32.4208472785242,1.73955307739134));
#39996=CARTESIAN_POINT('Origin',(0.,-20.,0.));
#39997=CARTESIAN_POINT('',(10.3559140644695,-29.4200231052784,1.73955307171784));
#39998=CARTESIAN_POINT('',(10.355914067582,-30.237883364692,1.73955305318817));
#39999=CARTESIAN_POINT('',(10.355914065439,-20.,1.73955306594593));
#40000=CARTESIAN_POINT('Ctrl Pts',(10.355914067582,-30.237883364692,1.73955305318817));
#40001=CARTESIAN_POINT('Ctrl Pts',(10.3114209382312,-30.2501434056922,2.00442972556705));
#40002=CARTESIAN_POINT('Ctrl Pts',(10.2567761710981,-30.2625054479786,2.26753619013086));
#40003=CARTESIAN_POINT('Ctrl Pts',(10.0820564267382,-30.2959410316655,2.97186972395602));
#40004=CARTESIAN_POINT('Ctrl Pts',(9.94317807314309,-30.3169874168048,3.40779866310292));
#40005=CARTESIAN_POINT('Ctrl Pts',(9.57385491146637,-30.3631565176171,4.34971157992326));
#40006=CARTESIAN_POINT('Ctrl Pts',(9.33076649203003,-30.3880991411306,4.84927865134335));
#40007=CARTESIAN_POINT('Ctrl Pts',(8.88502861779431,-30.4275175836397,5.60644141465374));
#40008=CARTESIAN_POINT('Ctrl Pts',(8.70787865924656,-30.4420223380472,5.87781969895527));
#40009=CARTESIAN_POINT('Ctrl Pts',(8.30845915225981,-30.4728957279828,6.43191194896451));
#40010=CARTESIAN_POINT('Ctrl Pts',(8.08364542633716,-30.489350864679,6.71227573994664));
#40011=CARTESIAN_POINT('Ctrl Pts',(7.52939490863498,-30.5277414435198,7.33515542024652));
#40012=CARTESIAN_POINT('Ctrl Pts',(7.19018783800821,-30.5496311385861,7.66795289461622));
#40013=CARTESIAN_POINT('Ctrl Pts',(6.32995937279302,-30.6013788961666,8.40448202845157));
#40014=CARTESIAN_POINT('Ctrl Pts',(5.79118879226009,-30.6308856372514,8.78441008173817));
#40015=CARTESIAN_POINT('Ctrl Pts',(4.97272527999633,-30.6732036226496,9.25335046784924));
#40016=CARTESIAN_POINT('Ctrl Pts',(4.71935310668115,-30.6860106091723,9.38510492680094));
#40017=CARTESIAN_POINT('Ctrl Pts',(4.13939223540417,-30.7150184476288,9.65725564221272));
#40018=CARTESIAN_POINT('Ctrl Pts',(3.81041435540575,-30.7313259023401,9.79172519873317));
#40019=CARTESIAN_POINT('Ctrl Pts',(3.03603056528935,-30.7691257738906,10.0633085023197));
#40020=CARTESIAN_POINT('Ctrl Pts',(2.58703129253767,-30.7905772727537,10.187980121067));
#40021=CARTESIAN_POINT('Ctrl Pts',(1.4928232939646,-30.841607684484,10.414776413859));
#40022=CARTESIAN_POINT('Ctrl Pts',(0.843463013178343,-30.870836559206,10.4873581835484));
#40023=CARTESIAN_POINT('Ctrl Pts',(-0.0881747803281585,-30.9126415796335,
10.5043565938054));
#40024=CARTESIAN_POINT('Ctrl Pts',(-0.368005461647002,-30.9251980391295,
10.4982784745436));
#40025=CARTESIAN_POINT('Ctrl Pts',(-0.990582168471628,-30.9534506824108,
10.459831295581));
#40026=CARTESIAN_POINT('Ctrl Pts',(-1.33264996115336,-30.9692424697433,
10.421773096229));
#40027=CARTESIAN_POINT('Ctrl Pts',(-2.13383636408253,-31.006620875628,10.2925397906981));
#40028=CARTESIAN_POINT('Ctrl Pts',(-2.58996854881396,-31.0281734756231,
10.1873306652452));
#40029=CARTESIAN_POINT('Ctrl Pts',(-3.66171524524308,-31.0793098558509,
9.86346650533591));
#40030=CARTESIAN_POINT('Ctrl Pts',(-4.26694314194246,-31.1085460403157,
9.61713830124803));
#40031=CARTESIAN_POINT('Ctrl Pts',(-5.09552466190136,-31.1504467639704,
9.1861909744127));
#40032=CARTESIAN_POINT('Ctrl Pts',(-5.34029022692644,-31.1630970076259,
9.04609159653255));
#40033=CARTESIAN_POINT('Ctrl Pts',(-5.89828934047953,-31.1929261460113,
8.69615535105665));
#40034=CARTESIAN_POINT('Ctrl Pts',(-6.20644769996021,-31.2102414674031,
8.47896959673581));
#40035=CARTESIAN_POINT('Ctrl Pts',(-6.86161829068408,-31.2486841049203,
7.9623261161646));
#40036=CARTESIAN_POINT('Ctrl Pts',(-7.20207319923924,-31.2697605674337,
7.65575566726518));
#40037=CARTESIAN_POINT('Ctrl Pts',(-7.93599382821493,-31.3177570010518,
6.90245623910987));
#40038=CARTESIAN_POINT('Ctrl Pts',(-8.31369470361352,-31.3444305781048,
6.44254610247563));
#40039=CARTESIAN_POINT('Ctrl Pts',(-8.82173608076159,-31.3846310470289,
5.70431655461814));
#40040=CARTESIAN_POINT('Ctrl Pts',(-8.98217157755633,-31.3981715821894,
5.4481964953158));
#40041=CARTESIAN_POINT('Ctrl Pts',(-9.41496419997131,-31.4378225798877,
4.68607875418314));
#40042=CARTESIAN_POINT('Ctrl Pts',(-9.65712582975631,-31.4643767905422,
4.164224602004));
#40043=CARTESIAN_POINT('Ctrl Pts',(-10.0427664017817,-31.5157901472222,
3.11583356842777));
#40044=CARTESIAN_POINT('Ctrl Pts',(-10.1903673845999,-31.5405562692237,
2.59268448520782));
#40045=CARTESIAN_POINT('Ctrl Pts',(-10.3855356098675,-31.5854785372323,
1.61736055470674));
#40046=CARTESIAN_POINT('Ctrl Pts',(-10.4455090940491,-31.6056782382681,
1.16899405645754));
#40047=CARTESIAN_POINT('Ctrl Pts',(-10.4928009493489,-31.6367390070053,
0.479107454901651));
#40048=CARTESIAN_POINT('Ctrl Pts',(-10.501000940797,-31.647525162036,0.239566678794278));
#40049=CARTESIAN_POINT('Ctrl Pts',(-10.5009983454372,-31.6775509147193,
-0.421392116697277));
#40050=CARTESIAN_POINT('Ctrl Pts',(-10.4756367617688,-31.6969890494979,
-0.842353769006203));
#40051=CARTESIAN_POINT('Ctrl Pts',(-10.3561890637257,-31.7428354182167,
-1.83014236019911));
#40052=CARTESIAN_POINT('Ctrl Pts',(-10.2407712106508,-31.7691114954583,
-2.39305363997429));
#40053=CARTESIAN_POINT('Ctrl Pts',(-9.95108184501951,-31.8158885846558,
-3.38501340156538));
#40054=CARTESIAN_POINT('Ctrl Pts',(-9.79336889849711,-31.836466111034,-3.81736511616227));
#40055=CARTESIAN_POINT('Ctrl Pts',(-9.45828426385376,-31.8737271435713,
-4.5770262651996));
#40056=CARTESIAN_POINT('Ctrl Pts',(-9.29090075953251,-31.8903862934732,
-4.90789873504563));
#40057=CARTESIAN_POINT('Ctrl Pts',(-8.96560477009884,-31.9202273653525,
-5.47438083061892));
#40058=CARTESIAN_POINT('Ctrl Pts',(-8.81499189021383,-31.9332460764668,
-5.71374043635616));
#40059=CARTESIAN_POINT('Ctrl Pts',(-8.2853071829109,-31.9763480062886,-6.4846469219686));
#40060=CARTESIAN_POINT('Ctrl Pts',(-7.86635295102467,-32.0062814177709,
-6.98695156839824));
#40061=CARTESIAN_POINT('Ctrl Pts',(-7.07107196393841,-32.0570072298445,
-7.77757295859835));
#40062=CARTESIAN_POINT('Ctrl Pts',(-6.71691114952588,-32.0779705140793,
-8.08540714081939));
#40063=CARTESIAN_POINT('Ctrl Pts',(-6.07134772840634,-32.1143385237302,
-8.57474490007928));
#40064=CARTESIAN_POINT('Ctrl Pts',(-5.78944106251115,-32.1297031700912,
-8.76754711268758));
#40065=CARTESIAN_POINT('Ctrl Pts',(-4.95173434984063,-32.1746158973024,
-9.28242590236286));
#40066=CARTESIAN_POINT('Ctrl Pts',(-4.37515198478731,-32.2043698287966,
-9.567714566424));
#40067=CARTESIAN_POINT('Ctrl Pts',(-3.27633469656313,-32.2582570306378,
-9.99117249070295));
#40068=CARTESIAN_POINT('Ctrl Pts',(-2.76252637197646,-32.2824463257335,
-10.1452631861122));
#40069=CARTESIAN_POINT('Ctrl Pts',(-1.6528006352643,-32.3334627596567,-10.3874682261819));
#40070=CARTESIAN_POINT('Ctrl Pts',(-1.05652574309616,-32.3602061085662,
-10.4649410612404));
#40071=CARTESIAN_POINT('Ctrl Pts',(-0.138988744223851,-32.4022299754543,
-10.5049007721026));
#40072=CARTESIAN_POINT('Ctrl Pts',(0.179382258015516,-32.4169053736573,
-10.5042885408753));
#40073=CARTESIAN_POINT('Ctrl Pts',(1.0661158693777,-32.4578089392958,-10.4622538380019));
#40074=CARTESIAN_POINT('Ctrl Pts',(1.63187667674151,-32.4838947553008,-10.3890502014744));
#40075=CARTESIAN_POINT('Ctrl Pts',(2.6380321696595,-32.5304638734261,-10.1746084646372));
#40076=CARTESIAN_POINT('Ctrl Pts',(3.08039007694023,-32.5510193472215,-10.0495310022941));
#40077=CARTESIAN_POINT('Ctrl Pts',(3.86376117224199,-32.5883240812183,-9.77142666594091));
#40078=CARTESIAN_POINT('Ctrl Pts',(4.20750854472331,-32.6050495749781,-9.62841095747214));
#40079=CARTESIAN_POINT('Ctrl Pts',(4.79762630811627,-32.6349498040389,-9.34524375017742));
#40080=CARTESIAN_POINT('Ctrl Pts',(5.04727137012981,-32.647958979161,-9.21280891394702));
#40081=CARTESIAN_POINT('Ctrl Pts',(5.85485408900499,-32.6910427783843,-8.74170458658902));
#40082=CARTESIAN_POINT('Ctrl Pts',(6.38658555460328,-32.7209682805492,-8.3611171823797));
#40083=CARTESIAN_POINT('Ctrl Pts',(7.23344660815099,-32.7716726285021,-7.62677250465232));
#40084=CARTESIAN_POINT('Ctrl Pts',(7.56640801567001,-32.7926225551551,-7.29656649559687));
#40085=CARTESIAN_POINT('Ctrl Pts',(8.10244086634262,-32.8290081001699,-6.68868094722597));
#40086=CARTESIAN_POINT('Ctrl Pts',(8.31599369584715,-32.8444041521484,-6.42123403183101));
#40087=CARTESIAN_POINT('Ctrl Pts',(8.89230111013309,-32.8893955639791,-5.62240119121903));
#40088=CARTESIAN_POINT('Ctrl Pts',(9.21980186414363,-32.9191971254648,-5.06751232146032));
#40089=CARTESIAN_POINT('Ctrl Pts',(9.72367002799984,-32.9731670180818,-4.00112737558665));
#40090=CARTESIAN_POINT('Ctrl Pts',(9.91534738340422,-32.9973917420132,-3.49924072900911));
#40091=CARTESIAN_POINT('Ctrl Pts',(10.2380025681877,-33.0483735734034,-2.41095010255949));
#40092=CARTESIAN_POINT('Ctrl Pts',(10.3587719016882,-33.0750495258476,-1.82351684226819));
#40093=CARTESIAN_POINT('Ctrl Pts',(10.4660945912271,-33.1170096423701,-0.912811052212753));
#40094=CARTESIAN_POINT('Ctrl Pts',(10.4889567112825,-33.1316924997962,-0.595100631778317));
#40095=CARTESIAN_POINT('Ctrl Pts',(10.5123594700041,-33.1725940482051,0.292277987890723));
#40096=CARTESIAN_POINT('Ctrl Pts',(10.4810610962923,-33.1986703698459,0.861692218080709));
#40097=CARTESIAN_POINT('Ctrl Pts',(10.3893895420749,-33.2292338362686,1.53061625619924));
#40098=CARTESIAN_POINT('Ctrl Pts',(10.3734389374652,-33.2340135101075,1.63522392315164));
#40099=CARTESIAN_POINT('Ctrl Pts',(10.3559140834541,-33.2387841926166,1.73955295869885));
#40100=CARTESIAN_POINT('Ctrl Pts',(10.3559140635165,-32.4208472785242,1.73955307739134));
#40101=CARTESIAN_POINT('Ctrl Pts',(10.3840142550594,-32.4132231534421,1.57226690913973));
#40102=CARTESIAN_POINT('Ctrl Pts',(10.4080682925852,-32.4055801058559,1.40425654582014));
#40103=CARTESIAN_POINT('Ctrl Pts',(10.4726219990082,-32.3807349184809,0.859475314855344));
#40104=CARTESIAN_POINT('Ctrl Pts',(10.4968081321096,-32.363322230047,0.481156570534235));
#40105=CARTESIAN_POINT('Ctrl Pts',(10.5049559575085,-32.3248137670465,-0.354584559322483));
#40106=CARTESIAN_POINT('Ctrl Pts',(10.479577766544,-32.3037695734766,-0.811350842458339));
#40107=CARTESIAN_POINT('Ctrl Pts',(10.357674605056,-32.2575915458211,-1.81591241340187));
#40108=CARTESIAN_POINT('Ctrl Pts',(10.2472581585425,-32.2326382453559,-2.3606523309045));
#40109=CARTESIAN_POINT('Ctrl Pts',(10.0050968633665,-32.1932183520985,-3.20527982365404));
#40110=CARTESIAN_POINT('Ctrl Pts',(9.9015450378348,-32.1787229375252,-3.51214808074864));
#40111=CARTESIAN_POINT('Ctrl Pts',(9.65338821463296,-32.1478382856919,-4.14878388955609));
#40112=CARTESIAN_POINT('Ctrl Pts',(9.50567038336643,-32.1313617946604,-4.47688803502186));
#40113=CARTESIAN_POINT('Ctrl Pts',(9.12470734526825,-32.0929602648949,-5.21879242580949));
#40114=CARTESIAN_POINT('Ctrl Pts',(8.87964062678606,-32.0710813188292,-5.62566181672868));
#40115=CARTESIAN_POINT('Ctrl Pts',(8.23126914645556,-32.0193549055306,-6.55359562379191));
#40116=CARTESIAN_POINT('Ctrl Pts',(7.80483323400473,-31.9898585540253,-7.05606191798641));
#40117=CARTESIAN_POINT('Ctrl Pts',(7.12996222725747,-31.9475542432222,-7.71466684323306));
#40118=CARTESIAN_POINT('Ctrl Pts',(6.9176793353886,-31.9347507915757,-7.90557746905834));
#40119=CARTESIAN_POINT('Ctrl Pts',(6.4308744656234,-31.9061308667628,-8.30873332574502));
#40120=CARTESIAN_POINT('Ctrl Pts',(6.15308232009626,-31.8902184156436,-8.51649927805857));
#40121=CARTESIAN_POINT('Ctrl Pts',(5.47704407567159,-31.8526802623375,-8.97175315950345));
#40122=CARTESIAN_POINT('Ctrl Pts',(5.0714820920083,-31.8310902257059,-9.20708673399354));
#40123=CARTESIAN_POINT('Ctrl Pts',(4.06665395013364,-31.7798973590638,-9.70355424353606));
#40124=CARTESIAN_POINT('Ctrl Pts',(3.45607871398721,-31.75064201096,-9.93741325689463));
#40125=CARTESIAN_POINT('Ctrl Pts',(2.55570528502285,-31.7086985765141,-10.1891691013494));
#40126=CARTESIAN_POINT('Ctrl Pts',(2.28070312194563,-31.696023293501,-10.2542277342069));
#40127=CARTESIAN_POINT('Ctrl Pts',(1.63813055474699,-31.6663786520499,-10.3791138036064));
#40128=CARTESIAN_POINT('Ctrl Pts',(1.26933972813626,-31.6492792475789,-10.4306392692092));
#40129=CARTESIAN_POINT('Ctrl Pts',(0.441105333466639,-31.6109803849645,
-10.5017749605605));
#40130=CARTESIAN_POINT('Ctrl Pts',(-0.0184858864031121,-31.5898300287752,
-10.5110189764899));
#40131=CARTESIAN_POINT('Ctrl Pts',(-1.04623331237894,-31.542872224199,-10.4642657505435));
#40132=CARTESIAN_POINT('Ctrl Pts',(-1.61221589783784,-31.5172671051563,
-10.3921239795205));
#40133=CARTESIAN_POINT('Ctrl Pts',(-2.48082846590605,-31.4774403983088,
-10.2087071239322));
#40134=CARTESIAN_POINT('Ctrl Pts',(-2.78894922061996,-31.4631908145374,
-10.1288681297465));
#40135=CARTESIAN_POINT('Ctrl Pts',(-3.44887523637628,-31.4319707435517,
-9.92547051902809));
#40136=CARTESIAN_POINT('Ctrl Pts',(-3.79868502154433,-31.4148918552876,
-9.7969219746775));
#40137=CARTESIAN_POINT('Ctrl Pts',(-4.57130897833008,-31.3761692272211,
-9.46538340870905));
#40138=CARTESIAN_POINT('Ctrl Pts',(-4.98887166049275,-31.3545800935949,
-9.25210887202356));
#40139=CARTESIAN_POINT('Ctrl Pts',(-5.9506735976996,-31.3033886531654,-8.67675682069549));
#40140=CARTESIAN_POINT('Ctrl Pts',(-6.47812054188313,-31.2741338280961,
-8.29039217654382));
#40141=CARTESIAN_POINT('Ctrl Pts',(-7.1776665519186,-31.2321914486821,-7.67019504976522));
#40142=CARTESIAN_POINT('Ctrl Pts',(-7.38137989220433,-31.2195167317465,
-7.47435728305298));
#40143=CARTESIAN_POINT('Ctrl Pts',(-7.83465925603891,-31.1898682421523,
-7.00197556760979));
#40144=CARTESIAN_POINT('Ctrl Pts',(-8.07790154431399,-31.1727642891347,
-6.71989865895839));
#40145=CARTESIAN_POINT('Ctrl Pts',(-8.58659952401769,-31.1344624286685,
-6.06235346049053));
#40146=CARTESIAN_POINT('Ctrl Pts',(-8.84343503863315,-31.1133136620866,
-5.68115199575005));
#40147=CARTESIAN_POINT('Ctrl Pts',(-9.36124837711765,-31.0663477931969,
-4.79194460638085));
#40148=CARTESIAN_POINT('Ctrl Pts',(-9.60744622474524,-31.040733411439,-4.27699665616754));
#40149=CARTESIAN_POINT('Ctrl Pts',(-9.92403605650205,-31.0009047667007,
-3.44755162367288));
#40150=CARTESIAN_POINT('Ctrl Pts',(-10.0238697397609,-30.9866626265707,
-3.1454944946359));
#40151=CARTESIAN_POINT('Ctrl Pts',(-10.2726032240647,-30.9450737385001,
-2.25985786969892));
#40152=CARTESIAN_POINT('Ctrl Pts',(-10.3852276139088,-30.9172365074899,
-1.66743429848475));
#40153=CARTESIAN_POINT('Ctrl Pts',(-10.5008966525255,-30.8649396524904,
-0.536728397058647));
#40154=CARTESIAN_POINT('Ctrl Pts',(-10.5146055243678,-30.8405548193487,
-0.00141240271758721));
#40155=CARTESIAN_POINT('Ctrl Pts',(-10.4549714258338,-30.7874695772104,
1.17279641169983));
#40156=CARTESIAN_POINT('Ctrl Pts',(-10.3639128066585,-30.7590076115737,
1.80863771145195));
#40157=CARTESIAN_POINT('Ctrl Pts',(-10.1363803408681,-30.7145138031144,
2.76429783978136));
#40158=CARTESIAN_POINT('Ctrl Pts',(-10.0411628828829,-30.6988431170466,
3.09234276003793));
#40159=CARTESIAN_POINT('Ctrl Pts',(-9.77771090054407,-30.6615342781934,
3.85837356241474));
#40160=CARTESIAN_POINT('Ctrl Pts',(-9.59577594160446,-30.6399284224677,
4.29089399154376));
#40161=CARTESIAN_POINT('Ctrl Pts',(-9.09285357153487,-30.5887101334724,
5.29310052073904));
#40162=CARTESIAN_POINT('Ctrl Pts',(-8.74641206874312,-30.5594452052334,
5.84783705291487));
#40163=CARTESIAN_POINT('Ctrl Pts',(-8.17931770227677,-30.5174831260516,
6.59163727651354));
#40164=CARTESIAN_POINT('Ctrl Pts',(-7.99890840640879,-30.5047981949374,
6.80943323918334));
#40165=CARTESIAN_POINT('Ctrl Pts',(-7.56225810640245,-30.4752170860831,
7.29524017171099));
#40166=CARTESIAN_POINT('Ctrl Pts',(-7.3001791479172,-30.4581930889484,7.55748934682704));
#40167=CARTESIAN_POINT('Ctrl Pts',(-6.68307917688385,-30.4199437237763,
8.11287939219607));
#40168=CARTESIAN_POINT('Ctrl Pts',(-6.32152632643383,-30.398766799773,8.39765887737412));
#40169=CARTESIAN_POINT('Ctrl Pts',(-5.46946745949914,-30.3515947339942,
8.98248657036692));
#40170=CARTESIAN_POINT('Ctrl Pts',(-4.97064553220629,-30.3258082299517,
9.26783910066012));
#40171=CARTESIAN_POINT('Ctrl Pts',(-4.16436479706397,-30.2858726134788,
9.64516602787655));
#40172=CARTESIAN_POINT('Ctrl Pts',(-3.87180381808485,-30.2716960682433,
9.76628349993903));
#40173=CARTESIAN_POINT('Ctrl Pts',(-3.22071534644599,-30.2403892234577,
10.0019666444914));
#40174=CARTESIAN_POINT('Ctrl Pts',(-2.86060133255844,-30.2231445594521,
10.1108499331138));
#40175=CARTESIAN_POINT('Ctrl Pts',(-2.04209450231884,-30.1843322759005,
10.3110946018336));
#40176=CARTESIAN_POINT('Ctrl Pts',(-1.58185518085002,-30.1628211623334,
10.3916584936515));
#40177=CARTESIAN_POINT('Ctrl Pts',(-0.488861678338,-30.1126184177227,10.5086673993384));
#40178=CARTESIAN_POINT('Ctrl Pts',(0.144862686984379,-30.0842356954534,
10.5190357669805));
#40179=CARTESIAN_POINT('Ctrl Pts',(1.18351196804607,-30.0375139318949,10.442104678448));
#40180=CARTESIAN_POINT('Ctrl Pts',(1.58923252694197,-30.0191758100296,10.3880982672268));
#40181=CARTESIAN_POINT('Ctrl Pts',(2.62418553411945,-29.9710647030441,10.188268816762));
#40182=CARTESIAN_POINT('Ctrl Pts',(3.2449840613249,-29.9411576434855,10.0078599991273));
#40183=CARTESIAN_POINT('Ctrl Pts',(4.33730619894142,-29.8874258788518,9.57801309186354));
#40184=CARTESIAN_POINT('Ctrl Pts',(4.81399661233378,-29.8635324481433,9.34751391885331));
#40185=CARTESIAN_POINT('Ctrl Pts',(5.79477555919283,-29.8125842367779,8.77826357532591));
#40186=CARTESIAN_POINT('Ctrl Pts',(6.29098588323357,-29.7856360743672,8.42975819579932));
#40187=CARTESIAN_POINT('Ctrl Pts',(6.98779898456601,-29.7440177658387,7.84439748658059));
#40188=CARTESIAN_POINT('Ctrl Pts',(7.21253448021068,-29.7299672068071,7.63827535935543));
#40189=CARTESIAN_POINT('Ctrl Pts',(7.85039218361032,-29.6883834983211,6.99996121811215));
#40190=CARTESIAN_POINT('Ctrl Pts',(8.23595657125194,-29.6609979484456,6.54195421658664));
#40191=CARTESIAN_POINT('Ctrl Pts',(8.84642545299348,-29.6130703647771,5.67667088791222));
#40192=CARTESIAN_POINT('Ctrl Pts',(9.08724967439003,-29.5924236753169,5.28258781613396));
#40193=CARTESIAN_POINT('Ctrl Pts',(9.47124289689141,-29.5552931414778,4.54977980894248));
#40194=CARTESIAN_POINT('Ctrl Pts',(9.62403962162961,-29.5388356072143,4.21696526539511));
#40195=CARTESIAN_POINT('Ctrl Pts',(9.86377048822363,-29.5091712328099,3.613493397077));
#40196=CARTESIAN_POINT('Ctrl Pts',(9.95768563518622,-29.4961204860429,3.34601210295084));
#40197=CARTESIAN_POINT('Ctrl Pts',(10.174812874006,-29.4619524881759,2.6370503212561));
#40198=CARTESIAN_POINT('Ctrl Pts',(10.2800944753069,-29.4408860330383,2.19092254272531));
#40199=CARTESIAN_POINT('Ctrl Pts',(10.3559140644695,-29.4200231052784,1.73955307171784));
#40200=CARTESIAN_POINT('Origin',(0.,-20.,0.));
#40201=CARTESIAN_POINT('',(10.3559140653568,-26.421010256864,1.73955306643568));
#40202=CARTESIAN_POINT('',(10.3559140724569,-27.2388808356861,1.73955302416723));
#40203=CARTESIAN_POINT('',(10.355914065439,-20.,1.73955306594593));
#40204=CARTESIAN_POINT('',(-10.5009997442766,-28.659363079701,0.000175012915686588));
#40205=CARTESIAN_POINT('Ctrl Pts',(10.3559140724569,-27.2388808356861,1.73955302416722));
#40206=CARTESIAN_POINT('Ctrl Pts',(10.3180828494693,-27.2493073019969,1.96477001328604));
#40207=CARTESIAN_POINT('Ctrl Pts',(10.2728958110239,-27.2596885430775,2.18880581571025));
#40208=CARTESIAN_POINT('Ctrl Pts',(10.1134262702403,-27.2911089272256,2.86472517941119));
#40209=CARTESIAN_POINT('Ctrl Pts',(9.97639339121059,-27.3119500059299,3.3105317825855));
#40210=CARTESIAN_POINT('Ctrl Pts',(9.68387378266125,-27.3487618546298,4.07664467838913));
#40211=CARTESIAN_POINT('Ctrl Pts',(9.54088168897673,-27.3647000906728,4.40091086813838));
#40212=CARTESIAN_POINT('Ctrl Pts',(9.09416197629864,-27.4101343112315,5.28934135904937));
#40213=CARTESIAN_POINT('Ctrl Pts',(8.75483590697131,-27.4398061706659,5.83384743376745));
#40214=CARTESIAN_POINT('Ctrl Pts',(8.04268084402705,-27.4937429142223,6.7732053918681));
#40215=CARTESIAN_POINT('Ctrl Pts',(7.68479268516474,-27.518057718188,7.17669897934601));
#40216=CARTESIAN_POINT('Ctrl Pts',(6.87612615325683,-27.5685635894673,7.95822424585137));
#40217=CARTESIAN_POINT('Ctrl Pts',(6.4213824366526,-27.594680748428,8.32948279211632));
#40218=CARTESIAN_POINT('Ctrl Pts',(5.6849545944657,-27.6355180028049,8.83439047696996));
#40219=CARTESIAN_POINT('Ctrl Pts',(5.42438449889926,-27.6496644019845,8.99673352843451));
#40220=CARTESIAN_POINT('Ctrl Pts',(4.6353646234558,-27.6914035184841,9.44156226430721));
#40221=CARTESIAN_POINT('Ctrl Pts',(4.08942764429286,-27.718844201922,9.69052713554875));
#40222=CARTESIAN_POINT('Ctrl Pts',(3.08845432594339,-27.7669295098316,10.0472616435365));
#40223=CARTESIAN_POINT('Ctrl Pts',(2.64183411088289,-27.7876771652348,10.1738259242397));
#40224=CARTESIAN_POINT('Ctrl Pts',(1.83654892234962,-27.8246337000787,10.345406873886));
#40225=CARTESIAN_POINT('Ctrl Pts',(1.48117862572945,-27.8408131593276,10.4022334959532));
#40226=CARTESIAN_POINT('Ctrl Pts',(0.840717383057913,-27.8702424298845,
10.4711574645231));
#40227=CARTESIAN_POINT('Ctrl Pts',(0.556727091361961,-27.8833459232151,
10.4900904066511));
#40228=CARTESIAN_POINT('Ctrl Pts',(-0.382942286388455,-27.9266623387551,
10.5144669957549));
#40229=CARTESIAN_POINT('Ctrl Pts',(-1.03837704787873,-27.9567183264857,
10.4700752116207));
#40230=CARTESIAN_POINT('Ctrl Pts',(-2.15149850395256,-28.0077187142414,
10.2890744141875));
#40231=CARTESIAN_POINT('Ctrl Pts',(-2.61195964182773,-28.0288328340789,
10.18192853611));
#40232=CARTESIAN_POINT('Ctrl Pts',(-3.41197046532413,-28.0663896438696,
9.93791110791496));
#40233=CARTESIAN_POINT('Ctrl Pts',(-3.7545220412476,-28.0828051548399,9.81362214620951));
#40234=CARTESIAN_POINT('Ctrl Pts',(-4.38626810774778,-28.1141948299114,
9.54647441580841));
#40235=CARTESIAN_POINT('Ctrl Pts',(-4.67669008286196,-28.1290350255201,
9.40760805081518));
#40236=CARTESIAN_POINT('Ctrl Pts',(-5.45140776757648,-28.1695327478811,
8.99242144202319));
#40237=CARTESIAN_POINT('Ctrl Pts',(-5.92082141672377,-28.1950542989414,
8.69053446185361));
#40238=CARTESIAN_POINT('Ctrl Pts',(-6.72723033061127,-28.240957643741,8.07612670194272));
#40239=CARTESIAN_POINT('Ctrl Pts',(-7.07196400813563,-28.2614004113592,
7.77603890485064));
#40240=CARTESIAN_POINT('Ctrl Pts',(-7.6659279027653,-28.2989454914261,7.1867277991972));
#40241=CARTESIAN_POINT('Ctrl Pts',(-7.92103705659126,-28.316026769149,6.90454017823679));
#40242=CARTESIAN_POINT('Ctrl Pts',(-8.56357929590211,-28.3626608096505,
6.11119497484426));
#40243=CARTESIAN_POINT('Ctrl Pts',(-8.92045034996192,-28.392359382672,5.5773804859751));
#40244=CARTESIAN_POINT('Ctrl Pts',(-9.48210855297792,-28.4461840621296,
4.54393020349883));
#40245=CARTESIAN_POINT('Ctrl Pts',(-9.7014317690898,-28.4703648199866,4.05461788758502));
#40246=CARTESIAN_POINT('Ctrl Pts',(-9.99690660037589,-28.5096138125605,
3.23223990883031));
#40247=CARTESIAN_POINT('Ctrl Pts',(-10.0958687103838,-28.5247502312717,
2.9084273328655));
#40248=CARTESIAN_POINT('Ctrl Pts',(-10.2537437865664,-28.5536815988701,
2.28565133512126));
#40249=CARTESIAN_POINT('Ctrl Pts',(-10.3156242632665,-28.5674796602456,
1.9878013057817));
#40250=CARTESIAN_POINT('Ctrl Pts',(-10.4553393248025,-28.6073421346758,
1.12977722020661));
#40251=CARTESIAN_POINT('Ctrl Pts',(-10.5009905626262,-28.6334925450997,
0.565441235913797));
#40252=CARTESIAN_POINT('Ctrl Pts',(-10.5009999985369,-28.6593635075824,
0.000175291825331297));
#40253=CARTESIAN_POINT('Ctrl Pts',(-10.5009999985413,-28.6593635194262,
0.000175033045044792));
#40254=CARTESIAN_POINT('Ctrl Pts',(-10.5010159780912,-28.7032403165628,
-0.958508249417025));
#40255=CARTESIAN_POINT('Ctrl Pts',(-10.3697509234716,-28.7456685279049,
-1.91267464266642));
#40256=CARTESIAN_POINT('Ctrl Pts',(-9.94871668281961,-28.8161435099959,
-3.41388131545287));
#40257=CARTESIAN_POINT('Ctrl Pts',(-9.73728215636369,-28.8439059520432,
-3.97703908499111));
#40258=CARTESIAN_POINT('Ctrl Pts',(-9.24776380885242,-28.8962494509905,
-5.00383191503871));
#40259=CARTESIAN_POINT('Ctrl Pts',(-8.97977178860976,-28.9207477341447,
-5.47020947191444));
#40260=CARTESIAN_POINT('Ctrl Pts',(-8.31549791319486,-28.9740076374205,
-6.44485365416914));
#40261=CARTESIAN_POINT('Ctrl Pts',(-7.90578322545317,-29.0025301998082,
-6.94134107903262));
#40262=CARTESIAN_POINT('Ctrl Pts',(-7.18642390871803,-29.0487787006893,
-7.66614792613423));
#40263=CARTESIAN_POINT('Ctrl Pts',(-6.90521670990436,-29.066191591194,-7.92038370704367));
#40264=CARTESIAN_POINT('Ctrl Pts',(-6.25584606237276,-29.104700174073,-8.44655067622578));
#40265=CARTESIAN_POINT('Ctrl Pts',(-5.8823879276126,-29.1257442841134,-8.71076064571559));
#40266=CARTESIAN_POINT('Ctrl Pts',(-5.01993443084397,-29.1719225123286,
-9.24008800767182));
#40267=CARTESIAN_POINT('Ctrl Pts',(-4.52469124889504,-29.1968760850498,
-9.4924262051184));
#40268=CARTESIAN_POINT('Ctrl Pts',(-3.71268461556848,-29.2362959981014,
-9.82811025550976));
#40269=CARTESIAN_POINT('Ctrl Pts',(-3.40798994745766,-29.2507911570666,
-9.93787598289074));
#40270=CARTESIAN_POINT('Ctrl Pts',(-2.75512093712771,-29.2816760325669,
-10.1395082730866));
#40271=CARTESIAN_POINT('Ctrl Pts',(-2.406312663009,-29.298153021054,-10.2279011969941));
#40272=CARTESIAN_POINT('Ctrl Pts',(-1.58841301769394,-29.3365547874104,
-10.3910065557595));
#40273=CARTESIAN_POINT('Ctrl Pts',(-1.11739699517865,-29.3584334646503,
-10.4521532292869));
#40274=CARTESIAN_POINT('Ctrl Pts',(0.0124719635250474,-29.4101593475656,
-10.5215609332356));
#40275=CARTESIAN_POINT('Ctrl Pts',(0.671147752100753,-29.4396554426413,
-10.5001421397514));
#40276=CARTESIAN_POINT('Ctrl Pts',(1.6066009404367,-29.4819594228499,-10.3812946328334));
#40277=CARTESIAN_POINT('Ctrl Pts',(1.8881221407293,-29.4947627948844,-10.3338006686585));
#40278=CARTESIAN_POINT('Ctrl Pts',(2.50656935637032,-29.5233820560201,-10.203347342019));
#40279=CARTESIAN_POINT('Ctrl Pts',(2.84202195402001,-29.5392939080835,-10.1150424741783));
#40280=CARTESIAN_POINT('Ctrl Pts',(3.61896460480308,-29.576831635684,-9.86881276084557));
#40281=CARTESIAN_POINT('Ctrl Pts',(4.05548667073814,-29.5984218541339,-9.69759806125798));
#40282=CARTESIAN_POINT('Ctrl Pts',(5.0692057690414,-29.64961499523,-9.21953331955728));
#40283=CARTESIAN_POINT('Ctrl Pts',(5.63207864372681,-29.678870436657,-8.88686417805851));
#40284=CARTESIAN_POINT('Ctrl Pts',(6.38920730795728,-29.7208140888407,-8.33839481878914));
#40285=CARTESIAN_POINT('Ctrl Pts',(6.61119126154604,-29.7334895044116,-8.16351302791474));
#40286=CARTESIAN_POINT('Ctrl Pts',(7.10861180975288,-29.7631330276903,-7.73802899177771));
#40287=CARTESIAN_POINT('Ctrl Pts',(7.37830861116425,-29.7802311437628,-7.48131007427148));
#40288=CARTESIAN_POINT('Ctrl Pts',(7.94912188714333,-29.8185291399234,-6.87701393956899));
#40289=CARTESIAN_POINT('Ctrl Pts',(8.24220991703396,-29.83967992921,-6.52287096297466));
#40290=CARTESIAN_POINT('Ctrl Pts',(8.84477725295011,-29.8866353695719,-5.68905149860153));
#40291=CARTESIAN_POINT('Ctrl Pts',(9.14027185246643,-29.9122378040575,-5.20104231234018));
#40292=CARTESIAN_POINT('Ctrl Pts',(9.53688871543161,-29.9520639329772,-4.40681239448226));
#40293=CARTESIAN_POINT('Ctrl Pts',(9.6660291135003,-29.9663156573816,-4.11583762468849));
#40294=CARTESIAN_POINT('Ctrl Pts',(10.000150471512,-30.0078459950931,-3.2601406203456));
#40295=CARTESIAN_POINT('Ctrl Pts',(10.1701629987673,-30.0356121576088,-2.68314482244037));
#40296=CARTESIAN_POINT('Ctrl Pts',(10.3967615251233,-30.0878785218362,-1.57006935790534));
#40297=CARTESIAN_POINT('Ctrl Pts',(10.4632942658359,-30.1123015279016,-1.03791360590769));
#40298=CARTESIAN_POINT('Ctrl Pts',(10.5196374656649,-30.1654127494571,0.136998416030386));
#40299=CARTESIAN_POINT('Ctrl Pts',(10.4916887195404,-30.1938636642477,0.778453020532126));
#40300=CARTESIAN_POINT('Ctrl Pts',(10.3906475481905,-30.2278632658661,1.52234894139183));
#40301=CARTESIAN_POINT('Ctrl Pts',(10.3741317555963,-30.2328634974621,1.63109944135982));
#40302=CARTESIAN_POINT('Ctrl Pts',(10.355914067582,-30.237883364692,1.73955305318817));
#40303=CARTESIAN_POINT('Ctrl Pts',(10.3559140644695,-29.4200231052784,1.73955307171784));
#40304=CARTESIAN_POINT('Ctrl Pts',(10.3882514180482,-29.4111249843691,1.54704221351056));
#40305=CARTESIAN_POINT('Ctrl Pts',(10.4152294293614,-29.4022599014847,1.35357803988769));
#40306=CARTESIAN_POINT('Ctrl Pts',(10.4886797662756,-29.3721694805024,0.692376564764958));
#40307=CARTESIAN_POINT('Ctrl Pts',(10.5091543523562,-29.3511563112863,0.222412656287216));
#40308=CARTESIAN_POINT('Ctrl Pts',(10.4901081552782,-29.3148513170984,-0.585977830036988));
#40309=CARTESIAN_POINT('Ctrl Pts',(10.4657500100927,-29.2996015140767,-0.92401988760244));
#40310=CARTESIAN_POINT('Ctrl Pts',(10.3913488019059,-29.2712846666844,-1.5394619260401));
#40311=CARTESIAN_POINT('Ctrl Pts',(10.3464009860695,-29.2583356301667,-1.81715629619735));
#40312=CARTESIAN_POINT('Ctrl Pts',(10.1604649521611,-29.2153416361916,-2.73144948308473));
#40313=CARTESIAN_POINT('Ctrl Pts',(9.97137368277822,-29.1854419308269,-3.35672624592777));
#40314=CARTESIAN_POINT('Ctrl Pts',(9.54949020362022,-29.1348354722116,-4.39273379916829));
#40315=CARTESIAN_POINT('Ctrl Pts',(9.34482163715318,-29.1139560856025,-4.81281480532517));
#40316=CARTESIAN_POINT('Ctrl Pts',(8.92613363013922,-29.0761303892706,-5.54404122658911));
#40317=CARTESIAN_POINT('Ctrl Pts',(8.72201361298073,-29.0592038169332,-5.85992567880135));
#40318=CARTESIAN_POINT('Ctrl Pts',(8.31558950328292,-29.0275252066659,-6.42044893060744));
#40319=CARTESIAN_POINT('Ctrl Pts',(8.11829189113292,-29.0129279808966,-6.66817273704267));
#40320=CARTESIAN_POINT('Ctrl Pts',(7.53289270146217,-28.9719163864058,-7.33862828664863));
#40321=CARTESIAN_POINT('Ctrl Pts',(7.12090889826163,-28.9456457421507,-7.73903235280617));
#40322=CARTESIAN_POINT('Ctrl Pts',(6.32352711747758,-28.8988747719585,-8.39614989545271));
#40323=CARTESIAN_POINT('Ctrl Pts',(5.94995049114923,-28.8782980508495,-8.66489599617427));
#40324=CARTESIAN_POINT('Ctrl Pts',(5.2455679906524,-28.8410353906503,-9.10452461256085));
#40325=CARTESIAN_POINT('Ctrl Pts',(4.92101182835862,-28.8243737855605,-9.28396417582404));
#40326=CARTESIAN_POINT('Ctrl Pts',(4.33336691403082,-28.7945305032247,-9.56936996621308));
#40327=CARTESIAN_POINT('Ctrl Pts',(4.07420699020443,-28.7815121233764,-9.68254848627957));
#40328=CARTESIAN_POINT('Ctrl Pts',(3.20264201786614,-28.7384108117789,-10.0219776853919));
#40329=CARTESIAN_POINT('Ctrl Pts',(2.57371132311182,-28.708477663395,-10.2016176558485));
#40330=CARTESIAN_POINT('Ctrl Pts',(1.47146700095473,-28.6577525681425,-10.4079524862632));
#40331=CARTESIAN_POINT('Ctrl Pts',(1.00550151449754,-28.6367897308613,-10.4632528868755));
#40332=CARTESIAN_POINT('Ctrl Pts',(0.196484823715644,-28.6004210999217,
-10.5047096051332));
#40333=CARTESIAN_POINT('Ctrl Pts',(-0.145070787774148,-28.5850553676004,
-10.5055452732831));
#40334=CARTESIAN_POINT('Ctrl Pts',(-1.12856998013108,-28.5400847485141,
-10.4599728064761));
#40335=CARTESIAN_POINT('Ctrl Pts',(-1.76698463185707,-28.5102728697013,
-10.3712332939238));
#40336=CARTESIAN_POINT('Ctrl Pts',(-2.91596786470437,-28.4562759682354,
-10.102292907271));
#40337=CARTESIAN_POINT('Ctrl Pts',(-3.42852853124,-28.4320347323068,-9.94004039345127));
#40338=CARTESIAN_POINT('Ctrl Pts',(-4.47456880458602,-28.3813798654914,
-9.51832511460139));
#40339=CARTESIAN_POINT('Ctrl Pts',(-5.0030487517424,-28.3550454604031,-9.25147415733906));
#40340=CARTESIAN_POINT('Ctrl Pts',(-5.76934019186021,-28.3138825271998,
-8.77958769831603));
#40341=CARTESIAN_POINT('Ctrl Pts',(-6.02512532155903,-28.2996390276929,
-8.60606232902924));
#40342=CARTESIAN_POINT('Ctrl Pts',(-6.75167554736299,-28.2578921707579,
-8.06488101360722));
#40343=CARTESIAN_POINT('Ctrl Pts',(-7.19919120879324,-28.2305424207394,
-7.66805748587392));
#40344=CARTESIAN_POINT('Ctrl Pts',(-7.93065471190074,-28.1825071544331,
-6.89866199727752));
#40345=CARTESIAN_POINT('Ctrl Pts',(-8.22805239524048,-28.1617223235682,
-6.5410992917377));
#40346=CARTESIAN_POINT('Ctrl Pts',(-8.71064440030622,-28.1248251234706,
-5.87566485854064));
#40347=CARTESIAN_POINT('Ctrl Pts',(-8.9055762136924,-28.1087433876614,-5.57579341790175));
#40348=CARTESIAN_POINT('Ctrl Pts',(-9.40599703178863,-28.0631569431029,
-4.71256572311404));
#40349=CARTESIAN_POINT('Ctrl Pts',(-9.67580842618505,-28.0334795771426,
-4.13035115468015));
#40350=CARTESIAN_POINT('Ctrl Pts',(-10.0716088133229,-27.9795617196811,
-3.02045273726026));
#40351=CARTESIAN_POINT('Ctrl Pts',(-10.2131095201338,-27.9552704449761,
-2.50057056438467));
#40352=CARTESIAN_POINT('Ctrl Pts',(-10.4245064791403,-27.9047175492257,
-1.39497431273176));
#40353=CARTESIAN_POINT('Ctrl Pts',(-10.4862215696626,-27.8785315067934,
-0.809591135208093));
#40354=CARTESIAN_POINT('Ctrl Pts',(-10.5051552217517,-27.8375911542391,
0.0853302118330865));
#40355=CARTESIAN_POINT('Ctrl Pts',(-10.4981514607938,-27.823414124343,0.392913377762777));
#40356=CARTESIAN_POINT('Ctrl Pts',(-10.4377355873879,-27.7816344134869,
1.29755611611818));
#40357=CARTESIAN_POINT('Ctrl Pts',(-10.3467201052374,-27.7541850038887,
1.8908703384309));
#40358=CARTESIAN_POINT('Ctrl Pts',(-10.0962332646097,-27.7060610410738,
2.92450402369313));
#40359=CARTESIAN_POINT('Ctrl Pts',(-9.95704563782578,-27.6852841319234,
3.36807018280015));
#40360=CARTESIAN_POINT('Ctrl Pts',(-9.65940668052789,-27.6483744816745,
4.13460533706184));
#40361=CARTESIAN_POINT('Ctrl Pts',(-9.51288954591326,-27.6322721124704,
4.46139302570563));
#40362=CARTESIAN_POINT('Ctrl Pts',(-9.05844385609214,-27.5866607065496,
5.35030438420042));
#40363=CARTESIAN_POINT('Ctrl Pts',(-8.71535936462651,-27.556979428553,5.89268077780341));
#40364=CARTESIAN_POINT('Ctrl Pts',(-7.99709418191676,-27.5030579396915,
6.82692606138143));
#40365=CARTESIAN_POINT('Ctrl Pts',(-7.63688993954271,-27.4787668262038,
7.22761144806861));
#40366=CARTESIAN_POINT('Ctrl Pts',(-6.82233854457238,-27.4282136065641,
8.00449861949725));
#40367=CARTESIAN_POINT('Ctrl Pts',(-6.36383370309586,-27.4020270905609,
8.37364400443418));
#40368=CARTESIAN_POINT('Ctrl Pts',(-5.62200618322968,-27.3610860287691,
8.87460515951703));
#40369=CARTESIAN_POINT('Ctrl Pts',(-5.35971855129559,-27.3469087878769,
9.03542942258841));
#40370=CARTESIAN_POINT('Ctrl Pts',(-4.56672153109829,-27.3051288115258,
9.47496870904137));
#40371=CARTESIAN_POINT('Ctrl Pts',(-4.01877905382267,-27.2776793556659,
9.72005267491154));
#40372=CARTESIAN_POINT('Ctrl Pts',(-3.01436264259617,-27.2295551453468,
10.069770207401));
#40373=CARTESIAN_POINT('Ctrl Pts',(-2.56615374137642,-27.2087780398319,
10.1932092011323));
#40374=CARTESIAN_POINT('Ctrl Pts',(-1.76065882230906,-27.1718686995197,
10.3585313093272));
#40375=CARTESIAN_POINT('Ctrl Pts',(-1.40663220683728,-27.155766843081,10.412515197553));
#40376=CARTESIAN_POINT('Ctrl Pts',(-0.413356374842349,-27.1101580262109,
10.5123851134107));
#40377=CARTESIAN_POINT('Ctrl Pts',(0.228351446452501,-27.0804788532733,
10.5180308699488));
#40378=CARTESIAN_POINT('Ctrl Pts',(1.40268231402333,-27.0265613658597,10.4207902608575));
#40379=CARTESIAN_POINT('Ctrl Pts',(1.93459759480564,-27.0022721538639,10.3352668020732));
#40380=CARTESIAN_POINT('Ctrl Pts',(3.02904937430544,-26.9517151118528,10.0718077381626));
#40381=CARTESIAN_POINT('Ctrl Pts',(3.58790235402662,-26.92552300815,9.88652617813119));
#40382=CARTESIAN_POINT('Ctrl Pts',(4.41112952875803,-26.8845735774232,9.53454453000986));
#40383=CARTESIAN_POINT('Ctrl Pts',(4.68848734744332,-26.8703938464143,9.40125986480505));
#40384=CARTESIAN_POINT('Ctrl Pts',(5.48771639964782,-26.8286107509462,8.97301308299686));
#40385=CARTESIAN_POINT('Ctrl Pts',(5.99066492886825,-26.801160763006,8.64534327207123));
#40386=CARTESIAN_POINT('Ctrl Pts',(6.82898261893844,-26.7530336505182,7.99072591469196));
#40387=CARTESIAN_POINT('Ctrl Pts',(7.17567339136795,-26.7322542327136,7.68091272566604));
#40388=CARTESIAN_POINT('Ctrl Pts',(7.75109503258679,-26.6953485369991,7.09362517231805));
#40389=CARTESIAN_POINT('Ctrl Pts',(7.98824421975867,-26.6792527136377,6.82546284931496));
#40390=CARTESIAN_POINT('Ctrl Pts',(8.61063702296856,-26.6336350177861,6.04470486401708));
#40391=CARTESIAN_POINT('Ctrl Pts',(8.96333652530217,-26.6039404892241,5.50818833421027));
#40392=CARTESIAN_POINT('Ctrl Pts',(9.51831946706771,-26.549991857334,4.46792743750132));
#40393=CARTESIAN_POINT('Ctrl Pts',(9.73481368309964,-26.5256868761265,3.97419224801561));
#40394=CARTESIAN_POINT('Ctrl Pts',(10.1061475258653,-26.4751614096877,2.91221475488355));
#40395=CARTESIAN_POINT('Ctrl Pts',(10.2530385291071,-26.4490155272709,2.3431614259462));
#40396=CARTESIAN_POINT('Ctrl Pts',(10.3530739892064,-26.4217918282755,1.75639771377517));
#40397=CARTESIAN_POINT('Ctrl Pts',(10.3544991746734,-26.4214010862009,1.74797619914241));
#40398=CARTESIAN_POINT('Ctrl Pts',(10.3559140653568,-26.421010256864,1.73955306643568));
#40399=CARTESIAN_POINT('Origin',(0.,-20.,0.));
#40400=CARTESIAN_POINT('',(10.3559140377345,-23.4201872127662,1.73955323087673));
#40401=CARTESIAN_POINT('',(10.3559140709193,-24.2381415361801,1.73955303332087));
#40402=CARTESIAN_POINT('',(10.355914065439,-20.,1.73955306594593));
#40403=CARTESIAN_POINT('Ctrl Pts',(10.3559140709193,-24.2381415361801,1.73955303332087));
#40404=CARTESIAN_POINT('Ctrl Pts',(10.324487938485,-24.2466601328659,1.92663921053825));
#40405=CARTESIAN_POINT('Ctrl Pts',(10.2879944391612,-24.2551927625748,2.11285960877395));
#40406=CARTESIAN_POINT('Ctrl Pts',(10.1182336378067,-24.2902807135696,2.86979724878587));
#40407=CARTESIAN_POINT('Ctrl Pts',(9.94236392548783,-24.3173779275724,3.42983186070435));
#40408=CARTESIAN_POINT('Ctrl Pts',(9.51698971186189,-24.3691263055226,4.47078879368452));
#40409=CARTESIAN_POINT('Ctrl Pts',(9.27521321078572,-24.3936940741653,4.95292735996964));
#40410=CARTESIAN_POINT('Ctrl Pts',(8.66699740385356,-24.4469621869336,5.9636461937184));
#40411=CARTESIAN_POINT('Ctrl Pts',(8.2868841451409,-24.4754272278359,6.48146988670358));
#40412=CARTESIAN_POINT('Ctrl Pts',(7.62456677287723,-24.5206666298982,7.22946709848752));
#40413=CARTESIAN_POINT('Ctrl Pts',(7.37364549015571,-24.5371090576338,7.48522212436666));
#40414=CARTESIAN_POINT('Ctrl Pts',(6.76847199429934,-24.5749904610049,8.04203810592781));
#40415=CARTESIAN_POINT('Ctrl Pts',(6.40630343053227,-24.5963869157273,8.33341926642748));
#40416=CARTESIAN_POINT('Ctrl Pts',(5.53541274582119,-24.6449447373298,8.94366321381699));
#40417=CARTESIAN_POINT('Ctrl Pts',(5.01626121662686,-24.6718579121132,9.24483912236207));
#40418=CARTESIAN_POINT('Ctrl Pts',(4.19608292035302,-24.712526852402,9.63111810984119));
#40419=CARTESIAN_POINT('Ctrl Pts',(3.91228822633343,-24.7263059673185,9.74984846907212));
#40420=CARTESIAN_POINT('Ctrl Pts',(3.07224379358609,-24.7667880875886,10.058704051096));
#40421=CARTESIAN_POINT('Ctrl Pts',(2.50476368166444,-24.7939577084118,10.2148091789403));
#40422=CARTESIAN_POINT('Ctrl Pts',(1.39835422386016,-24.8457516018512,10.4213756409963));
#40423=CARTESIAN_POINT('Ctrl Pts',(0.862657737827972,-24.8702937958779,
10.4793277585888));
#40424=CARTESIAN_POINT('Ctrl Pts',(-0.315682587887609,-24.9235290904774,
10.5158001253286));
#40425=CARTESIAN_POINT('Ctrl Pts',(-0.956700476789631,-24.9519867382644,
10.4769467269681));
#40426=CARTESIAN_POINT('Ctrl Pts',(-1.94608698095275,-24.9973108142846,
10.3253767058593));
#40427=CARTESIAN_POINT('Ctrl Pts',(-2.2989640436574,-25.0138473733298,10.2525805469767));
#40428=CARTESIAN_POINT('Ctrl Pts',(-3.09595440814296,-25.0517865568668,
10.0449455584571));
#40429=CARTESIAN_POINT('Ctrl Pts',(-3.53629243011848,-25.0731455955327,
9.89851055047748));
#40430=CARTESIAN_POINT('Ctrl Pts',(-4.51998909658421,-25.1216522668389,
9.49732996439393));
#40431=CARTESIAN_POINT('Ctrl Pts',(-5.05411063215014,-25.1485513465259,
9.22418367733075));
#40432=CARTESIAN_POINT('Ctrl Pts',(-5.82221778999046,-25.1891743890039,
8.74453365071616));
#40433=CARTESIAN_POINT('Ctrl Pts',(-6.07514792543899,-25.2029204880705,
8.5707445924514));
#40434=CARTESIAN_POINT('Ctrl Pts',(-6.78788954817592,-25.2432891502633,
8.0335959312419));
#40435=CARTESIAN_POINT('Ctrl Pts',(-7.22534305985099,-25.2703752097324,
7.64254438229231));
#40436=CARTESIAN_POINT('Ctrl Pts',(-7.99808801740006,-25.3221165935984,
6.82581303906658));
#40437=CARTESIAN_POINT('Ctrl Pts',(-8.33763701369675,-25.3466883205253,
6.40663472829547));
#40438=CARTESIAN_POINT('Ctrl Pts',(-9.00747178856978,-25.3999537393579,
5.43573215714895));
#40439=CARTESIAN_POINT('Ctrl Pts',(-9.32235157281206,-25.4284124736759,
4.87601006088883));
#40440=CARTESIAN_POINT('Ctrl Pts',(-9.73005546617197,-25.473589476729,3.96539573671134));
#40441=CARTESIAN_POINT('Ctrl Pts',(-9.85917630460047,-25.4899749751795,
3.63248819485952));
#40442=CARTESIAN_POINT('Ctrl Pts',(-10.1168812261931,-25.5278217961119,
2.85232379282939));
#40443=CARTESIAN_POINT('Ctrl Pts',(-10.2332049247408,-25.5492412627006,
2.40178350380998));
#40444=CARTESIAN_POINT('Ctrl Pts',(-10.4401845279722,-25.6002691438484,
1.30365312682006));
#40445=CARTESIAN_POINT('Ctrl Pts',(-10.5010165906538,-25.6295253206722,
0.652408809668201));
#40446=CARTESIAN_POINT('Ctrl Pts',(-10.500989925391,-25.6765803594897,-0.396387287871056));
#40447=CARTESIAN_POINT('Ctrl Pts',(-10.4785667799993,-25.694365129117,-0.792178141498095));
#40448=CARTESIAN_POINT('Ctrl Pts',(-10.3613394950743,-25.7417835205261,
-1.82369462712537));
#40449=CARTESIAN_POINT('Ctrl Pts',(-10.2304880564737,-25.7715417106329,
-2.45363924603205));
#40450=CARTESIAN_POINT('Ctrl Pts',(-9.88647827046607,-25.8254287562713,
-3.5798520113043));
#40451=CARTESIAN_POINT('Ctrl Pts',(-9.69108059040702,-25.8496138822996,
-4.07931002618793));
#40452=CARTESIAN_POINT('Ctrl Pts',(-9.19762431485055,-25.9006343639578,
-5.10246730907822));
#40453=CARTESIAN_POINT('Ctrl Pts',(-8.89092518171722,-25.9273856157321,
-5.61986717440523));
#40454=CARTESIAN_POINT('Ctrl Pts',(-8.35661210688886,-25.969416823983,-6.36704628567195));
#40455=CARTESIAN_POINT('Ctrl Pts',(-8.15986176121085,-25.984091212231,-6.61731803590292));
#40456=CARTESIAN_POINT('Ctrl Pts',(-7.58007650684482,-26.0249950507928,
-7.28956992978709));
#40457=CARTESIAN_POINT('Ctrl Pts',(-7.1736182037361,-26.051082152157,-7.68990368212843));
#40458=CARTESIAN_POINT('Ctrl Pts',(-6.38444491515332,-26.0976523350784,
-8.34989403290927));
#40459=CARTESIAN_POINT('Ctrl Pts',(-6.01324674143197,-26.1182076274909,
-8.62106351431982));
#40460=CARTESIAN_POINT('Ctrl Pts',(-5.31131245965022,-26.1555127252341,
-9.06638840623387));
#40461=CARTESIAN_POINT('Ctrl Pts',(-4.98677184026508,-26.1722387689039,
-9.24886704550868));
#40462=CARTESIAN_POINT('Ctrl Pts',(-4.39999243575498,-26.2021394902377,
-9.53891317575588));
#40463=CARTESIAN_POINT('Ctrl Pts',(-4.14181100974971,-26.2151485882327,
-9.65381774195569));
#40464=CARTESIAN_POINT('Ctrl Pts',(-3.27300226131473,-26.2582322453998,
-9.99920845997779));
#40465=CARTESIAN_POINT('Ctrl Pts',(-2.64552823940767,-26.2881576880921,
-10.1832182567101));
#40466=CARTESIAN_POINT('Ctrl Pts',(-1.54524586309445,-26.338861869509,-10.3972410569353));
#40467=CARTESIAN_POINT('Ctrl Pts',(-1.07998652906133,-26.3598116907492,
-10.4558136787306));
#40468=CARTESIAN_POINT('Ctrl Pts',(-0.270896018139364,-26.3961973752654,
-10.5030766931263));
#40469=CARTESIAN_POINT('Ctrl Pts',(0.071340704784431,-26.4115936761907,
-10.5063272370803));
#40470=CARTESIAN_POINT('Ctrl Pts',(1.05460639196492,-26.4565397577758,-10.4676137279418));
#40471=CARTESIAN_POINT('Ctrl Pts',(1.69241871094522,-26.4862948003017,-10.3835862733447));
#40472=CARTESIAN_POINT('Ctrl Pts',(2.84082739009004,-26.540176754067,-10.1236082251032));
#40473=CARTESIAN_POINT('Ctrl Pts',(3.35329434407156,-26.5643599008276,-9.96559988560545));
#40474=CARTESIAN_POINT('Ctrl Pts',(4.41010538544358,-26.615382302051,-9.54895493657161));
#40475=CARTESIAN_POINT('Ctrl Pts',(4.94879637738572,-26.6421373033285,-9.28121631427281));
#40476=CARTESIAN_POINT('Ctrl Pts',(5.73341078880083,-26.6841719841633,-8.80342196799812));
#40477=CARTESIAN_POINT('Ctrl Pts',(5.99750260540311,-26.6988458826237,-8.62567085850713));
#40478=CARTESIAN_POINT('Ctrl Pts',(6.71068601229851,-26.7397498535273,-8.09704254545277));
#40479=CARTESIAN_POINT('Ctrl Pts',(7.13991577908143,-26.765837578229,-7.72120680789644));
#40480=CARTESIAN_POINT('Ctrl Pts',(7.85631652329748,-26.8124082775159,-6.98284727235599));
#40481=CARTESIAN_POINT('Ctrl Pts',(8.15412139751634,-26.8329634819584,-6.63265971039695));
#40482=CARTESIAN_POINT('Ctrl Pts',(8.65000251261382,-26.8702687561498,-5.96547565715465));
#40483=CARTESIAN_POINT('Ctrl Pts',(8.85592167238629,-26.8869950665565,-5.65527106798478));
#40484=CARTESIAN_POINT('Ctrl Pts',(9.18845369441323,-26.9168960266871,-5.09147486122319));
#40485=CARTESIAN_POINT('Ctrl Pts',(9.32208504064439,-26.9299050872885,-4.84247100950633));
#40486=CARTESIAN_POINT('Ctrl Pts',(9.73060653772764,-26.9729886756051,-4.0015008607191));
#40487=CARTESIAN_POINT('Ctrl Pts',(9.96038934011534,-27.0029140894856,-3.3893062747658));
#40488=CARTESIAN_POINT('Ctrl Pts',(10.2549714620511,-27.0536181901952,-2.30780535843868));
#40489=CARTESIAN_POINT('Ctrl Pts',(10.3476959451791,-27.0745679603403,-1.84813368023866));
#40490=CARTESIAN_POINT('Ctrl Pts',(10.4544987947741,-27.1109537124791,-1.04473034767586));
#40491=CARTESIAN_POINT('Ctrl Pts',(10.4829796544845,-27.1263501340767,-0.703662523753121));
#40492=CARTESIAN_POINT('Ctrl Pts',(10.5044217982251,-27.1547753299759,-0.0817046725738455));
#40493=CARTESIAN_POINT('Ctrl Pts',(10.5028605497905,-27.1676811210334,0.198672253356716));
#40494=CARTESIAN_POINT('Ctrl Pts',(10.4707928935629,-27.200100246433,0.901470012425277));
#40495=CARTESIAN_POINT('Ctrl Pts',(10.4259632367834,-27.2195749503812,1.3225360568573));
#40496=CARTESIAN_POINT('Ctrl Pts',(10.3559140724569,-27.2388808356861,1.73955302416723));
#40497=CARTESIAN_POINT('Ctrl Pts',(10.3559140653568,-26.421010256864,1.73955306643568));
#40498=CARTESIAN_POINT('Ctrl Pts',(10.4053763093799,-26.4073475080301,1.44509424338123));
#40499=CARTESIAN_POINT('Ctrl Pts',(10.4422574745547,-26.3935825359074,1.14865779515576));
#40500=CARTESIAN_POINT('Ctrl Pts',(10.5150042598825,-26.3522195855432,0.253998944556693));
#40501=CARTESIAN_POINT('Ctrl Pts',(10.5123763900469,-26.3247747687406,-0.346127364410621));
#40502=CARTESIAN_POINT('Ctrl Pts',(10.4169392019792,-26.2766726747831,-1.40487089015339));
#40503=CARTESIAN_POINT('Ctrl Pts',(10.3447016192798,-26.2559126398823,-1.86371609433252));
#40504=CARTESIAN_POINT('Ctrl Pts',(10.1631875152453,-26.2189761033502,-2.66635328187233));
#40505=CARTESIAN_POINT('Ctrl Pts',(10.0661264941496,-26.2028294217224,-3.01212785376631));
#40506=CARTESIAN_POINT('Ctrl Pts',(9.86067987055812,-26.1734270709244,-3.62201909199679));
#40507=CARTESIAN_POINT('Ctrl Pts',(9.7588780768272,-26.1603165689332,-3.88797195504891));
#40508=CARTESIAN_POINT('Ctrl Pts',(9.38725267733539,-26.1169778131602,-4.7519034130016));
#40509=CARTESIAN_POINT('Ctrl Pts',(9.07223249432078,-26.0869071754513,-5.32876508686101));
#40510=CARTESIAN_POINT('Ctrl Pts',(8.44117890084041,-26.0358766706685,-6.26425055801145));
#40511=CARTESIAN_POINT('Ctrl Pts',(8.15075011012007,-26.0147471347025,-6.63774153321893));
#40512=CARTESIAN_POINT('Ctrl Pts',(7.59423778360497,-25.9772077629551,-7.26158509250741));
#40513=CARTESIAN_POINT('Ctrl Pts',(7.33841597607909,-25.9608256695678,-7.52002076294703));
#40514=CARTESIAN_POINT('Ctrl Pts',(6.83157823214244,-25.9294566036194,-7.98149458489889));
#40515=CARTESIAN_POINT('Ctrl Pts',(6.58360070608352,-25.9146022781673,-8.18724107263935));
#40516=CARTESIAN_POINT('Ctrl Pts',(5.88210965424615,-25.8741070383352,-8.71675867788197));
#40517=CARTESIAN_POINT('Ctrl Pts',(5.41166455579838,-25.848602124492,-9.01637443596638));
#40518=CARTESIAN_POINT('Ctrl Pts',(4.51626111574609,-25.8027121228259,-9.49120096410001));
#40519=CARTESIAN_POINT('Ctrl Pts',(4.09932026913625,-25.782266567676,-9.67858920945322));
#40520=CARTESIAN_POINT('Ctrl Pts',(3.31555205797358,-25.7447277412708,-9.97108141040827));
#40521=CARTESIAN_POINT('Ctrl Pts',(2.95266192269231,-25.7276555657732,-10.0844996688866));
#40522=CARTESIAN_POINT('Ctrl Pts',(1.96335650260526,-25.6810310275951,-10.3357061868763));
#40523=CARTESIAN_POINT('Ctrl Pts',(1.32915926414281,-25.6513325826279,-10.4362320760073));
#40524=CARTESIAN_POINT('Ctrl Pts',(0.155471184914087,-25.5975072837113,
-10.51349280556));
#40525=CARTESIAN_POINT('Ctrl Pts',(-0.380732389865649,-25.57332580318,-10.5077478743005));
#40526=CARTESIAN_POINT('Ctrl Pts',(-1.51243151051676,-25.5223017337623,
-10.4088524806023));
#40527=CARTESIAN_POINT('Ctrl Pts',(-2.105094063499,-25.4955435251842,-10.3053495809229));
#40528=CARTESIAN_POINT('Ctrl Pts',(-2.99324982973951,-25.4535058446851,
-10.0703866737259));
#40529=CARTESIAN_POINT('Ctrl Pts',(-3.29697789022645,-25.4388323356821,
-9.97507727961022));
#40530=CARTESIAN_POINT('Ctrl Pts',(-4.1310470222125,-25.3979282388972,-9.67108410550937));
#40531=CARTESIAN_POINT('Ctrl Pts',(-4.64944294220166,-25.3718399981342,
-9.4328216758454));
#40532=CARTESIAN_POINT('Ctrl Pts',(-5.54624320751089,-25.3252688460578,
-8.92866454615409));
#40533=CARTESIAN_POINT('Ctrl Pts',(-5.93133526126242,-25.3047136898339,
-8.67762246063726));
#40534=CARTESIAN_POINT('Ctrl Pts',(-6.59647417843472,-25.2674082686937,
-8.17899596633479));
#40535=CARTESIAN_POINT('Ctrl Pts',(-6.8821083588964,-25.2506817614338,-7.94015285595226));
#40536=CARTESIAN_POINT('Ctrl Pts',(-7.3612417254224,-25.2207805952289,-7.49419227461852));
#40537=CARTESIAN_POINT('Ctrl Pts',(-7.56016532418387,-25.2077715320452,
-7.29346935868841));
#40538=CARTESIAN_POINT('Ctrl Pts',(-8.19096809570171,-25.164687907134,-6.60338968624071));
#40539=CARTESIAN_POINT('Ctrl Pts',(-8.58535441284443,-25.1347624597448,
-6.08181250940848));
#40540=CARTESIAN_POINT('Ctrl Pts',(-9.17532162892297,-25.0840582931718,
-5.12873073611511));
#40541=CARTESIAN_POINT('Ctrl Pts',(-9.39493501539029,-25.0631084905745,
-4.71440412229259));
#40542=CARTESIAN_POINT('Ctrl Pts',(-9.72579195387837,-25.0267227414275,
-3.97454108686022));
#40543=CARTESIAN_POINT('Ctrl Pts',(-9.85008604033848,-25.0113263559998,
-3.65565422511408));
#40544=CARTESIAN_POINT('Ctrl Pts',(-10.0475090082611,-24.9829011584856,
-3.06547160656759));
#40545=CARTESIAN_POINT('Ctrl Pts',(-10.1257431666508,-24.9699953280803,
-2.79622534657591));
#40546=CARTESIAN_POINT('Ctrl Pts',(-10.3498013354513,-24.9270425516554,
-1.89143472476857));
#40547=CARTESIAN_POINT('Ctrl Pts',(-10.4472378754441,-24.8971384918907,
-1.24546120469556));
#40548=CARTESIAN_POINT('Ctrl Pts',(-10.5105315661798,-24.8465673575754,
-0.129494179720476));
#40549=CARTESIAN_POINT('Ctrl Pts',(-10.5059298138899,-24.8257262199787,
0.336876526799625));
#40550=CARTESIAN_POINT('Ctrl Pts',(-10.4433458394034,-24.7889144151198,
1.15454288161165));
#40551=CARTESIAN_POINT('Ctrl Pts',(-10.3984689036257,-24.7729762833458,
1.50608188596581));
#40552=CARTESIAN_POINT('Ctrl Pts',(-10.2227949989665,-24.7275317307321,
2.4850893482032));
#40553=CARTESIAN_POINT('Ctrl Pts',(-10.0522379450659,-24.6978492270761,
3.10382547311552));
#40554=CARTESIAN_POINT('Ctrl Pts',(-9.63637208949906,-24.6438914559049,
4.20732917911189));
#40555=CARTESIAN_POINT('Ctrl Pts',(-9.40784979141307,-24.6195662675661,
4.69613336652643));
#40556=CARTESIAN_POINT('Ctrl Pts',(-8.85489998518067,-24.5690808561733,
5.67489077709454));
#40557=CARTESIAN_POINT('Ctrl Pts',(-8.5248765942037,-24.5429938150063,6.15955437490175));
#40558=CARTESIAN_POINT('Ctrl Pts',(-7.96308858724984,-24.5022015509437,
6.85231412771111));
#40559=CARTESIAN_POINT('Ctrl Pts',(-7.7596548887701,-24.488068459494,7.08186008694194));
#40560=CARTESIAN_POINT('Ctrl Pts',(-7.13008574280455,-24.446348251407,7.73249176946044));
#40561=CARTESIAN_POINT('Ctrl Pts',(-6.67764566236236,-24.4189126050422,
8.12641565994594));
#40562=CARTESIAN_POINT('Ctrl Pts',(-5.81990455958426,-24.3708457351095,
8.75296769942309));
#40563=CARTESIAN_POINT('Ctrl Pts',(-5.42802938843548,-24.3501112091167,
9.00123515811852));
#40564=CARTESIAN_POINT('Ctrl Pts',(-4.70445600895737,-24.313133073147,9.39515960325234));
#40565=CARTESIAN_POINT('Ctrl Pts',(-4.37921949755164,-24.2969184627326,
9.55109226122527));
#40566=CARTESIAN_POINT('Ctrl Pts',(-3.45484554077471,-24.2511530434077,
9.93711692767386));
#40567=CARTESIAN_POINT('Ctrl Pts',(-2.84168985470582,-24.2214319510062,
10.1295144453064));
#40568=CARTESIAN_POINT('Ctrl Pts',(-1.68852707966416,-24.167453513004,10.3783310276351));
#40569=CARTESIAN_POINT('Ctrl Pts',(-1.15427463222685,-24.1431446261589,
10.4512462941115));
#40570=CARTESIAN_POINT('Ctrl Pts',(-0.0313600116869125,-24.0926269555234,
10.5173154052712));
#40571=CARTESIAN_POINT('Ctrl Pts',(0.555901389045456,-24.0664924976876,
10.5026602528213));
#40572=CARTESIAN_POINT('Ctrl Pts',(1.44408451207068,-24.0256293279911,10.4057621242859));
#40573=CARTESIAN_POINT('Ctrl Pts',(1.74768954867303,-24.0114752109939,10.3590947597181));
#40574=CARTESIAN_POINT('Ctrl Pts',(2.63628317027525,-23.9697254489966,10.1823275246356));
#40575=CARTESIAN_POINT('Ctrl Pts',(3.21269362732594,-23.9422821578989,10.0154088227914));
#40576=CARTESIAN_POINT('Ctrl Pts',(4.20465038560577,-23.8941865287022,9.63364391806447));
#40577=CARTESIAN_POINT('Ctrl Pts',(4.62605489440489,-23.873431323799,9.43852747246173));
#40578=CARTESIAN_POINT('Ctrl Pts',(5.34843304860398,-23.8364869856283,9.04401972794437));
#40579=CARTESIAN_POINT('Ctrl Pts',(5.65463777661911,-23.8203275156975,8.8557945456203));
#40580=CARTESIAN_POINT('Ctrl Pts',(6.18508999708405,-23.7909147123274,8.49097506618665));
#40581=CARTESIAN_POINT('Ctrl Pts',(6.41292653670309,-23.7778069954154,8.32023836861591));
#40582=CARTESIAN_POINT('Ctrl Pts',(7.14183446102848,-23.7344772695802,7.72626177473927));
#40583=CARTESIAN_POINT('Ctrl Pts',(7.61022803695759,-23.7044126029548,7.2653555028247));
#40584=CARTESIAN_POINT('Ctrl Pts',(8.33687987902412,-23.6533943336693,6.40239276922271));
#40585=CARTESIAN_POINT('Ctrl Pts',(8.6164470357158,-23.6322710425749,6.02088394807754));
#40586=CARTESIAN_POINT('Ctrl Pts',(9.064094517327,-23.5947246656876,5.31464763599177));
#40587=CARTESIAN_POINT('Ctrl Pts',(9.2427159250987,-23.5783290937117,4.99754809726775));
#40588=CARTESIAN_POINT('Ctrl Pts',(9.5477499637454,-23.5469517252478,4.38350415411119));
#40589=CARTESIAN_POINT('Ctrl Pts',(9.67763823138923,-23.5321031086549,4.08875946811593));
#40590=CARTESIAN_POINT('Ctrl Pts',(9.99473535962366,-23.4916068255762,3.26902449295443));
#40591=CARTESIAN_POINT('Ctrl Pts',(10.1540425457154,-23.4660951502127,2.73435576359926));
#40592=CARTESIAN_POINT('Ctrl Pts',(10.3020404719139,-23.4339572630673,2.04017106286942));
#40593=CARTESIAN_POINT('Ctrl Pts',(10.3306207529291,-23.427063885569,1.89012929749398));
#40594=CARTESIAN_POINT('Ctrl Pts',(10.3559140377345,-23.4201872127662,1.73955323087672));
#40595=CARTESIAN_POINT('Origin',(0.,-20.,0.));
#40596=CARTESIAN_POINT('',(10.3559140572458,-20.4205078998763,1.73955311472209));
#40597=CARTESIAN_POINT('',(10.355914065439,-21.2383993725198,1.73955306594593));
#40598=CARTESIAN_POINT('',(10.355914065439,-20.,1.73955306594593));
#40599=CARTESIAN_POINT('',(7.93381306740072,-20.,-6.87936125025729));
#40600=CARTESIAN_POINT('Ctrl Pts',(10.3559140572458,-20.4205078998763,1.73955311472209));
#40601=CARTESIAN_POINT('Ctrl Pts',(10.4511075586512,-20.3940337853284,1.17284680893575));
#40602=CARTESIAN_POINT('Ctrl Pts',(10.4996412156828,-20.3677228408922,0.599170819368804));
#40603=CARTESIAN_POINT('Ctrl Pts',(10.5020506634867,-20.3206270227268,-0.441750604526287));
#40604=CARTESIAN_POINT('Ctrl Pts',(10.4721013615195,-20.2997771298122,-0.907363802500196));
#40605=CARTESIAN_POINT('Ctrl Pts',(10.3687453289844,-20.2641925554499,-1.69313568641755));
#40606=CARTESIAN_POINT('Ctrl Pts',(10.3110983543044,-20.2495054010901,-2.0146550712014));
#40607=CARTESIAN_POINT('Ctrl Pts',(10.1851156530754,-20.2236232764559,-2.56754856983621));
#40608=CARTESIAN_POINT('Ctrl Pts',(10.1236181694273,-20.2125498532238,-2.80022127884439));
#40609=CARTESIAN_POINT('Ctrl Pts',(9.86137790754711,-20.170624768431,-3.67022565940672));
#40610=CARTESIAN_POINT('Ctrl Pts',(9.60796262449235,-20.1397884991224,-4.2900376910404));
#40611=CARTESIAN_POINT('Ctrl Pts',(8.92131961002248,-20.0726190186162,-5.59781065982524));
#40612=CARTESIAN_POINT('Ctrl Pts',(8.4637606257779,-20.0367812230352,-6.26818461470371));
#40613=CARTESIAN_POINT('Ctrl Pts',(7.93381306740072,-20.,-6.87936125025729));
#40614=CARTESIAN_POINT('',(-7.93387242656103,-20.0000000365693,-6.87929279207206));
#40615=CARTESIAN_POINT('Origin',(0.,-20.,0.));
#40616=CARTESIAN_POINT('Ctrl Pts',(-7.93387242656103,-20.0000000365693,
-6.87929279207206));
#40617=CARTESIAN_POINT('Ctrl Pts',(-7.76761933943708,-20.0115427600485,
-7.07103209197269));
#40618=CARTESIAN_POINT('Ctrl Pts',(-7.59438520903055,-20.0230854835278,
-7.25677295860134));
#40619=CARTESIAN_POINT('Ctrl Pts',(-7.41462834869705,-20.034628207007,-7.4360128732203));
#40620=CARTESIAN_POINT('Ctrl Pts',(-7.23490292970705,-20.0461689115439,
-7.61522143691495));
#40621=CARTESIAN_POINT('Ctrl Pts',(-7.04865725581925,-20.0577096160809,
-7.78793112142728));
#40622=CARTESIAN_POINT('Ctrl Pts',(-6.85638681915036,-20.0692503206178,
-7.95367592916516));
#40623=CARTESIAN_POINT('Ctrl Pts',(-6.66413668086264,-20.080789806779,-8.11940323888648));
#40624=CARTESIAN_POINT('Ctrl Pts',(-6.46586326115029,-20.0923292929403,
-8.27816695779237));
#40625=CARTESIAN_POINT('Ctrl Pts',(-6.26209628867734,-20.1038687791016,
-8.42954038316049));
#40626=CARTESIAN_POINT('Ctrl Pts',(-6.05831348529575,-20.1154091617798,
-8.58092556891764));
#40627=CARTESIAN_POINT('Ctrl Pts',(-5.84903649881054,-20.126949544458,-8.72491914519595));
#40628=CARTESIAN_POINT('Ctrl Pts',(-5.63482633728949,-20.1384899271363,
-8.86113610935916));
#40629=CARTESIAN_POINT('Ctrl Pts',(-5.42061577914819,-20.1500303311821,
-8.99735332573452));
#40630=CARTESIAN_POINT('Ctrl Pts',(-5.20147226469043,-20.1615707352279,
-9.12579375361984));
#40631=CARTESIAN_POINT('Ctrl Pts',(-4.97798450545638,-20.1731111392737,
-9.24611655039218));
#40632=CARTESIAN_POINT('Ctrl Pts',(-4.75444854472634,-20.1846540323361,
-9.36646529820017));
#40633=CARTESIAN_POINT('Ctrl Pts',(-4.52656671290687,-20.1961969253985,
-9.47869278418477));
#40634=CARTESIAN_POINT('Ctrl Pts',(-4.29495217795627,-20.2077398184608,
-9.58250420240288));
#40635=CARTESIAN_POINT('Ctrl Pts',(-4.17906943469033,-20.2135150264528,
-9.63444374034253));
#40636=CARTESIAN_POINT('Ctrl Pts',(-4.06225265218799,-20.2192902344447,
-9.6842772535272));
#40637=CARTESIAN_POINT('Ctrl Pts',(-3.94458058590528,-20.2250654424367,
-9.73197230787774));
#40638=CARTESIAN_POINT('Ctrl Pts',(-3.70889539637858,-20.236632597099,-9.8275006544021));
#40639=CARTESIAN_POINT('Ctrl Pts',(-3.46970190359019,-20.2481997517614,
-9.91447815568018));
#40640=CARTESIAN_POINT('Ctrl Pts',(-3.227639342775,-20.2597669064238,-9.99266457322425));
#40641=CARTESIAN_POINT('Ctrl Pts',(-2.98561909575511,-20.2713320390874,
-10.0708373233757));
#40642=CARTESIAN_POINT('Ctrl Pts',(-2.74073104518588,-20.282897171751,-10.1402219724847));
#40643=CARTESIAN_POINT('Ctrl Pts',(-2.49363094408252,-20.2944623044145,
-10.2006277117986));
#40644=CARTESIAN_POINT('Ctrl Pts',(-2.24655838679567,-20.306026147933,-10.2610267177903));
#40645=CARTESIAN_POINT('Ctrl Pts',(-1.99727454010465,-20.3175899914514,
-10.3124487466889));
#40646=CARTESIAN_POINT('Ctrl Pts',(-1.74644781609206,-20.3291538349698,
-10.3547535473167));
#40647=CARTESIAN_POINT('Ctrl Pts',(-1.49560122773008,-20.3407185942927,
-10.3970616982946));
#40648=CARTESIAN_POINT('Ctrl Pts',(-1.24321179031955,-20.3522833536156,
-10.4302511288727));
#40649=CARTESIAN_POINT('Ctrl Pts',(-0.989956899476713,-20.3638481129385,
-10.4542329387277));
#40650=CARTESIAN_POINT('Ctrl Pts',(-0.736706570407378,-20.3754126639502,
-10.4782143166084));
#40651=CARTESIAN_POINT('Ctrl Pts',(-0.482591094877707,-20.386977214962,
-10.4929883812208));
#40652=CARTESIAN_POINT('Ctrl Pts',(-0.228292540303652,-20.3985417659737,
-10.4985181581041));
#40653=CARTESIAN_POINT('Ctrl Pts',(0.0260656621990141,-20.4101090295511,
-10.5040492320444));
#40654=CARTESIAN_POINT('Ctrl Pts',(0.280606752688652,-20.4216762931284,
-10.5003316777243));
#40655=CARTESIAN_POINT('Ctrl Pts',(0.534647621022751,-20.4332435567058,
-10.4873806511128));
#40656=CARTESIAN_POINT('Ctrl Pts',(0.754810692836675,-20.4432682598111,
-10.4761567176542));
#40657=CARTESIAN_POINT('Ctrl Pts',(0.974597946320386,-20.4532929629165,
-10.4579986016713));
#40658=CARTESIAN_POINT('Ctrl Pts',(1.19356681527101,-20.4633176660218,-10.4329477741185));
#40659=CARTESIAN_POINT('Ctrl Pts',(1.44621574302689,-20.4748842896372,-10.4040438264891));
#40660=CARTESIAN_POINT('Ctrl Pts',(1.69785355141683,-20.4864509132526,-10.3659536780285));
#40661=CARTESIAN_POINT('Ctrl Pts',(1.94780404330222,-20.4980175368679,-10.3187722335991));
#40662=CARTESIAN_POINT('Ctrl Pts',(2.19771061531791,-20.5095821280624,-10.271599079623));
#40663=CARTESIAN_POINT('Ctrl Pts',(2.44593019076294,-20.5211467192569,-10.2153378699943));
#40664=CARTESIAN_POINT('Ctrl Pts',(2.69179571929448,-20.5327113104513,-10.1501348171139));
#40665=CARTESIAN_POINT('Ctrl Pts',(2.93763365212993,-20.5442746036479,-10.0849390825577));
#40666=CARTESIAN_POINT('Ctrl Pts',(3.18111779808646,-20.5558378968444,-10.0108035796106));
#40667=CARTESIAN_POINT('Ctrl Pts',(3.42159418211181,-20.567401190041,-9.92792497216506));
#40668=CARTESIAN_POINT('Ctrl Pts',(3.66208940860482,-20.5789653892765,-9.84503987078675));
#40669=CARTESIAN_POINT('Ctrl Pts',(3.89957613936932,-20.5905295885121,-9.7534103830688));
#40670=CARTESIAN_POINT('Ctrl Pts',(4.13341708260761,-20.6020937877476,-9.65328256196863));
#40671=CARTESIAN_POINT('Ctrl Pts',(4.36725372089671,-20.6136577740893,-9.55315658419485));
#40672=CARTESIAN_POINT('Ctrl Pts',(4.59744445206855,-20.6252217604311,-9.44453269662927));
#40673=CARTESIAN_POINT('Ctrl Pts',(4.82337272867542,-20.6367857467728,-9.32770478307875));
#40674=CARTESIAN_POINT('Ctrl Pts',(5.049353932526,-20.6483524421598,-9.21084950075641));
#40675=CARTESIAN_POINT('Ctrl Pts',(5.27107043963594,-20.6599191375467,-9.08578647774354));
#40676=CARTESIAN_POINT('Ctrl Pts',(5.48792973200312,-20.6714858329337,-8.95285587154156));
#40677=CARTESIAN_POINT('Ctrl Pts',(5.67594100123841,-20.6815138518248,-8.83760855278735));
#40678=CARTESIAN_POINT('Ctrl Pts',(5.86030167021098,-20.6915418707158,-8.71644839631923));
#40679=CARTESIAN_POINT('Ctrl Pts',(6.04064259344008,-20.7015698896069,-8.58962386011853));
#40680=CARTESIAN_POINT('Ctrl Pts',(6.24866971656362,-20.7131374244913,-8.44332903731897));
#40681=CARTESIAN_POINT('Ctrl Pts',(6.45141193053673,-20.7247049593757,-8.2894509307573));
#40682=CARTESIAN_POINT('Ctrl Pts',(6.64832085415769,-20.7362724942601,-8.1283965712908));
#40683=CARTESIAN_POINT('Ctrl Pts',(6.84519539190618,-20.7478380091254,-7.96737033647484));
#40684=CARTESIAN_POINT('Ctrl Pts',(7.03623845868885,-20.7594035239908,-7.79917052559365));
#40685=CARTESIAN_POINT('Ctrl Pts',(7.22093426151812,-20.7709690388561,-7.624244840693));
#40686=CARTESIAN_POINT('Ctrl Pts',(7.4056094914013,-20.7825332654588,-7.4493386404619));
#40687=CARTESIAN_POINT('Ctrl Pts',(7.58393866813121,-20.7940974920614,-7.26770825235433));
#40688=CARTESIAN_POINT('Ctrl Pts',(7.75544162581868,-20.805661718664,-7.07983941827206));
#40689=CARTESIAN_POINT('Ctrl Pts',(7.92695814427787,-20.8172268596523,-6.89195572936509));
#40690=CARTESIAN_POINT('Ctrl Pts',(8.09164717607218,-20.8287920006405,-6.69783281100001));
#40691=CARTESIAN_POINT('Ctrl Pts',(8.24906684102578,-20.8403571416288,-6.49799178610508));
#40692=CARTESIAN_POINT('Ctrl Pts',(8.40648365211932,-20.8519220729527,-6.29815438412675));
#40693=CARTESIAN_POINT('Ctrl Pts',(8.55663119010718,-20.8634870042766,-6.09259930154301));
#40694=CARTESIAN_POINT('Ctrl Pts',(8.69910868029778,-20.8750519356005,-5.88187973086563));
#40695=CARTESIAN_POINT('Ctrl Pts',(8.84161952783095,-20.8866195745477,-5.67111082576427));
#40696=CARTESIAN_POINT('Ctrl Pts',(8.97645658274871,-20.8981872134949,-5.45517524491679));
#40697=CARTESIAN_POINT('Ctrl Pts',(9.10326231471628,-20.9097548524421,-5.23465531142849));
#40698=CARTESIAN_POINT('Ctrl Pts',(9.21312918916514,-20.9197772726921,-5.04359268775918));
#40699=CARTESIAN_POINT('Ctrl Pts',(9.31696772742072,-20.929799692942,-4.84908921829048));
#40700=CARTESIAN_POINT('Ctrl Pts',(9.41457305225478,-20.939822113192,-4.65153901883646));
#40701=CARTESIAN_POINT('Ctrl Pts',(9.52721930290881,-20.9513889827819,-4.42354644443251));
#40702=CARTESIAN_POINT('Ctrl Pts',(9.63159720442441,-20.9629558523718,-4.19142462929392));
#40703=CARTESIAN_POINT('Ctrl Pts',(9.72742002242571,-20.9745227219618,-3.95579330947807));
#40704=CARTESIAN_POINT('Ctrl Pts',(9.82322603763173,-20.9860875632692,-3.72020330826367));
#40705=CARTESIAN_POINT('Ctrl Pts',(9.9104798598109,-20.9976524045767,-3.48110528720753));
#40706=CARTESIAN_POINT('Ctrl Pts',(9.98894283068408,-21.0092172458841,-3.239139102497));
#40707=CARTESIAN_POINT('Ctrl Pts',(10.0673970183146,-21.0207807926089,-2.99720000378244));
#40708=CARTESIAN_POINT('Ctrl Pts',(10.1370622341292,-21.0323443393336,-2.75239364572877));
#40709=CARTESIAN_POINT('Ctrl Pts',(10.1977493055541,-21.0439078860583,-2.50537623942399));
#40710=CARTESIAN_POINT('Ctrl Pts',(10.2584411501937,-21.0554723422896,-2.25833940448198));
#40711=CARTESIAN_POINT('Ctrl Pts',(10.3101533700907,-21.0670367985209,-2.00909144186774));
#40712=CARTESIAN_POINT('Ctrl Pts',(10.3527473408365,-21.0786012547522,-1.7583013100156));
#40713=CARTESIAN_POINT('Ctrl Pts',(10.3953405331329,-21.0901654996309,-1.50751576161611));
#40714=CARTESIAN_POINT('Ctrl Pts',(10.4288157650271,-21.1017297445096,-1.25518837362847));
#40715=CARTESIAN_POINT('Ctrl Pts',(10.4530858517841,-21.1132939893884,-1.00199659442136));
#40716=CARTESIAN_POINT('Ctrl Pts',(10.477361625521,-21.1248609440073,-0.748745487178918));
#40717=CARTESIAN_POINT('Ctrl Pts',(10.492427915911,-21.1364278986261,-0.494629859558366));
#40718=CARTESIAN_POINT('Ctrl Pts',(10.4982494496924,-21.147994853245,-0.240332045374238));
#40719=CARTESIAN_POINT('Ctrl Pts',(10.5032956851473,-21.1580213477557,-0.0199010225154512));
#40720=CARTESIAN_POINT('Ctrl Pts',(10.5013963984425,-21.1680478422664,0.200666716014797));
#40721=CARTESIAN_POINT('Ctrl Pts',(10.4925603111451,-21.1780743367771,0.420926498313265));
#40722=CARTESIAN_POINT('Ctrl Pts',(10.4823664077128,-21.1896415738773,0.675032968203946));
#40723=CARTESIAN_POINT('Ctrl Pts',(10.4629357454992,-21.2012088109776,0.928808297393872));
#40724=CARTESIAN_POINT('Ctrl Pts',(10.4343131459793,-21.2127760480778,1.18157106076805));
#40725=CARTESIAN_POINT('Ctrl Pts',(10.413178564243,-21.2213171562251,1.36820803197274));
#40726=CARTESIAN_POINT('Ctrl Pts',(10.3870334654684,-21.2298582643724,1.5542929328799));
#40727=CARTESIAN_POINT('Ctrl Pts',(10.355914065439,-21.2383993725198,1.73955306594593));
#40728=CARTESIAN_POINT('Origin',(0.,-20.,0.));
#40729=CARTESIAN_POINT('',(-10.5009999965284,-22.6589303284762,0.000270018945713324));
#40730=CARTESIAN_POINT('Ctrl Pts',(10.355914065439,-21.2383993725198,1.73955306594593));
#40731=CARTESIAN_POINT('Ctrl Pts',(10.3137801598842,-21.249963549325,1.99038479606632));
#40732=CARTESIAN_POINT('Ctrl Pts',(10.262525630829,-21.2615277261302,2.23970409686379));
#40733=CARTESIAN_POINT('Ctrl Pts',(10.2022850825147,-21.2730919029355,2.48684138921193));
#40734=CARTESIAN_POINT('Ctrl Pts',(10.1401064651179,-21.2850281243877,2.74192962422017));
#40735=CARTESIAN_POINT('Ctrl Pts',(10.0683541050816,-21.2969643458399,2.99469282093897));
#40736=CARTESIAN_POINT('Ctrl Pts',(9.98723265985342,-21.3089005672922,3.24440823540398));
#40737=CARTESIAN_POINT('Ctrl Pts',(9.90863688274792,-21.3204651615632,3.48634890842686));
#40738=CARTESIAN_POINT('Ctrl Pts',(9.8212467005171,-21.3320297558341,3.72542843874294));
#40739=CARTESIAN_POINT('Ctrl Pts',(9.72529859813282,-21.3435943501051,3.96100595520327));
#40740=CARTESIAN_POINT('Ctrl Pts',(9.62472557048125,-21.355716385148,4.20793886464386));
#40741=CARTESIAN_POINT('Ctrl Pts',(9.51474940816849,-21.3678384201908,4.45102352994098));
#40742=CARTESIAN_POINT('Ctrl Pts',(9.39569915454623,-21.3799604552337,4.68954564934165));
#40743=CARTESIAN_POINT('Ctrl Pts',(9.27664890092398,-21.3920824902765,4.92806776874232));
#40744=CARTESIAN_POINT('Ctrl Pts',(9.14852472029361,-21.4042045253194,5.16202703322294));
#40745=CARTESIAN_POINT('Ctrl Pts',(9.01171144400528,-21.4163265603622,5.3907381544631));
#40746=CARTESIAN_POINT('Ctrl Pts',(8.88116158188507,-21.4278936395697,5.60897870942459));
#40747=CARTESIAN_POINT('Ctrl Pts',(8.74265991882838,-21.4394607187771,5.82250848322716));
#40748=CARTESIAN_POINT('Ctrl Pts',(8.59657188523118,-21.4510277979846,6.03075060187808));
#40749=CARTESIAN_POINT('Ctrl Pts',(8.4505094356669,-21.4625928514783,6.2389562516062));
#40750=CARTESIAN_POINT('Ctrl Pts',(8.29686342668248,-21.4741579049721,6.44187586825201));
#40751=CARTESIAN_POINT('Ctrl Pts',(8.13604225364843,-21.4857229584658,6.63896207602118));
#40752=CARTESIAN_POINT('Ctrl Pts',(7.97523905559419,-21.4972867193337,6.83602625546821));
#40753=CARTESIAN_POINT('Ctrl Pts',(7.80726246971846,-21.5088504802016,7.02725811347665));
#40754=CARTESIAN_POINT('Ctrl Pts',(7.63256145618795,-21.5204142410695,7.21214299757805));
#40755=CARTESIAN_POINT('Ctrl Pts',(7.45784667973633,-21.5319789129288,7.39704244688444));
#40756=CARTESIAN_POINT('Ctrl Pts',(7.27640660479399,-21.5435435847882,7.57559371963092));
#40757=CARTESIAN_POINT('Ctrl Pts',(7.08872830055417,-21.5551082566475,7.74731773460482));
#40758=CARTESIAN_POINT('Ctrl Pts',(6.90105341810014,-21.5666727176576,7.9190386186745));
#40759=CARTESIAN_POINT('Ctrl Pts',(6.7071407393271,-21.5782371786677,8.08393230839117));
#40760=CARTESIAN_POINT('Ctrl Pts',(6.50751234785376,-21.5898016396778,8.24155835036863));
#40761=CARTESIAN_POINT('Ctrl Pts',(6.30783719252314,-21.6013688097154,8.39922131696226));
#40762=CARTESIAN_POINT('Ctrl Pts',(6.10244386533026,-21.612935979753,8.54961306089774));
#40763=CARTESIAN_POINT('Ctrl Pts',(5.89188669093887,-21.6245031497906,8.69233410662162));
#40764=CARTESIAN_POINT('Ctrl Pts',(5.70939778698396,-21.6345283611761,8.81602975974163));
#40765=CARTESIAN_POINT('Ctrl Pts',(5.52303059208191,-21.6445535725617,8.93396407346109));
#40766=CARTESIAN_POINT('Ctrl Pts',(5.3331633740482,-21.6545787839473,9.04590346099885));
#40767=CARTESIAN_POINT('Ctrl Pts',(5.11409401130845,-21.6661459027596,9.17505946037215));
#40768=CARTESIAN_POINT('Ctrl Pts',(4.89029674129765,-21.677713021572,9.29627375453589));
#40769=CARTESIAN_POINT('Ctrl Pts',(4.66236849914987,-21.6892801403843,9.40921468445348));
#40770=CARTESIAN_POINT('Ctrl Pts',(4.4344801664234,-21.7008452338355,9.52213583881753));
#40771=CARTESIAN_POINT('Ctrl Pts',(4.20246255342235,-21.7124103272867,9.62678639796797));
#40772=CARTESIAN_POINT('Ctrl Pts',(3.96693620500328,-21.7239754207378,9.72288116483145));
#40773=CARTESIAN_POINT('Ctrl Pts',(3.73143617643087,-21.7355392218007,9.81896519319563));
#40774=CARTESIAN_POINT('Ctrl Pts',(3.49242845155076,-21.7471030228636,9.90649523377258));
#40775=CARTESIAN_POINT('Ctrl Pts',(3.25055353409967,-21.7586668239265,9.98523423470637));
#40776=CARTESIAN_POINT('Ctrl Pts',(3.00865956023713,-21.7702315360576,10.0639794391887));
#40777=CARTESIAN_POINT('Ctrl Pts',(2.76389820463271,-21.7817962481888,10.1339321311693));
#40778=CARTESIAN_POINT('Ctrl Pts',(2.51692641074983,-21.7933609603199,10.1949047294651));
#40779=CARTESIAN_POINT('Ctrl Pts',(2.26995912005407,-21.8049254615846,10.2558762160104));
#40780=CARTESIAN_POINT('Ctrl Pts',(2.02078174091657,-21.8164899628492,10.3078678717852));
#40781=CARTESIAN_POINT('Ctrl Pts',(1.77006347660718,-21.8280544641139,10.3507427892293));
#40782=CARTESIAN_POINT('Ctrl Pts',(1.51928648744899,-21.8396216740907,10.3936277491129));
#40783=CARTESIAN_POINT('Ctrl Pts',(1.26696816464985,-21.8511888840674,10.4273916553262));
#40784=CARTESIAN_POINT('Ctrl Pts',(1.01378641150786,-21.8627560940442,10.451949010201));
#40785=CARTESIAN_POINT('Ctrl Pts',(0.794361003023756,-21.8727810652069,
10.4732321696619));
#40786=CARTESIAN_POINT('Ctrl Pts',(0.574287290355624,-21.8828060363696,
10.4876009062648));
#40787=CARTESIAN_POINT('Ctrl Pts',(0.354009164658848,-21.8928310075323,
10.4950311343672));
#40788=CARTESIAN_POINT('Ctrl Pts',(0.0998454799983954,-21.9043981279682,
10.5036043603578));
#40789=CARTESIAN_POINT('Ctrl Pts',(-0.154669164764553,-21.9159652484041,
10.5029417501122));
#40790=CARTESIAN_POINT('Ctrl Pts',(-0.408851908986821,-21.92753236884,10.4930377449296));
#40791=CARTESIAN_POINT('Ctrl Pts',(-0.662990148560078,-21.9390974639982,
10.4831354738312));
#40792=CARTESIAN_POINT('Ctrl Pts',(-0.916796327124914,-21.9506625591565,
10.4639950486802));
#40793=CARTESIAN_POINT('Ctrl Pts',(-1.16958908724468,-21.9622276543147,
10.4356630056263));
#40794=CARTESIAN_POINT('Ctrl Pts',(-1.42235359973181,-21.9737914571631,
10.4073341284589));
#40795=CARTESIAN_POINT('Ctrl Pts',(-1.67410464488521,-21.9853552600116,
10.3698157149898));
#40796=CARTESIAN_POINT('Ctrl Pts',(-1.9241663796562,-21.99691906286,10.323206127139));
#40797=CARTESIAN_POINT('Ctrl Pts',(-2.17424781820299,-22.0084837768858,
10.2765928666557));
#40798=CARTESIAN_POINT('Ctrl Pts',(-2.42263940761389,-22.0200484909115,
10.220887047828));
#40799=CARTESIAN_POINT('Ctrl Pts',(-2.66867454355026,-22.0316132049373,
10.1562383381155));
#40800=CARTESIAN_POINT('Ctrl Pts',(-2.91470519460546,-22.0431777081542,
10.0915908068597));
#40801=CARTESIAN_POINT('Ctrl Pts',(-3.15837921079943,-22.0547422113712,
10.0180007828975));
#40802=CARTESIAN_POINT('Ctrl Pts',(-3.39904347241097,-22.0663067145882,
9.93566829522103));
#40803=CARTESIAN_POINT('Ctrl Pts',(-3.6397641056346,-22.0778739265982,9.85331652252478));
#40804=CARTESIAN_POINT('Ctrl Pts',(-3.87747331294342,-22.0894411386083,
9.76221828223451));
#40805=CARTESIAN_POINT('Ctrl Pts',(-4.11153493727735,-22.1010083506183,
9.66262290786243));
#40806=CARTESIAN_POINT('Ctrl Pts',(-4.31438921697679,-22.1110333107847,
9.57630654572003));
#40807=CARTESIAN_POINT('Ctrl Pts',(-4.51450390802682,-22.1210582709511,
9.48360864941968));
#40808=CARTESIAN_POINT('Ctrl Pts',(-4.71147772092378,-22.1310832311175,
9.38472049052282));
#40809=CARTESIAN_POINT('Ctrl Pts',(-4.93875220021531,-22.1426503403095,
9.27062027338817));
#40810=CARTESIAN_POINT('Ctrl Pts',(-5.16191511449861,-22.1542174495014,
9.14824246401068));
#40811=CARTESIAN_POINT('Ctrl Pts',(-5.38036420898964,-22.1657845586934,
9.01790895821328));
#40812=CARTESIAN_POINT('Ctrl Pts',(-5.59877505233851,-22.1773496424472,
8.88759827423379));
#40813=CARTESIAN_POINT('Ctrl Pts',(-5.81247348602248,-22.1889147262009,
8.74933481654849));
#40814=CARTESIAN_POINT('Ctrl Pts',(-6.02088350472526,-22.2004798099547,
8.60348550428995));
#40815=CARTESIAN_POINT('Ctrl Pts',(-6.22927023290093,-22.2120436012711,
8.45765249118719));
#40816=CARTESIAN_POINT('Ctrl Pts',(-6.43236949941675,-22.2236073925875,
8.30423547485258));
#40817=CARTESIAN_POINT('Ctrl Pts',(-6.62963494174465,-22.2351711839039,
8.14364424193484));
#40818=CARTESIAN_POINT('Ctrl Pts',(-6.82691592579408,-22.2467358862832,
7.98304035670358));
#40819=CARTESIAN_POINT('Ctrl Pts',(-7.01836195042591,-22.2583005886625,
7.81526129764087));
#40820=CARTESIAN_POINT('Ctrl Pts',(-7.20345931715591,-22.2698652910418,
7.64075747986283));
#40821=CARTESIAN_POINT('Ctrl Pts',(-7.38855330907376,-22.2814297825661,
7.46625684374865));
#40822=CARTESIAN_POINT('Ctrl Pts',(-7.56729867441535,-22.2929942740905,
7.28503188540077));
#40823=CARTESIAN_POINT('Ctrl Pts',(-7.73921765517788,-22.3045587656148,
7.09757078765566));
#40824=CARTESIAN_POINT('Ctrl Pts',(-7.91117690526097,-22.3161259659396,
6.91006578009324));
#40825=CARTESIAN_POINT('Ctrl Pts',(-8.07630638719474,-22.3276931662644,
6.71632191726792));
#40826=CARTESIAN_POINT('Ctrl Pts',(-8.23416683158492,-22.3392603665892,
6.51686255721469));
#40827=CARTESIAN_POINT('Ctrl Pts',(-8.37098088745965,-22.3492853959603,
6.34399566749777));
#40828=CARTESIAN_POINT('Ctrl Pts',(-8.50233549758968,-22.3593104253315,
6.16683632915167));
#40829=CARTESIAN_POINT('Ctrl Pts',(-8.6279698299386,-22.3693354547026,5.98574453294403));
#40830=CARTESIAN_POINT('Ctrl Pts',(-8.7729297269788,-22.3809025733261,5.776796487913));
#40831=CARTESIAN_POINT('Ctrl Pts',(-8.91031820995912,-22.3924696919496,
5.56254773761589));
#40832=CARTESIAN_POINT('Ctrl Pts',(-9.03976050121706,-22.4040368105731,
5.343569133139));
#40833=CARTESIAN_POINT('Ctrl Pts',(-9.16918012806939,-22.4156019038781,
5.12462887022624));
#40834=CARTESIAN_POINT('Ctrl Pts',(-9.29065619986459,-22.4271669971831,
4.9009606445605));
#40835=CARTESIAN_POINT('Ctrl Pts',(-9.40385853326217,-22.4387320904881,
4.67316227905604));
#40836=CARTESIAN_POINT('Ctrl Pts',(-9.51704821682695,-22.4502958914479,
4.44538936895653));
#40837=CARTESIAN_POINT('Ctrl Pts',(-9.62196588488816,-22.4618596924076,
4.2134874883438));
#40838=CARTESIAN_POINT('Ctrl Pts',(-9.71832789633379,-22.4734234933674,
3.97807791519226));
#40839=CARTESIAN_POINT('Ctrl Pts',(-9.81469750034251,-22.484988205463,3.74264979363137));
#40840=CARTESIAN_POINT('Ctrl Pts',(-9.90250999273814,-22.4965529175587,
3.50371368221689));
#40841=CARTESIAN_POINT('Ctrl Pts',(-9.98152985600637,-22.5081176296544,
3.26191090216357));
#40842=CARTESIAN_POINT('Ctrl Pts',(-10.060548278714,-22.5196821309211,3.02011253026216));
#40843=CARTESIAN_POINT('Ctrl Pts',(-10.1307743086362,-22.5312466321879,
2.77544785797645));
#40844=CARTESIAN_POINT('Ctrl Pts',(-10.1920220597857,-22.5428111334547,
2.52857416993089));
#40845=CARTESIAN_POINT('Ctrl Pts',(-10.253284157106,-22.5543783434954,2.28164265621764));
#40846=CARTESIAN_POINT('Ctrl Pts',(-10.3055637050415,-22.5659455535361,
2.03250136123242));
#40847=CARTESIAN_POINT('Ctrl Pts',(-10.3487254459157,-22.5775127635768,
1.78182003722534));
#40848=CARTESIAN_POINT('Ctrl Pts',(-10.3861324977168,-22.5875377351471,
1.56456167176555));
#40849=CARTESIAN_POINT('Ctrl Pts',(-10.4166917642207,-22.5975627067174,
1.34614685374224));
#40850=CARTESIAN_POINT('Ctrl Pts',(-10.4403464900633,-22.6075876782877,
1.12701648941934));
#40851=CARTESIAN_POINT('Ctrl Pts',(-10.4692474892472,-22.6198360424031,
0.859286204883308));
#40852=CARTESIAN_POINT('Ctrl Pts',(-10.4878466242685,-22.6320844065186,
0.590435506072792));
#40853=CARTESIAN_POINT('Ctrl Pts',(-10.496085593371,-22.644332770634,0.32122922754471));
#40854=CARTESIAN_POINT('Ctrl Pts',(-10.4993586516315,-22.6491986232481,
0.214282858074387));
#40855=CARTESIAN_POINT('Ctrl Pts',(-10.5009972449014,-22.6540644758621,
0.107280420198263));
#40856=CARTESIAN_POINT('Ctrl Pts',(-10.5009999965284,-22.6589303284762,
0.000270018945713879));
#40857=CARTESIAN_POINT('Ctrl Pts',(-10.5009999965872,-22.6588805488861,
0.000267724969670036));
#40858=CARTESIAN_POINT('Ctrl Pts',(-10.5010126771194,-22.6818006656778,
-0.497101904332627));
#40859=CARTESIAN_POINT('Ctrl Pts',(-10.4656892092644,-22.7046448522079,
-0.993853520664748));
#40860=CARTESIAN_POINT('Ctrl Pts',(-10.3242131605364,-22.7500807458748,
-1.98339130199445));
#40861=CARTESIAN_POINT('Ctrl Pts',(-10.2175600408328,-22.7726097978088,
-2.47481233318349));
#40862=CARTESIAN_POINT('Ctrl Pts',(-9.99242656851183,-22.8084782689233,
-3.24204137223171));
#40863=CARTESIAN_POINT('Ctrl Pts',(-9.89662109300719,-22.8218100622224,
-3.52367825448765));
#40864=CARTESIAN_POINT('Ctrl Pts',(-9.57874156277706,-22.8615515930728,
-4.34236563191908));
#40865=CARTESIAN_POINT('Ctrl Pts',(-9.32392563585833,-22.888417807518,-4.86547030910378));
#40866=CARTESIAN_POINT('Ctrl Pts',(-8.75263104549614,-22.9398753912165,
-5.82676945844352));
#40867=CARTESIAN_POINT('Ctrl Pts',(-8.44302268121886,-22.9643879426073,
-6.26699164878198));
#40868=CARTESIAN_POINT('Ctrl Pts',(-7.69346093331466,-23.0175828619016,
-7.17579645049292));
#40869=CARTESIAN_POINT('Ctrl Pts',(-7.24148335360625,-23.0460297043472,
-7.63166399727421));
#40870=CARTESIAN_POINT('Ctrl Pts',(-6.47325740482191,-23.0914459140182,
-8.27642591553376));
#40871=CARTESIAN_POINT('Ctrl Pts',(-6.18385667843293,-23.108087882826,-8.49483305557552));
#40872=CARTESIAN_POINT('Ctrl Pts',(-5.50052676811626,-23.1460926230776,
-8.95707975104865));
#40873=CARTESIAN_POINT('Ctrl Pts',(-5.10057640740971,-23.1674106662637,
-9.19071286829367));
#40874=CARTESIAN_POINT('Ctrl Pts',(-4.15101812912958,-23.2158562594999,
-9.66427110769821));
#40875=CARTESIAN_POINT('Ctrl Pts',(-3.59366149896661,-23.2427350604403,
-9.88507487774687));
#40876=CARTESIAN_POINT('Ctrl Pts',(-2.72749800666996,-23.28330497042,-10.1452141221778));
#40877=CARTESIAN_POINT('Ctrl Pts',(-2.43076105389523,-23.2970169167777,
-10.2203724046451));
#40878=CARTESIAN_POINT('Ctrl Pts',(-1.55943077684954,-23.337267736517,-10.4009665326054));
#40879=CARTESIAN_POINT('Ctrl Pts',(-0.978820817213086,-23.36426686629,-10.4715709498557));
#40880=CARTESIAN_POINT('Ctrl Pts',(0.143534307043352,-23.4159539037152,
-10.5138593771421));
#40881=CARTESIAN_POINT('Ctrl Pts',(0.683221821986221,-23.4405566447055,
-10.4926199329967));
#40882=CARTESIAN_POINT('Ctrl Pts',(1.85613040415187,-23.4938839262522,-10.3555490567668));
#40883=CARTESIAN_POINT('Ctrl Pts',(2.48519125001576,-23.522372779407,-10.2228382358753));
#40884=CARTESIAN_POINT('Ctrl Pts',(3.43950857927777,-23.5675979520273,-9.92816134190129));
#40885=CARTESIAN_POINT('Ctrl Pts',(3.77521664844392,-23.5840007523882,-9.80542356509557));
#40886=CARTESIAN_POINT('Ctrl Pts',(4.53170105575867,-23.6218580551176,-9.48422827044658));
#40887=CARTESIAN_POINT('Ctrl Pts',(4.94687736646116,-23.6432704977692,-9.27444418477801));
#40888=CARTESIAN_POINT('Ctrl Pts',(5.86248228431866,-23.6918487325796,-8.73277218301214));
#40889=CARTESIAN_POINT('Ctrl Pts',(6.35111776109031,-23.7187665439782,-8.38411192777041));
#40890=CARTESIAN_POINT('Ctrl Pts',(7.04173267828325,-23.759454305756,-7.79613710549295));
#40891=CARTESIAN_POINT('Ctrl Pts',(7.2672222328201,-23.7732481327237,-7.58638453490304));
#40892=CARTESIAN_POINT('Ctrl Pts',(7.89592170235234,-23.8137806611875,-6.94777403078112));
#40893=CARTESIAN_POINT('Ctrl Pts',(8.27269706695908,-23.8409873637394,-6.49458121508277));
#40894=CARTESIAN_POINT('Ctrl Pts',(8.917404410757,-23.8928046424922,-5.57136141121609));
#40895=CARTESIAN_POINT('Ctrl Pts',(9.19096995960149,-23.9173338174171,-5.10747143168864));
#40896=CARTESIAN_POINT('Ctrl Pts',(9.70990217882667,-23.9705419353012,-4.04958052614503));
#40897=CARTESIAN_POINT('Ctrl Pts',(9.93878643732868,-23.9989857837472,-3.44989966382878));
#40898=CARTESIAN_POINT('Ctrl Pts',(10.2086722175911,-24.0442828585718,-2.48665852888054));
#40899=CARTESIAN_POINT('Ctrl Pts',(10.2878717861949,-24.0608064550266,-2.13544798836442));
#40900=CARTESIAN_POINT('Ctrl Pts',(10.4275170772288,-24.0987376386477,-1.32395296018504));
#40901=CARTESIAN_POINT('Ctrl Pts',(10.4757999960315,-24.1201017840994,-0.862315821854623));
#40902=CARTESIAN_POINT('Ctrl Pts',(10.5161713237268,-24.1686157045272,0.199424976794982));
#40903=CARTESIAN_POINT('Ctrl Pts',(10.4876938255333,-24.1955169652023,0.798704439162373));
#40904=CARTESIAN_POINT('Ctrl Pts',(10.3927673562948,-24.2276343130389,1.5083423436313));
#40905=CARTESIAN_POINT('Ctrl Pts',(10.3753053972976,-24.2328851818079,1.62411251161865));
#40906=CARTESIAN_POINT('Ctrl Pts',(10.3559140709193,-24.2381415361801,1.73955303332087));
#40907=CARTESIAN_POINT('Ctrl Pts',(10.3559140377345,-23.4201872127662,1.73955323087673));
#40908=CARTESIAN_POINT('Ctrl Pts',(10.406224139909,-23.4065090324115,1.44004696449681));
#40909=CARTESIAN_POINT('Ctrl Pts',(10.4435295861151,-23.3929004977755,1.13842662890351));
#40910=CARTESIAN_POINT('Ctrl Pts',(10.4979431611934,-23.3622138170407,0.456729939028258));
#40911=CARTESIAN_POINT('Ctrl Pts',(10.5075946919293,-23.3451379950166,0.0765682733419336));
#40912=CARTESIAN_POINT('Ctrl Pts',(10.4884876459115,-23.3149182215354,-0.584724929674124));
#40913=CARTESIAN_POINT('Ctrl Pts',(10.469039939308,-23.3019523091401,-0.865723117446026));
#40914=CARTESIAN_POINT('Ctrl Pts',(10.3672043976137,-23.2589371370392,-1.79361707290191));
#40915=CARTESIAN_POINT('Ctrl Pts',(10.2358927282489,-23.2290341433094,-2.43362470669664));
#40916=CARTESIAN_POINT('Ctrl Pts',(9.91006544442555,-23.1784062867506,-3.50426303834268));
#40917=CARTESIAN_POINT('Ctrl Pts',(9.74437407547304,-23.15750927925,-3.94162844346253));
#40918=CARTESIAN_POINT('Ctrl Pts',(9.39420562564757,-23.119704904819,-4.70749177167167));
#40919=CARTESIAN_POINT('Ctrl Pts',(9.22015573169296,-23.1028177710418,-5.03987124081586));
#40920=CARTESIAN_POINT('Ctrl Pts',(8.8668634357367,-23.0711616140692,-5.63472971615912));
#40921=CARTESIAN_POINT('Ctrl Pts',(8.69277342211163,-23.0565457790609,-5.89975711545663));
#40922=CARTESIAN_POINT('Ctrl Pts',(8.171352561563,-23.0155657991684,-6.62024886433821));
#40923=CARTESIAN_POINT('Ctrl Pts',(7.79837287523769,-22.9893449493126,-7.05578526963895));
#40924=CARTESIAN_POINT('Ctrl Pts',(7.06535612250973,-22.9426303310857,-7.78221733902895));
#40925=CARTESIAN_POINT('Ctrl Pts',(6.71807931316477,-22.9220612514924,-8.08390867161846));
#40926=CARTESIAN_POINT('Ctrl Pts',(6.05662793146166,-22.8847833951965,-8.58638445909492));
#40927=CARTESIAN_POINT('Ctrl Pts',(5.74941291497919,-22.8680987420118,-8.79505471097264));
#40928=CARTESIAN_POINT('Ctrl Pts',(5.18990797552534,-22.8382339102335,-9.13322165807456));
#40929=CARTESIAN_POINT('Ctrl Pts',(4.94222124970648,-22.8252178309031,-9.26959164122858));
#40930=CARTESIAN_POINT('Ctrl Pts',(4.10539493328197,-22.782119710391,-9.68724213096674));
#40931=CARTESIAN_POINT('Ctrl Pts',(3.49553769443001,-22.7521873090204,-9.92361748713999));
#40932=CARTESIAN_POINT('Ctrl Pts',(2.41683688012316,-22.7014650792893,-10.2298359829262));
#40933=CARTESIAN_POINT('Ctrl Pts',(1.95792627690865,-22.6805043147014,-10.3274959996256));
#40934=CARTESIAN_POINT('Ctrl Pts',(1.15602594585778,-22.6441329257167,-10.4427587646851));
#40935=CARTESIAN_POINT('Ctrl Pts',(0.815865287064391,-22.628762285365,-10.4748254059024));
#40936=CARTESIAN_POINT('Ctrl Pts',(0.194645699797482,-22.600358412073,-10.5029390869844));
#40937=CARTESIAN_POINT('Ctrl Pts',(-0.0858451102346386,-22.5874473131349,
-10.5043916746554));
#40938=CARTESIAN_POINT('Ctrl Pts',(-1.01743073845812,-22.5444929550306,
-10.4718977688152));
#40939=CARTESIAN_POINT('Ctrl Pts',(-1.6652952669242,-22.5145928138781,-10.3885821791191));
#40940=CARTESIAN_POINT('Ctrl Pts',(-2.75584752866656,-22.4640236485553,
-10.1436377018274));
#40941=CARTESIAN_POINT('Ctrl Pts',(-3.20314257028947,-22.4431807456872,
-10.01139169134));
#40942=CARTESIAN_POINT('Ctrl Pts',(-3.97228551560262,-22.4063720486285,
-9.72714292012351));
#40943=CARTESIAN_POINT('Ctrl Pts',(-4.29796499089189,-22.390438848756,-9.58769290003277));
#40944=CARTESIAN_POINT('Ctrl Pts',(-4.87268905354279,-22.3612041365895,
-9.30642702146816));
#40945=CARTESIAN_POINT('Ctrl Pts',(-5.12415824032289,-22.3480402573149,
-9.1703698004908));
#40946=CARTESIAN_POINT('Ctrl Pts',(-5.9361095214585,-22.3045007329254,-8.68722756834665));
#40947=CARTESIAN_POINT('Ctrl Pts',(-6.46949146700468,-22.274288523468,-8.29765273153006));
#40948=CARTESIAN_POINT('Ctrl Pts',(-7.31903068547389,-22.2229760793682,
-7.54514475759568));
#40949=CARTESIAN_POINT('Ctrl Pts',(-7.65336598045431,-22.2017063732082,
-7.20579017911899));
#40950=CARTESIAN_POINT('Ctrl Pts',(-8.19613841000151,-22.1643093722904,
-6.57431773809772));
#40951=CARTESIAN_POINT('Ctrl Pts',(-8.41478982117273,-22.1482151012864,
-6.29203040106584));
#40952=CARTESIAN_POINT('Ctrl Pts',(-8.80430054692049,-22.1170094087629,
-5.73244242234787));
#40953=CARTESIAN_POINT('Ctrl Pts',(-8.97747011337554,-22.102019170908,-5.45725501845262));
#40954=CARTESIAN_POINT('Ctrl Pts',(-9.41030252966894,-22.0615496413099,
-4.69291805059709));
#40955=CARTESIAN_POINT('Ctrl Pts',(-9.64451601360296,-22.0362064635198,
-4.19053807975288));
#40956=CARTESIAN_POINT('Ctrl Pts',(-9.99791547121999,-21.9904499283073,
-3.24371744513277));
#40957=CARTESIAN_POINT('Ctrl Pts',(-10.1296434741463,-21.9699808940398,
-2.8054135521693));
#40958=CARTESIAN_POINT('Ctrl Pts',(-10.31734413195,-21.9325019284077,-1.99156133970853));
#40959=CARTESIAN_POINT('Ctrl Pts',(-10.3823447247696,-21.9155136750956,
-1.61889487774995));
#40960=CARTESIAN_POINT('Ctrl Pts',(-10.5030076144496,-21.8689692439359,
-0.607126987358097));
#40961=CARTESIAN_POINT('Ctrl Pts',(-10.5204832514869,-21.8392641814794,
0.0348922578667292));
#40962=CARTESIAN_POINT('Ctrl Pts',(-10.4449071686769,-21.785421023033,1.20908565829536));
#40963=CARTESIAN_POINT('Ctrl Pts',(-10.3696412030061,-21.7612284501406,
1.74026880283431));
#40964=CARTESIAN_POINT('Ctrl Pts',(-10.1247818277644,-21.710204092864,2.84958961418419));
#40965=CARTESIAN_POINT('Ctrl Pts',(-9.94536935611983,-21.6834558891121,
3.42359290542861));
#40966=CARTESIAN_POINT('Ctrl Pts',(-9.59710590798032,-21.6414012727804,
4.27412882816889));
#40967=CARTESIAN_POINT('Ctrl Pts',(-9.46294310112404,-21.6266997482495,
4.56347724468131));
#40968=CARTESIAN_POINT('Ctrl Pts',(-9.05704833891964,-21.5861763648574,
5.34371529786909));
#40969=CARTESIAN_POINT('Ctrl Pts',(-8.75883552642321,-21.5604901799677,
5.81964293282196));
#40970=CARTESIAN_POINT('Ctrl Pts',(-8.15172709732509,-21.514445948901,6.63538914960673));
#40971=CARTESIAN_POINT('Ctrl Pts',(-7.85585685223666,-21.4940221454076,
6.98316279103273));
#40972=CARTESIAN_POINT('Ctrl Pts',(-7.27284316228942,-21.4564448514398,
7.58433648259945));
#40973=CARTESIAN_POINT('Ctrl Pts',(-6.99266881941011,-21.4393122697469,
7.8434040017997));
#40974=CARTESIAN_POINT('Ctrl Pts',(-6.20550144937807,-21.3926213532581,
8.49549654692277));
#40975=CARTESIAN_POINT('Ctrl Pts',(-5.67558875802255,-21.3629161952602,
8.85829639766727));
#40976=CARTESIAN_POINT('Ctrl Pts',(-4.65071984931404,-21.3092081106712,
9.43003485904779));
#40977=CARTESIAN_POINT('Ctrl Pts',(-4.16644892800853,-21.2851465828459,
9.65378040094941));
#40978=CARTESIAN_POINT('Ctrl Pts',(-3.10190238043785,-21.2341148599773,
10.0505355741598));
#40979=CARTESIAN_POINT('Ctrl Pts',(-2.51942526000138,-21.2072357234102,
10.2121276927707));
#40980=CARTESIAN_POINT('Ctrl Pts',(-1.6136871428915,-21.1650814863832,10.381143529226));
#40981=CARTESIAN_POINT('Ctrl Pts',(-1.29859330519493,-21.1504174360658,
10.4252472504763));
#40982=CARTESIAN_POINT('Ctrl Pts',(-0.413545275006808,-21.1094624247547,
10.5083756119576));
#40983=CARTESIAN_POINT('Ctrl Pts',(0.158316546435473,-21.0833144906049,
10.5153193412997));
#40984=CARTESIAN_POINT('Ctrl Pts',(1.18818365570688,-21.0365871872097,10.4437586451435));
#40985=CARTESIAN_POINT('Ctrl Pts',(1.64584983720964,-21.0159369151384,10.3814767005508));
#40986=CARTESIAN_POINT('Ctrl Pts',(2.45742091444955,-20.9787649615925,10.2160014172027));
#40987=CARTESIAN_POINT('Ctrl Pts',(2.81280671748541,-20.9622699862602,10.1239180741488));
#40988=CARTESIAN_POINT('Ctrl Pts',(3.77045720939255,-20.9163944722653,9.82145297041031));
#40989=CARTESIAN_POINT('Ctrl Pts',(4.35952789963926,-20.8868457017479,9.57453993269119));
#40990=CARTESIAN_POINT('Ctrl Pts',(5.38484932548846,-20.833709836774,9.03040909797843));
#40991=CARTESIAN_POINT('Ctrl Pts',(5.82815004985385,-20.8100559510091,8.75086152133243));
#40992=CARTESIAN_POINT('Ctrl Pts',(6.75946559695342,-20.7579892093737,8.06129183010583));
#40993=CARTESIAN_POINT('Ctrl Pts',(7.23477325212092,-20.7296956407351,7.63759444106696));
#40994=CARTESIAN_POINT('Ctrl Pts',(7.9051425651324,-20.6847591221548,6.92093582610613));
#40995=CARTESIAN_POINT('Ctrl Pts',(8.1287956607558,-20.6687988423574,6.65682438153097));
#40996=CARTESIAN_POINT('Ctrl Pts',(8.66423284190235,-20.6282304641132,5.95721583962474));
#40997=CARTESIAN_POINT('Ctrl Pts',(8.95650810981446,-20.6037577438035,5.50802474448138));
#40998=CARTESIAN_POINT('Ctrl Pts',(9.43837940585966,-20.558315149391,4.62688874302381));
#40999=CARTESIAN_POINT('Ctrl Pts',(9.63564732829537,-20.5373260610621,4.20064404240522));
#41000=CARTESIAN_POINT('Ctrl Pts',(9.93082880038755,-20.500341761071,3.4315330518541));
#41001=CARTESIAN_POINT('Ctrl Pts',(10.0410467818482,-20.484379886629,3.09421328464689));
#41002=CARTESIAN_POINT('Ctrl Pts',(10.2093893104803,-20.4550281480888,2.47429834566571));
#41003=CARTESIAN_POINT('Ctrl Pts',(10.2733465128307,-20.441775257999,2.19365705868249));
#41004=CARTESIAN_POINT('Ctrl Pts',(10.3362442290325,-20.4258473136096,1.85375707557567));
#41005=CARTESIAN_POINT('Ctrl Pts',(10.3463163024248,-20.4231771163331,1.79669050433489));
#41006=CARTESIAN_POINT('Ctrl Pts',(10.3559140572458,-20.4205078998763,1.73955311472209));
#41007=CARTESIAN_POINT('Origin',(0.,-13.3748739960349,0.));
#41008=CARTESIAN_POINT('',(-12.1744999967658,-23.8748739960011,0.000280623926547941));
#41009=CARTESIAN_POINT('Ctrl Pts',(7.41272179941102,-21.9374490664136,-9.65763976210216));
#41010=CARTESIAN_POINT('Ctrl Pts',(7.63814242828085,-21.9485939981776,-9.48461814907643));
#41011=CARTESIAN_POINT('Ctrl Pts',(7.85752362648661,-21.9597389299416,-9.30368459558577));
#41012=CARTESIAN_POINT('Ctrl Pts',(8.07031593182521,-21.9708838617056,-9.11528666639334));
#41013=CARTESIAN_POINT('Ctrl Pts',(8.28308879835672,-21.9820277753681,-8.92690594755537));
#41014=CARTESIAN_POINT('Ctrl Pts',(8.48927377437015,-21.9931716890305,-8.7310623915339));
#41015=CARTESIAN_POINT('Ctrl Pts',(8.68835576973433,-22.004315602693,-8.5282427421201));
#41016=CARTESIAN_POINT('Ctrl Pts',(8.88745520365534,-22.0154604925049,-8.32540532675024));
#41017=CARTESIAN_POINT('Ctrl Pts',(9.07945022461544,-22.0266053823167,-8.11559078522033));
#41018=CARTESIAN_POINT('Ctrl Pts',(9.26386275874899,-22.0377502721286,-7.89932256823732));
#41019=CARTESIAN_POINT('Ctrl Pts',(9.44827425420413,-22.0488950991684,-7.68305556935552));
#41020=CARTESIAN_POINT('Ctrl Pts',(9.62510317680151,-22.0600399262082,-7.46033517215365));
#41021=CARTESIAN_POINT('Ctrl Pts',(9.79391130575108,-22.071184753248,-7.23171843928408));
#41022=CARTESIAN_POINT('Ctrl Pts',(9.96275714478459,-22.0823320699331,-7.00305063567375));
#41023=CARTESIAN_POINT('Ctrl Pts',(10.1235784500975,-22.0934793866182,-6.76848407820211));
#41024=CARTESIAN_POINT('Ctrl Pts',(10.2759790307611,-22.1046267033033,-6.52860668208442));
#41025=CARTESIAN_POINT('Ctrl Pts',(10.396545869554,-22.113445545908,-6.33883536217311));
#41026=CARTESIAN_POINT('Ctrl Pts',(10.5118432533725,-22.1222643885128,-6.14574079649067));
#41027=CARTESIAN_POINT('Ctrl Pts',(10.6216946965625,-22.1310832311175,-5.94962620868038));
#41028=CARTESIAN_POINT('Ctrl Pts',(10.7605504536662,-22.142230531791,-5.70173106248375));
#41029=CARTESIAN_POINT('Ctrl Pts',(10.8907448834759,-22.1533778324646,-5.44893572672557));
#41030=CARTESIAN_POINT('Ctrl Pts',(11.0119467530863,-22.1645251331381,-5.19186661588989));
#41031=CARTESIAN_POINT('Ctrl Pts',(11.1331280357991,-22.1756705403727,-4.93484116985485));
#41032=CARTESIAN_POINT('Ctrl Pts',(11.2453196941389,-22.1868159476073,-4.67354363924067));
#41033=CARTESIAN_POINT('Ctrl Pts',(11.3482374041766,-22.197961354842,-4.4086231488353));
#41034=CARTESIAN_POINT('Ctrl Pts',(11.4511436882338,-22.2091055247074,-4.14373207004787));
#41035=CARTESIAN_POINT('Ctrl Pts',(11.5447779833641,-22.2202496945728,-3.87521908322489));
#41036=CARTESIAN_POINT('Ctrl Pts',(11.6289044340638,-22.2313938644382,-3.60375247671244));
#41037=CARTESIAN_POINT('Ctrl Pts',(11.7156802739049,-22.2428889969602,-3.32373658904568));
#41038=CARTESIAN_POINT('Ctrl Pts',(11.7923396078499,-22.2543841294822,-3.04057831121346));
#41039=CARTESIAN_POINT('Ctrl Pts',(11.8586790366336,-22.2658792620043,-2.75502844923715));
#41040=CARTESIAN_POINT('Ctrl Pts',(11.9229964655407,-22.2770240273771,-2.47818203551626));
#41041=CARTESIAN_POINT('Ctrl Pts',(11.9776137036276,-22.2881687927499,-2.19908793968349));
#41042=CARTESIAN_POINT('Ctrl Pts',(12.0223969991253,-22.2993135581228,-1.91844224448467));
#41043=CARTESIAN_POINT('Ctrl Pts',(12.0692921285266,-22.3109838742194,-1.62456221520089));
#41044=CARTESIAN_POINT('Ctrl Pts',(12.1054034747325,-22.322654190316,-1.32898104250057));
#41045=CARTESIAN_POINT('Ctrl Pts',(12.1306380526509,-22.3343245064127,-1.03250699057049));
#41046=CARTESIAN_POINT('Ctrl Pts',(12.1558726305694,-22.3459948225093,-0.736032938640407));
#41047=CARTESIAN_POINT('Ctrl Pts',(12.1702304204935,-22.3576651386059,-0.438666342520084));
#41048=CARTESIAN_POINT('Ctrl Pts',(12.1736809240298,-22.3693354547026,-0.14121972211462));
#41049=CARTESIAN_POINT('Ctrl Pts',(12.1769767929329,-22.3804827645107,0.142896800657586));
#41050=CARTESIAN_POINT('Ctrl Pts',(12.1703224929076,-22.3916300743188,0.427171187125004));
#41051=CARTESIAN_POINT('Ctrl Pts',(12.1537269468445,-22.4027773841269,0.710894894865639));
#41052=CARTESIAN_POINT('Ctrl Pts',(12.1371342194696,-22.4139228006082,0.99457041324932));
#41053=CARTESIAN_POINT('Ctrl Pts',(12.11060363268,-22.4250682170895,1.2776951734493));
#41054=CARTESIAN_POINT('Ctrl Pts',(12.074196166311,-22.4362136335708,1.55956313993394));
#41055=CARTESIAN_POINT('Ctrl Pts',(12.0377927416301,-22.4473578127703,1.84139981551791));
#41056=CARTESIAN_POINT('Ctrl Pts',(11.9915146609846,-22.4585019919697,2.12197971150438));
#41057=CARTESIAN_POINT('Ctrl Pts',(11.9354746331794,-22.4696461711692,2.40060315977681));
#41058=CARTESIAN_POINT('Ctrl Pts',(11.8776698234813,-22.4811412967624,2.68800086523175));
#41059=CARTESIAN_POINT('Ctrl Pts',(11.8094783169454,-22.4926364223556,2.97331661069409));
#41060=CARTESIAN_POINT('Ctrl Pts',(11.7310808084977,-22.5041315479488,3.25579380712257));
#41061=CARTESIAN_POINT('Ctrl Pts',(11.6550727153316,-22.5152763227554,3.52966160583902));
#41062=CARTESIAN_POINT('Ctrl Pts',(11.5694716039288,-22.5264210975619,3.80086105222759));
#41063=CARTESIAN_POINT('Ctrl Pts',(11.474493137458,-22.5375658723685,4.06871693392769));
#41064=CARTESIAN_POINT('Ctrl Pts',(11.3750360097731,-22.549236173355,4.34920342331078));
#41065=CARTESIAN_POINT('Ctrl Pts',(11.2652959853262,-22.5609064743416,4.62602313302054));
#41066=CARTESIAN_POINT('Ctrl Pts',(11.1455782047075,-22.5725767753281,4.89842186145174));
#41067=CARTESIAN_POINT('Ctrl Pts',(11.0258604240889,-22.5842470763146,5.17082058988296));
#41068=CARTESIAN_POINT('Ctrl Pts',(10.8961650303231,-22.5959173773012,5.43879803342295));
#41069=CARTESIAN_POINT('Ctrl Pts',(10.7568540674013,-22.6075876782877,5.7016261559867));
#41070=CARTESIAN_POINT('Ctrl Pts',(10.6237862289835,-22.6187349828027,5.95267581791911));
#41071=CARTESIAN_POINT('Ctrl Pts',(10.4819059659421,-22.6298822873177,6.19910251958811));
#41072=CARTESIAN_POINT('Ctrl Pts',(10.331560180348,-22.6410295918327,6.44028838561183));
#41073=CARTESIAN_POINT('Ctrl Pts',(10.1812399312278,-22.65217500296,6.68143328582788));
#41074=CARTESIAN_POINT('Ctrl Pts',(10.0224571713426,-22.6633204140874,6.91733890132943));
#41075=CARTESIAN_POINT('Ctrl Pts',(9.85560331246683,-22.6744658252148,7.14741446939331));
#41076=CARTESIAN_POINT('Ctrl Pts',(9.68876797717992,-22.6856099990138,7.37746449519372));
#41077=CARTESIAN_POINT('Ctrl Pts',(9.51386348868994,-22.6967541728128,7.60168555009459));
#41078=CARTESIAN_POINT('Ctrl Pts',(9.33132363306435,-22.7078983466118,7.81951721687565));
#41079=CARTESIAN_POINT('Ctrl Pts',(9.14303517522473,-22.7193934762169,8.04420890662349));
#41080=CARTESIAN_POINT('Ctrl Pts',(8.94662282970408,-22.7308886058219,8.2621020201305));
#41081=CARTESIAN_POINT('Ctrl Pts',(8.74260731912746,-22.742383735427,8.47261869279735));
#41082=CARTESIAN_POINT('Ctrl Pts',(8.54481000069459,-22.7535285047855,8.67671902429285));
#41083=CARTESIAN_POINT('Ctrl Pts',(8.33986632224137,-22.7646732741439,8.87388570935971));
#41084=CARTESIAN_POINT('Ctrl Pts',(8.12828876731095,-22.7758180435024,9.06362907257389));
#41085=CARTESIAN_POINT('Ctrl Pts',(7.90673410626793,-22.7874883532308,9.26231993340696));
#41086=CARTESIAN_POINT('Ctrl Pts',(7.67790509962409,-22.7991586629592,9.45287030906363));
#41087=CARTESIAN_POINT('Ctrl Pts',(7.44243059986101,-22.8108289726876,9.63476398342235));
#41088=CARTESIAN_POINT('Ctrl Pts',(7.20695610009792,-22.822499282416,9.81665765778107));
#41089=CARTESIAN_POINT('Ctrl Pts',(6.9648363780942,-22.8341695921444,9.98989443269218));
#41090=CARTESIAN_POINT('Ctrl Pts',(6.71673773003182,-22.8458399018728,10.1540082980056));
#41091=CARTESIAN_POINT('Ctrl Pts',(6.47975757864706,-22.8569872087515,10.3107674297061));
#41092=CARTESIAN_POINT('Ctrl Pts',(6.23725183406651,-22.8681345156302,10.4592501796308));
#41093=CARTESIAN_POINT('Ctrl Pts',(5.98982077868779,-22.8792818225089,10.5990800208886));
#41094=CARTESIAN_POINT('Ctrl Pts',(5.7424317492995,-22.8904272360254,10.7388861121464));
#41095=CARTESIAN_POINT('Ctrl Pts',(5.49011931144717,-22.9015726495419,10.8700420977849));
#41096=CARTESIAN_POINT('Ctrl Pts',(5.2335098553344,-22.9127180630584,10.9922165573699));
#41097=CARTESIAN_POINT('Ctrl Pts',(4.97692888674906,-22.9238622392655,11.1143774537437));
#41098=CARTESIAN_POINT('Ctrl Pts',(4.71605209324548,-22.9350064154727,11.227558700446));
#41099=CARTESIAN_POINT('Ctrl Pts',(4.45152855075324,-22.9461505916799,11.3314758002578));
#41100=CARTESIAN_POINT('Ctrl Pts',(4.17867465159937,-22.9576457194947,11.4386654500156));
#41101=CARTESIAN_POINT('Ctrl Pts',(3.90194086783386,-22.9691408473095,11.535997888534));
#41102=CARTESIAN_POINT('Ctrl Pts',(3.62206095978642,-22.9806359751244,11.6232149018071));
#41103=CARTESIAN_POINT('Ctrl Pts',(3.3507114148116,-22.9917807469079,11.7077736578494));
#41104=CARTESIAN_POINT('Ctrl Pts',(3.07640495140956,-23.0029255186914,11.7828243840286));
#41105=CARTESIAN_POINT('Ctrl Pts',(2.79982589396561,-23.014070290475,11.8481823590574));
#41106=CARTESIAN_POINT('Ctrl Pts',(2.51020469315729,-23.0257405963054,11.9166223030835));
#41107=CARTESIAN_POINT('Ctrl Pts',(2.21809172121681,-23.0374109021359,11.9744332999611));
#41108=CARTESIAN_POINT('Ctrl Pts',(1.92428618151177,-23.0490812079664,12.0214630116988));
#41109=CARTESIAN_POINT('Ctrl Pts',(1.63048064180675,-23.0607515137969,12.0684927234366));
#41110=CARTESIAN_POINT('Ctrl Pts',(1.33498286700784,-23.0724218196274,12.1047411056734));
#41111=CARTESIAN_POINT('Ctrl Pts',(1.03860091274412,-23.0840921254579,12.1301178227603));
#41112=CARTESIAN_POINT('Ctrl Pts',(0.755501187515748,-23.0952394315824,
12.1543572932515));
#41113=CARTESIAN_POINT('Ctrl Pts',(0.471510238288568,-23.1063867377068,
12.1686853376153));
#41114=CARTESIAN_POINT('Ctrl Pts',(0.187335335693578,-23.1175340438313,
12.1730586017648));
#41115=CARTESIAN_POINT('Ctrl Pts',(-0.0967912998095614,-23.1286794565864,
12.1774311231157));
#41116=CARTESIAN_POINT('Ctrl Pts',(-0.381101559686401,-23.1398248693415,
12.1718522358687));
#41117=CARTESIAN_POINT('Ctrl Pts',(-0.664886834336528,-23.1509702820966,
12.1563306860058));
#41118=CARTESIAN_POINT('Ctrl Pts',(-0.948640604399958,-23.1621144575373,
12.1408108592767));
#41119=CARTESIAN_POINT('Ctrl Pts',(-1.2318692393348,-23.1732586329779,12.1153505885898));
#41120=CARTESIAN_POINT('Ctrl Pts',(-1.51386666477452,-23.1844028084186,
12.0800106776147));
#41121=CARTESIAN_POINT('Ctrl Pts',(-1.80474476760346,-23.195897936804,12.0435578403501));
#41122=CARTESIAN_POINT('Ctrl Pts',(-2.09431256209703,-23.2073930651893,
11.9965930464181));
#41123=CARTESIAN_POINT('Ctrl Pts',(-2.38180219291559,-23.2188881935747,
11.9392407029854));
#41124=CARTESIAN_POINT('Ctrl Pts',(-2.66052949347101,-23.2300329645888,
11.8836363884227));
#41125=CARTESIAN_POINT('Ctrl Pts',(-2.93730316054586,-23.2411777356028,
11.8182684020138));
#41126=CARTESIAN_POINT('Ctrl Pts',(-3.21143391640609,-23.2523225066169,
11.743302025008));
#41127=CARTESIAN_POINT('Ctrl Pts',(-3.49849141578954,-23.2639928136879,
11.6648005790335));
#41128=CARTESIAN_POINT('Ctrl Pts',(-3.78265044479702,-23.2756631207589,
11.5757738130286));
#41129=CARTESIAN_POINT('Ctrl Pts',(-4.06313635096133,-23.2873334278299,
11.4764704174888));
#41130=CARTESIAN_POINT('Ctrl Pts',(-4.34362225712563,-23.299003734901,11.3771670219491));
#41131=CARTESIAN_POINT('Ctrl Pts',(-4.62043472711151,-23.310674041972,11.2675871171198));
#41132=CARTESIAN_POINT('Ctrl Pts',(-4.89282100638345,-23.322344349043,11.1480380717637));
#41133=CARTESIAN_POINT('Ctrl Pts',(-5.15300038646404,-23.3334916552407,
11.0338465765346));
#41134=CARTESIAN_POINT('Ctrl Pts',(-5.40921927779757,-23.3446389614383,
10.9105257231928));
#41135=CARTESIAN_POINT('Ctrl Pts',(-5.66083590451648,-23.355786267636,10.7783759032675));
#41136=CARTESIAN_POINT('Ctrl Pts',(-5.91240979416356,-23.3669316804642,
10.6462485289827));
#41137=CARTESIAN_POINT('Ctrl Pts',(-6.15938274378058,-23.3780770932925,
10.5052953060483));
#41138=CARTESIAN_POINT('Ctrl Pts',(-6.40113673390645,-23.3892225061207,
10.3558630139566));
#41139=CARTESIAN_POINT('Ctrl Pts',(-6.64286388556777,-23.4003666816343,
10.2064473111806));
#41140=CARTESIAN_POINT('Ctrl Pts',(-6.87937300783742,-23.4115108571478,
10.0485545591068));
#41141=CARTESIAN_POINT('Ctrl Pts',(-7.11007321917927,-23.4226550326614,
9.882576034006));
#41142=CARTESIAN_POINT('Ctrl Pts',(-7.34803865072143,-23.4341501609919,
9.71137050661351));
#41143=CARTESIAN_POINT('Ctrl Pts',(-7.57982312721504,-23.4456452893225,
9.53156184412831));
#41144=CARTESIAN_POINT('Ctrl Pts',(-7.80481195646738,-23.457140417653,9.34362673559812));
#41145=CARTESIAN_POINT('Ctrl Pts',(-8.02294340543191,-23.4682851887384,
9.16141965593453));
#41146=CARTESIAN_POINT('Ctrl Pts',(-8.23468710462325,-23.4794299598237,
8.97157434171908));
#41147=CARTESIAN_POINT('Ctrl Pts',(-8.43951691801119,-23.4905747309091,
8.77456576934739));
#41148=CARTESIAN_POINT('Ctrl Pts',(-8.65400555820757,-23.5022450378623,
8.56826718372596));
#41149=CARTESIAN_POINT('Ctrl Pts',(-8.86091234015456,-23.5139153448154,
8.35411373254376));
#41150=CARTESIAN_POINT('Ctrl Pts',(-9.05967607823019,-23.5255856517686,
8.13269448630303));
#41151=CARTESIAN_POINT('Ctrl Pts',(-9.2584398163058,-23.5372559587218,7.91127524006232));
#41152=CARTESIAN_POINT('Ctrl Pts',(-9.44906029292414,-23.5489262656749,
7.68259045429057));
#41153=CARTESIAN_POINT('Ctrl Pts',(-9.631023630308,-23.5605965726281,7.44727024368318));
#41154=CARTESIAN_POINT('Ctrl Pts',(-9.8048323458045,-23.5717438789489,7.22249582415408));
#41155=CARTESIAN_POINT('Ctrl Pts',(-9.97079470968131,-23.5828911852698,
6.99160050424424));
#41156=CARTESIAN_POINT('Ctrl Pts',(-10.128490951645,-23.5940384915906,6.75515516420202));
#41157=CARTESIAN_POINT('Ctrl Pts',(-10.286160408936,-23.6051839045438,6.51874998434983));
#41158=CARTESIAN_POINT('Ctrl Pts',(-10.4355663994461,-23.6163293174971,
6.27679688823947));
#41159=CARTESIAN_POINT('Ctrl Pts',(-10.5763322111555,-23.6274747304504,
6.0298961192773));
#41160=CARTESIAN_POINT('Ctrl Pts',(-10.7170823956828,-23.6386189060904,
5.78302276011893));
#41161=CARTESIAN_POINT('Ctrl Pts',(-10.8491941846832,-23.6497630817305,
5.53120305658148));
#41162=CARTESIAN_POINT('Ctrl Pts',(-10.9723359885886,-23.6609072573705,
5.27506333644663));
#41163=CARTESIAN_POINT('Ctrl Pts',(-11.0993557765869,-23.6724023856074,
5.01085725924436));
#41164=CARTESIAN_POINT('Ctrl Pts',(-11.2168313213538,-23.6838975138443,
4.74205492746937));
#41165=CARTESIAN_POINT('Ctrl Pts',(-11.3244509997133,-23.6953926420812,
4.46936906118676));
#41166=CARTESIAN_POINT('Ctrl Pts',(-11.4287905658947,-23.7065374132952,
4.20499431647958));
#41167=CARTESIAN_POINT('Ctrl Pts',(-11.5238660555388,-23.7176821845091,
3.93696952183191));
#41168=CARTESIAN_POINT('Ctrl Pts',(-11.6094427838768,-23.7288269557231,
3.66596351562464));
#41169=CARTESIAN_POINT('Ctrl Pts',(-11.6990549123853,-23.7404972624715,
3.38217812762871));
#41170=CARTESIAN_POINT('Ctrl Pts',(-11.7782507937505,-23.7521675692198,
3.09512390584126));
#41171=CARTESIAN_POINT('Ctrl Pts',(-11.8468195663286,-23.7638378759682,
2.80558664326246));
#41172=CARTESIAN_POINT('Ctrl Pts',(-11.9153883389068,-23.7755081827165,
2.51604938068365));
#41173=CARTESIAN_POINT('Ctrl Pts',(-11.9733299339243,-23.7871784894648,
2.22402940580713));
#41174=CARTESIAN_POINT('Ctrl Pts',(-12.0204946704578,-23.7988487962132,
1.93032591224761));
#41175=CARTESIAN_POINT('Ctrl Pts',(-12.0672414471629,-23.8104156841837,
1.63922513145235));
#41176=CARTESIAN_POINT('Ctrl Pts',(-12.1034122499846,-23.8219825721543,
1.34640866791079));
#41177=CARTESIAN_POINT('Ctrl Pts',(-12.1289081894145,-23.8335494601249,
1.05263307128082));
#41178=CARTESIAN_POINT('Ctrl Pts',(-12.1543967460716,-23.8451129987108,
0.758942542255195));
#41179=CARTESIAN_POINT('Ctrl Pts',(-12.1692165959912,-23.8566765372968,
0.464293654495028));
#41180=CARTESIAN_POINT('Ctrl Pts',(-12.1733207336769,-23.8682400758828,
0.169447823923155));
#41181=CARTESIAN_POINT('Ctrl Pts',(-12.1741055719096,-23.8704513825889,
0.11306416959796));
#41182=CARTESIAN_POINT('Ctrl Pts',(-12.1744986969062,-23.872662689295,0.056673323816421));
#41183=CARTESIAN_POINT('Ctrl Pts',(-12.1744999967658,-23.8748739960011,
0.000280623926556051));
#41184=CARTESIAN_POINT('Ctrl Pts',(-12.1744999967658,-23.8748739960349,
0.00028062306491734));
#41185=CARTESIAN_POINT('Ctrl Pts',(-12.1745065428157,-23.8860100974646,
-0.283712015376132));
#41186=CARTESIAN_POINT('Ctrl Pts',(-12.1645717688562,-23.8971461988943,
-0.567720156626778));
#41187=CARTESIAN_POINT('Ctrl Pts',(-12.1447184939399,-23.908282300324,-0.8510363993127));
#41188=CARTESIAN_POINT('Ctrl Pts',(-12.1248634023349,-23.9194194207708,
-1.13437856706043));
#41189=CARTESIAN_POINT('Ctrl Pts',(-12.0950880117066,-23.9305565412177,
-1.41702844262597));
#41190=CARTESIAN_POINT('Ctrl Pts',(-12.0554671639295,-23.9416936616646,
-1.6982819876032));
#41191=CARTESIAN_POINT('Ctrl Pts',(-12.0158465226463,-23.9528307240675,
-1.97953406675724));
#41192=CARTESIAN_POINT('Ctrl Pts',(-11.9663805663668,-23.9639677864705,
-2.25938956526504));
#41193=CARTESIAN_POINT('Ctrl Pts',(-11.9071957223858,-23.9751048488735,
-2.53715200151623));
#41194=CARTESIAN_POINT('Ctrl Pts',(-11.8479967642311,-23.9862445672002,
-2.81498067748367));
#41195=CARTESIAN_POINT('Ctrl Pts',(-11.7790743410825,-23.9973842855269,
-3.09071503164591));
#41196=CARTESIAN_POINT('Ctrl Pts',(-11.7006058479935,-24.0085240038537,
-3.36366957947735));
#41197=CARTESIAN_POINT('Ctrl Pts',(-11.6335067433188,-24.0180496758352,
-3.59707543519565));
#41198=CARTESIAN_POINT('Ctrl Pts',(-11.5594283093542,-24.0275753478167,
-3.82844876548518));
#41199=CARTESIAN_POINT('Ctrl Pts',(-11.4785103889095,-24.0371010197983,
-4.05736977630798));
#41200=CARTESIAN_POINT('Ctrl Pts',(-11.3838171384972,-24.0482483260728,
-4.32526191297343));
#41201=CARTESIAN_POINT('Ctrl Pts',(-11.2797273169031,-24.0593956323473,
-4.58987760285483));
#41202=CARTESIAN_POINT('Ctrl Pts',(-11.1664931690163,-24.0705429386218,
-4.85055466481025));
#41203=CARTESIAN_POINT('Ctrl Pts',(-11.053278253932,-24.081688351528,-5.11118745080703));
#41204=CARTESIAN_POINT('Ctrl Pts',(-10.9309222196804,-24.0928337644342,
-5.36788269991822));
#41205=CARTESIAN_POINT('Ctrl Pts',(-10.7997253247509,-24.1039791773405,
-5.61999850177324));
#41206=CARTESIAN_POINT('Ctrl Pts',(-10.6685429947127,-24.115123352933,-5.87208631486202));
#41207=CARTESIAN_POINT('Ctrl Pts',(-10.5285218869459,-24.1262675285254,
-6.11959545930329));
#41208=CARTESIAN_POINT('Ctrl Pts',(-10.3800086368805,-24.1374117041179,
-6.36190780727653));
#41209=CARTESIAN_POINT('Ctrl Pts',(-10.2268184035207,-24.14890683239,-6.61185106227649));
#41210=CARTESIAN_POINT('Ctrl Pts',(-10.0645926378427,-24.1604019606621,
-6.85626464349746));
#41211=CARTESIAN_POINT('Ctrl Pts',(-9.89376139950918,-24.1718970889342,
-7.09450037843273));
#41212=CARTESIAN_POINT('Ctrl Pts',(-9.72813688326918,-24.1830418601,-7.32547498667565));
#41213=CARTESIAN_POINT('Ctrl Pts',(-9.55442385726194,-24.1941866312657,
-7.55064253139713));
#41214=CARTESIAN_POINT('Ctrl Pts',(-9.37305720387854,-24.2053314024315,
-7.76944328139543));
#41215=CARTESIAN_POINT('Ctrl Pts',(-9.18313814126281,-24.2170017092568,
-7.99856165880439));
#41216=CARTESIAN_POINT('Ctrl Pts',(-8.98482646679887,-24.2286720160821,
-8.22069809174982));
#41217=CARTESIAN_POINT('Ctrl Pts',(-8.77866826149681,-24.2403423229074,
-8.43524948087421));
#41218=CARTESIAN_POINT('Ctrl Pts',(-8.57251005619474,-24.2520126297327,
-8.6498008699986));
#41219=CARTESIAN_POINT('Ctrl Pts',(-8.35850555884004,-24.263682936558,-8.85676697946432));
#41220=CARTESIAN_POINT('Ctrl Pts',(-8.13724527165577,-24.2753532433833,
-9.05558886207384));
#41221=CARTESIAN_POINT('Ctrl Pts',(-7.92590068440107,-24.2865005496194,
-9.24550061375804));
#41222=CARTESIAN_POINT('Ctrl Pts',(-7.70787322336667,-24.2976478558555,
-9.42803877404122));
#41223=CARTESIAN_POINT('Ctrl Pts',(-7.48370125772818,-24.3087951620916,
-9.60274261526766));
#41224=CARTESIAN_POINT('Ctrl Pts',(-7.25956736767171,-24.3199405749591,
-9.77741678306721));
#41225=CARTESIAN_POINT('Ctrl Pts',(-7.02929126696434,-24.3310859878265,
-9.94425912456056));
#41226=CARTESIAN_POINT('Ctrl Pts',(-6.79344378337951,-24.342231400694,-10.1028496876902));
#41227=CARTESIAN_POINT('Ctrl Pts',(-6.55762248253287,-24.3533755762473,
-10.2614226448012));
#41228=CARTESIAN_POINT('Ctrl Pts',(-6.31623125517515,-24.3645197518006,
-10.4117455039978));
#41229=CARTESIAN_POINT('Ctrl Pts',(-6.06987027004878,-24.3756639273539,
-10.5534413891762));
#41230=CARTESIAN_POINT('Ctrl Pts',(-5.81575087656889,-24.3871590556551,
-10.6995995658927));
#41231=CARTESIAN_POINT('Ctrl Pts',(-5.55634388989934,-24.3986541839563,
-10.836578445479));
#41232=CARTESIAN_POINT('Ctrl Pts',(-5.29233710829935,-24.4101493122576,
-10.9640146927172));
#41233=CARTESIAN_POINT('Ctrl Pts',(-5.03637692415595,-24.4212940833839,
-11.0875668420671));
#41234=CARTESIAN_POINT('Ctrl Pts',(-4.776093436397,-24.4324388545102,-11.2021493190998));
#41235=CARTESIAN_POINT('Ctrl Pts',(-4.51213635499412,-24.4435836256365,
-11.3074787536365));
#41236=CARTESIAN_POINT('Ctrl Pts',(-4.2357322807886,-24.4552539325252,-11.4177750362176));
#41237=CARTESIAN_POINT('Ctrl Pts',(-3.95530011241909,-24.4669242394138,
-11.517924499486));
#41238=CARTESIAN_POINT('Ctrl Pts',(-3.67160795292729,-24.4785945463025,
-11.6076589065152));
#41239=CARTESIAN_POINT('Ctrl Pts',(-3.38791579343547,-24.4902648531912,
-11.6973933135444));
#41240=CARTESIAN_POINT('Ctrl Pts',(-3.10096396534875,-24.5019351600798,
-11.7767125715228));
#41241=CARTESIAN_POINT('Ctrl Pts',(-2.81153844769576,-24.5136054669685,
-11.8454084694082));
#41242=CARTESIAN_POINT('Ctrl Pts',(-2.53508343133578,-24.5247527732184,
-11.9110257851439));
#41243=CARTESIAN_POINT('Ctrl Pts',(-2.25628900057298,-24.5359000794684,
-11.9669705731406));
#41244=CARTESIAN_POINT('Ctrl Pts',(-1.97584835600998,-24.5470473857183,
-12.0130959175415));
#41245=CARTESIAN_POINT('Ctrl Pts',(-1.69545534425414,-24.5581927985997,
-12.0592134275587));
#41246=CARTESIAN_POINT('Ctrl Pts',(-1.41341694004882,-24.5693382114811,
-12.0955147805296));
#41247=CARTESIAN_POINT('Ctrl Pts',(-1.13043533186696,-24.5804836243626,
-12.1219043970189));
#41248=CARTESIAN_POINT('Ctrl Pts',(-0.847485139039732,-24.59162779993,-12.1482910838508));
#41249=CARTESIAN_POINT('Ctrl Pts',(-0.563592216852522,-24.6027719754975,
-12.1647682066767));
#41250=CARTESIAN_POINT('Ctrl Pts',(-0.27946390335161,-24.6139161510649,
-12.1712920504244));
#41251=CARTESIAN_POINT('Ctrl Pts',(0.0136121878271691,-24.6254112793556,
-12.178021343262));
#41252=CARTESIAN_POINT('Ctrl Pts',(0.306938440053736,-24.6369064076464,
-12.1741602840482));
#41253=CARTESIAN_POINT('Ctrl Pts',(0.599737050830206,-24.6484015359371,
-12.1597189819445));
#41254=CARTESIAN_POINT('Ctrl Pts',(0.883611525722814,-24.6595463070775,
-12.1457178326884));
#41255=CARTESIAN_POINT('Ctrl Pts',(1.16698976785748,-24.670691078218,-12.1217718491365));
#41256=CARTESIAN_POINT('Ctrl Pts',(1.44916568538212,-24.6818358493585,-12.0879431280227));
#41257=CARTESIAN_POINT('Ctrl Pts',(1.7446477106438,-24.6935061562243,-12.0525192012949));
#41258=CARTESIAN_POINT('Ctrl Pts',(2.03881097517401,-24.7051764630902,-12.0062580999378));
#41259=CARTESIAN_POINT('Ctrl Pts',(2.33085267230979,-24.716846769956,-11.9492918647921));
#41260=CARTESIAN_POINT('Ctrl Pts',(2.62289436944556,-24.7285170768219,-11.8923256296464));
#41261=CARTESIAN_POINT('Ctrl Pts',(2.91281417157282,-24.7401873836877,-11.8246543335606));
#41262=CARTESIAN_POINT('Ctrl Pts',(3.19982230071158,-24.7518576905535,-11.7464712783827));
#41263=CARTESIAN_POINT('Ctrl Pts',(3.4739656115066,-24.7630048889684,-11.6717926911982));
#41264=CARTESIAN_POINT('Ctrl Pts',(3.74553441079381,-24.7741520873833,-11.5875016792656));
#41265=CARTESIAN_POINT('Ctrl Pts',(4.01384973800586,-24.7852992857982,-11.4938009609837));
#41266=CARTESIAN_POINT('Ctrl Pts',(4.28211826815581,-24.7964445400225,-11.400116585109));
#41267=CARTESIAN_POINT('Ctrl Pts',(4.54713420746316,-24.8075897942468,-11.2970258675264));
#41268=CARTESIAN_POINT('Ctrl Pts',(4.8082352784448,-24.8187350484711,-11.1847808989322));
#41269=CARTESIAN_POINT('Ctrl Pts',(5.0693226528587,-24.8298797180493,-11.0725418183675));
#41270=CARTESIAN_POINT('Ctrl Pts',(5.32649532310743,-24.8410243876275,-10.9511495489443));
#41271=CARTESIAN_POINT('Ctrl Pts',(5.57911119597613,-24.8521690572056,-10.8209042373054));
#41272=CARTESIAN_POINT('Ctrl Pts',(5.83170819246218,-24.8633128940133,-10.6906686580729));
#41273=CARTESIAN_POINT('Ctrl Pts',(6.07974883505326,-24.874456730821,-10.5515814810599));
#41274=CARTESIAN_POINT('Ctrl Pts',(6.32261488353058,-24.8856005676286,-10.403989200521));
#41275=CARTESIAN_POINT('Ctrl Pts',(6.56550075576078,-24.8967453140434,-10.2563848728767));
#41276=CARTESIAN_POINT('Ctrl Pts',(6.80321096137586,-24.9078900604581,-10.1002741921835));
#41277=CARTESIAN_POINT('Ctrl Pts',(7.03515431424307,-24.9190348068728,-9.936048209665));
#41278=CARTESIAN_POINT('Ctrl Pts',(7.1627874146331,-24.9251675048802,-9.84567842301525));
#41279=CARTESIAN_POINT('Ctrl Pts',(7.2886747830738,-24.9313002028877,-9.75285205462969));
#41280=CARTESIAN_POINT('Ctrl Pts',(7.41272179941101,-24.9374329008951,-9.65763976210217));
#41281=CARTESIAN_POINT('',(-12.1744999959752,-23.6251260039651,0.000313050724133792));
#41282=CARTESIAN_POINT('Ctrl Pts',(-12.1744999959752,-23.6251260039651,
0.000313050724133792));
#41283=CARTESIAN_POINT('Ctrl Pts',(-12.1745072760035,-23.6362300684397,
-0.28280626030774));
#41284=CARTESIAN_POINT('Ctrl Pts',(-12.1646342579426,-23.6473341329143,
-0.565958783664843));
#41285=CARTESIAN_POINT('Ctrl Pts',(-12.1449000764791,-23.6584381973888,
-0.848441148423234));
#41286=CARTESIAN_POINT('Ctrl Pts',(-12.1251680288802,-23.6695410611767,
-1.13089296825575));
#41287=CARTESIAN_POINT('Ctrl Pts',(-12.0955769658755,-23.6806439249646,
-1.41267450420121));
#41288=CARTESIAN_POINT('Ctrl Pts',(-12.0561980343215,-23.6917467887524,
-1.69308570581112));
#41289=CARTESIAN_POINT('Ctrl Pts',(-12.0168162232634,-23.7028504644146,
-1.97351741191864));
#41290=CARTESIAN_POINT('Ctrl Pts',(-11.9676451482731,-23.7139541400767,
-2.25257831493435));
#41291=CARTESIAN_POINT('Ctrl Pts',(-11.9088076155506,-23.7250578157389,
-2.52957534495496));
#41292=CARTESIAN_POINT('Ctrl Pts',(-11.8499700831609,-23.7361614913382,
-2.80657237340874));
#41293=CARTESIAN_POINT('Ctrl Pts',(-11.7814661517746,-23.7472651669375,
-3.08150526454602));
#41294=CARTESIAN_POINT('Ctrl Pts',(-11.7034695576592,-23.7583688425369,
-3.35369207932761));
#41295=CARTESIAN_POINT('Ctrl Pts',(-11.6254556305768,-23.7694749856753,
-3.62593938143092));
#41296=CARTESIAN_POINT('Ctrl Pts',(-11.5379448995412,-23.7805811288137,
-3.89543912724969));
#41297=CARTESIAN_POINT('Ctrl Pts',(-11.4411611446377,-23.7916872719521,
-4.16152398916932));
#41298=CARTESIAN_POINT('Ctrl Pts',(-11.3820531543148,-23.7984700404219,
-4.3240279285868));
#41299=CARTESIAN_POINT('Ctrl Pts',(-11.3194874657191,-23.8052528088917,
-4.48525848955029));
#41300=CARTESIAN_POINT('Ctrl Pts',(-11.2535239975975,-23.8120355773616,
-4.64506704854697));
#41301=CARTESIAN_POINT('Ctrl Pts',(-11.1451147212248,-23.8231828842355,
-4.90770833670762));
#41302=CARTESIAN_POINT('Ctrl Pts',(-11.027490726027,-23.8343301911093,-5.1665920149544));
#41303=CARTESIAN_POINT('Ctrl Pts',(-10.9009381361996,-23.8454774979832,
-5.42106982068579));
#41304=CARTESIAN_POINT('Ctrl Pts',(-10.7744070412407,-23.8566229114949,
-5.67550440354045));
#41305=CARTESIAN_POINT('Ctrl Pts',(-10.6389504981074,-23.8677683250065,
-5.9255343691766));
#41306=CARTESIAN_POINT('Ctrl Pts',(-10.4949015330221,-23.8789137385181,
-6.17053417964529));
#41307=CARTESIAN_POINT('Ctrl Pts',(-10.3508685595493,-23.8900579147204,
-6.41550679143171));
#41308=CARTESIAN_POINT('Ctrl Pts',(-10.1982452040525,-23.9012020909227,
-6.65545013324551));
#41309=CARTESIAN_POINT('Ctrl Pts',(-10.037409578847,-23.9123462671249,-6.88976481430757));
#41310=CARTESIAN_POINT('Ctrl Pts',(-9.87150892940053,-23.9238413949434,
-7.13145851688982));
#41311=CARTESIAN_POINT('Ctrl Pts',(-9.69687054816424,-23.9353365227619,
-7.36716304913461));
#41312=CARTESIAN_POINT('Ctrl Pts',(-9.51395741258113,-23.9468316505804,
-7.59625332658098));
#41313=CARTESIAN_POINT('Ctrl Pts',(-9.33661922343069,-23.957976422359,-7.8183612403992));
#41314=CARTESIAN_POINT('Ctrl Pts',(-9.1515033916188,-23.9691211941376,-8.03425189815682));
#41315=CARTESIAN_POINT('Ctrl Pts',(-8.95907314105923,-23.9802659659162,
-8.24338878757706));
#41316=CARTESIAN_POINT('Ctrl Pts',(-8.75756880151721,-23.9919362717546,
-8.4623875710529));
#41317=CARTESIAN_POINT('Ctrl Pts',(-8.54804383413787,-24.003606577593,-8.67398007541675));
#41318=CARTESIAN_POINT('Ctrl Pts',(-8.33107475358735,-24.0152768834315,
-8.87759222425425));
#41319=CARTESIAN_POINT('Ctrl Pts',(-8.11410567303683,-24.0269471892699,
-9.08120437309175));
#41320=CARTESIAN_POINT('Ctrl Pts',(-7.88969272996757,-24.0386174951083,
-9.27683594321905));
#41321=CARTESIAN_POINT('Ctrl Pts',(-7.65845451946485,-24.0502878009467,
-9.46395924670476));
#41322=CARTESIAN_POINT('Ctrl Pts',(-7.43757914943243,-24.0614351070725,
-9.64269670021316));
#41323=CARTESIAN_POINT('Ctrl Pts',(-7.21041084144513,-24.0725824131983,
-9.81372509541071));
#41324=CARTESIAN_POINT('Ctrl Pts',(-6.97751105217776,-24.0837297193241,
-9.97661213873413));
#41325=CARTESIAN_POINT('Ctrl Pts',(-6.74465082092712,-24.0948751320805,
-10.139471515702));
#41326=CARTESIAN_POINT('Ctrl Pts',(-6.50606127048044,-24.1060205448369,
-10.2941921487503));
#41327=CARTESIAN_POINT('Ctrl Pts',(-6.26233416579329,-24.1171659575934,
-10.4403841426424));
#41328=CARTESIAN_POINT('Ctrl Pts',(-6.01863411861028,-24.1283101330354,
-10.5865599069465));
#41329=CARTESIAN_POINT('Ctrl Pts',(-5.76979788477571,-24.1394543084775,
-10.7242087855524));
#41330=CARTESIAN_POINT('Ctrl Pts',(-5.51644430519778,-24.1505984839195,
-10.8529854177388));
#41331=CARTESIAN_POINT('Ctrl Pts',(-5.25511210174971,-24.1620936123039,
-10.9858174902043));
#41332=CARTESIAN_POINT('Ctrl Pts',(-4.9889736812031,-24.1735887406883,-11.1092093074788));
#41333=CARTESIAN_POINT('Ctrl Pts',(-4.71873469727067,-24.1850838690726,
-11.2228335596129));
#41334=CARTESIAN_POINT('Ctrl Pts',(-4.45673226505212,-24.196228640088,-11.3329946843513));
#41335=CARTESIAN_POINT('Ctrl Pts',(-4.19087578555295,-24.2073734111034,
-11.4339747257494));
#41336=CARTESIAN_POINT('Ctrl Pts',(-3.92182874309239,-24.2185181821189,
-11.5255242639914));
#41337=CARTESIAN_POINT('Ctrl Pts',(-3.64009468169887,-24.2301884891877,
-11.6213908566577));
#41338=CARTESIAN_POINT('Ctrl Pts',(-3.35486221345111,-24.2418587962565,
-11.7069160450841));
#41339=CARTESIAN_POINT('Ctrl Pts',(-3.06691227567061,-24.2535291033253,
-11.7818716400808));
#41340=CARTESIAN_POINT('Ctrl Pts',(-2.77896233789011,-24.2651994103942,
-11.8568272350776));
#41341=CARTESIAN_POINT('Ctrl Pts',(-2.48829525746922,-24.276869717463,-11.9212131606227));
#41342=CARTESIAN_POINT('Ctrl Pts',(-2.19570672218016,-24.2885400245318,
-11.9748620969167));
#41343=CARTESIAN_POINT('Ctrl Pts',(-1.91623044331381,-24.2996873307296,
-12.0261067742441));
#41344=CARTESIAN_POINT('Ctrl Pts',(-1.63491767399143,-24.3108346369273,
-12.0675709631649));
#41345=CARTESIAN_POINT('Ctrl Pts',(-1.35246828020352,-24.3219819431251,
-12.0991437631364));
#41346=CARTESIAN_POINT('Ctrl Pts',(-1.07006686043228,-24.3331273559534,
-12.1307112004694));
#41347=CARTESIAN_POINT('Ctrl Pts',(-0.786529466626631,-24.3442727687817,
-12.1523905734547));
#41348=CARTESIAN_POINT('Ctrl Pts',(-0.502562287985962,-24.35541818161,-12.1641227138127));
#41349=CARTESIAN_POINT('Ctrl Pts',(-0.21862663413152,-24.3665623571237,
-12.1758535517201));
#41350=CARTESIAN_POINT('Ctrl Pts',(0.065738442831518,-24.3777065326373,
-12.1776393510993));
#41351=CARTESIAN_POINT('Ctrl Pts',(0.349824290944202,-24.388850708151,-12.1694730048374));
#41352=CARTESIAN_POINT('Ctrl Pts',(0.642856581842261,-24.4003458364815,
-12.1610494836753));
#41353=CARTESIAN_POINT('Ctrl Pts',(0.935591475061994,-24.411840964812,-12.1420368316068));
#41354=CARTESIAN_POINT('Ctrl Pts',(1.22725272951179,-24.4233360931425,-12.1124853348892));
#41355=CARTESIAN_POINT('Ctrl Pts',(1.51002451090377,-24.4344808642279,-12.0838345311155));
#41356=CARTESIAN_POINT('Ctrl Pts',(1.79178685310204,-24.4456256353134,-12.0452778196724));
#41357=CARTESIAN_POINT('Ctrl Pts',(2.0718378161832,-24.4567704063989,-11.9969136995076));
#41358=CARTESIAN_POINT('Ctrl Pts',(2.36509468764143,-24.4684407133519,-11.9462689510864));
#41359=CARTESIAN_POINT('Ctrl Pts',(2.65647458170125,-24.4801110203049,-11.8848696481262));
#41360=CARTESIAN_POINT('Ctrl Pts',(2.9451825869511,-24.4917813272579,-11.812889137697));
#41361=CARTESIAN_POINT('Ctrl Pts',(3.23389059220094,-24.5034516342109,-11.7409086272678));
#41362=CARTESIAN_POINT('Ctrl Pts',(3.51992638522858,-24.5151219411639,-11.6583469990493));
#41363=CARTESIAN_POINT('Ctrl Pts',(3.80251123137941,-24.5267922481169,-11.5654381060656));
#41364=CARTESIAN_POINT('Ctrl Pts',(4.07242967029088,-24.5379394524956,-11.4766937034667));
#41365=CARTESIAN_POINT('Ctrl Pts',(4.33928034053855,-24.5490866568743,-11.3784827372588));
#41366=CARTESIAN_POINT('Ctrl Pts',(4.6023956623735,-24.5602338612531,-11.2710427386718));
#41367=CARTESIAN_POINT('Ctrl Pts',(4.86547585228003,-24.5713795772244,-11.163617085788));
#41368=CARTESIAN_POINT('Ctrl Pts',(5.12482144211058,-24.5825252931958,-11.0469649602304));
#41369=CARTESIAN_POINT('Ctrl Pts',(5.37978398500469,-24.5936710091671,-10.9213723736849));
#41370=CARTESIAN_POINT('Ctrl Pts',(5.6347135872906,-24.6048152851361,-10.7957960134295));
#41371=CARTESIAN_POINT('Ctrl Pts',(5.8852610344657,-24.6159595611051,-10.6612816171815));
#41372=CARTESIAN_POINT('Ctrl Pts',(6.13080066714201,-24.6271038370741,-10.5181620747054));
#41373=CARTESIAN_POINT('Ctrl Pts',(6.37634730179191,-24.6382484308407,-10.375038450936));
#41374=CARTESIAN_POINT('Ctrl Pts',(6.61688560493623,-24.6493930246074,-10.2233093229305));
#41375=CARTESIAN_POINT('Ctrl Pts',(6.85181594527438,-24.6605376183741,-10.0633527465792));
#41376=CARTESIAN_POINT('Ctrl Pts',(7.04258417037973,-24.6695872556807,-9.93346474607435));
#41377=CARTESIAN_POINT('Ctrl Pts',(7.22965507309842,-24.6786368929874,-9.79815263546583));
#41378=CARTESIAN_POINT('Ctrl Pts',(7.41272179941105,-24.687686530294,-9.65763976210214));
#41379=CARTESIAN_POINT('Ctrl Pts',(7.41324263166141,-21.6876995907947,-9.65831743152016));
#41380=CARTESIAN_POINT('Ctrl Pts',(8.88409813246325,-21.7604723234234,-8.52773514691198));
#41381=CARTESIAN_POINT('Ctrl Pts',(11.414685028869,-21.9126624639138,-5.45082711782888));
#41382=CARTESIAN_POINT('Ctrl Pts',(12.6811956770552,-22.1442700122659,0.50872888397338));
#41383=CARTESIAN_POINT('Ctrl Pts',(10.8914562364704,-22.382522235851,6.51518676137968));
#41384=CARTESIAN_POINT('Ctrl Pts',(6.4456037215397,-22.6207744594361,10.9327814560358));
#41385=CARTESIAN_POINT('Ctrl Pts',(0.427851551046576,-22.8590266830212,
12.6841806328137));
#41386=CARTESIAN_POINT('Ctrl Pts',(-5.69424089117864,-23.0972789066063,
11.3422716237698));
#41387=CARTESIAN_POINT('Ctrl Pts',(-10.4276708680614,-23.3355311301914,
7.23430593172712));
#41388=CARTESIAN_POINT('Ctrl Pts',(-12.0452929662932,-23.5114801626443,
2.89768759261325));
#41389=CARTESIAN_POINT('Ctrl Pts',(-12.1750513728812,-23.6080117872355,
0.436676266174656));
#41390=CARTESIAN_POINT('Ctrl Pts',(-12.1746001704992,-23.6251260039651,
0.000313053299986626));
#41391=CARTESIAN_POINT('Ctrl Pts',(7.93208051261574,-20.0005837734501,-6.87965285147223));
#41392=CARTESIAN_POINT('Ctrl Pts',(9.07668263151754,-20.0800217251941,-5.55995978932681));
#41393=CARTESIAN_POINT('Ctrl Pts',(10.6930139230921,-20.2388770847998,-2.33991560351307));
#41394=CARTESIAN_POINT('Ctrl Pts',(10.5082240576505,-20.4771498522672,3.06359191036739));
#41395=CARTESIAN_POINT('Ctrl Pts',(7.7610444220363,-20.7154020758523,7.71831352629605));
#41396=CARTESIAN_POINT('Ctrl Pts',(3.12105089944607,-20.9536542994374,10.4913407524211));
#41397=CARTESIAN_POINT('Ctrl Pts',(-2.28002032107308,-21.1919065230225,
10.7055409903604));
#41398=CARTESIAN_POINT('Ctrl Pts',(-7.12508829170954,-21.4301587466076,
8.30910926435329));
#41399=CARTESIAN_POINT('Ctrl Pts',(-10.2325364964883,-21.6684109701927,
3.88625151956404));
#41400=CARTESIAN_POINT('Ctrl Pts',(-10.8445684035224,-21.9066631937778,
-1.48431630400502));
#41401=CARTESIAN_POINT('Ctrl Pts',(-8.81191628458542,-22.1449154173629,
-6.49291954617506));
#41402=CARTESIAN_POINT('Ctrl Pts',(-4.63029122950666,-22.383167640948,-9.91807630779845));
#41403=CARTESIAN_POINT('Ctrl Pts',(0.680530483683632,-22.6214198645331,
-10.9245019479025));
#41404=CARTESIAN_POINT('Ctrl Pts',(5.82538981214024,-22.8596720881182,-9.26675138990805));
#41405=CARTESIAN_POINT('Ctrl Pts',(9.54960316733972,-23.0979243117033,-5.34910593878247));
#41406=CARTESIAN_POINT('Ctrl Pts',(10.9449409563647,-23.3361765352884,-0.126965784354505));
#41407=CARTESIAN_POINT('Ctrl Pts',(9.67112030848427,-23.5744287588735,5.12613742673736));
#41408=CARTESIAN_POINT('Ctrl Pts',(6.03878961601207,-23.8126809824586,9.12912226706514));
#41409=CARTESIAN_POINT('Ctrl Pts',(0.933770628914186,-24.0509332060437,
10.9057748640797));
#41410=CARTESIAN_POINT('Ctrl Pts',(-4.3989683509955,-24.2891854296288,10.0228204950036));
#41411=CARTESIAN_POINT('Ctrl Pts',(-8.65892458966233,-24.5274376532139,
6.69558646125051));
#41412=CARTESIAN_POINT('Ctrl Pts',(-10.8072164379082,-24.765689876799,1.7354901366115));
#41413=CARTESIAN_POINT('Ctrl Pts',(-10.3199368707579,-25.0039421003841,
-3.64784266760709));
#41414=CARTESIAN_POINT('Ctrl Pts',(-7.31591945824722,-25.2421943239692,
-8.14157083244356));
#41415=CARTESIAN_POINT('Ctrl Pts',(-2.52775824622543,-25.4804465475543,
-10.6498024110112));
#41416=CARTESIAN_POINT('Ctrl Pts',(2.8768510043701,-25.7186987711394,-10.5608513596116));
#41417=CARTESIAN_POINT('Ctrl Pts',(7.5798784633816,-25.9569509947245,-7.89641029984006));
#41418=CARTESIAN_POINT('Ctrl Pts',(10.4343900608802,-26.1952032183096,-3.30626030429192));
#41419=CARTESIAN_POINT('Ctrl Pts',(10.7442519485492,-26.4334554418947,2.09019214633302));
#41420=CARTESIAN_POINT('Ctrl Pts',(8.43389766221118,-26.6717076654798,6.97690643235821));
#41421=CARTESIAN_POINT('Ctrl Pts',(4.06675662420537,-26.9099598890649,10.1621525132199));
#41422=CARTESIAN_POINT('Ctrl Pts',(-1.29215020014935,-27.14821211265,10.8691398464998));
#41423=CARTESIAN_POINT('Ctrl Pts',(-6.33593849695176,-27.3864643362351,
8.92545441450063));
#41424=CARTESIAN_POINT('Ctrl Pts',(-9.83457236079029,-27.6247165598202,
4.80510557874393));
#41425=CARTESIAN_POINT('Ctrl Pts',(-10.934834919905,-27.8629687834053,-0.487071264723974));
#41426=CARTESIAN_POINT('Ctrl Pts',(-9.36840356171729,-28.1012210069904,
-5.66046533840602));
#41427=CARTESIAN_POINT('Ctrl Pts',(-5.51728615423312,-28.3394732305755,
-9.45343358969647));
#41428=CARTESIAN_POINT('Ctrl Pts',(-0.320660237907371,-28.5777254541606,
-10.9409793964854));
#41429=CARTESIAN_POINT('Ctrl Pts',(4.95416555177833,-28.8159776777457,-9.76033282363192));
#41430=CARTESIAN_POINT('Ctrl Pts',(9.02081186376675,-29.0542299013308,-6.1994198487454));
#41431=CARTESIAN_POINT('Ctrl Pts',(10.8875398137095,-29.2924821249159,-1.12664543996017));
#41432=CARTESIAN_POINT('Ctrl Pts',(10.0991077719128,-29.530734348501,4.22088561249689));
#41433=CARTESIAN_POINT('Ctrl Pts',(6.84779179425367,-29.7689865720861,8.53906322057902));
#41434=CARTESIAN_POINT('Ctrl Pts',(1.92649498392104,-30.0072387956712,10.7748072010324));
#41435=CARTESIAN_POINT('Ctrl Pts',(-3.46461892863269,-30.2454910192563,
10.3828834541207));
#41436=CARTESIAN_POINT('Ctrl Pts',(-8.0108112405926,-30.4837432428414,7.45887098762869));
#41437=CARTESIAN_POINT('Ctrl Pts',(-10.6033954949622,-30.7219954664265,
2.71585292678186));
#41438=CARTESIAN_POINT('Ctrl Pts',(-10.6101144412331,-30.9602476900116,
-2.68948409298712));
#41439=CARTESIAN_POINT('Ctrl Pts',(-8.02932952031574,-31.1984999135967,
-7.43893275925249));
#41440=CARTESIAN_POINT('Ctrl Pts',(-3.49042046230085,-31.4367521371818,
-10.3742381955904));
#41441=CARTESIAN_POINT('Ctrl Pts',(1.89970245342874,-31.6750043607669,-10.7795632439784));
#41442=CARTESIAN_POINT('Ctrl Pts',(6.8265421998787,-31.913256584352,-8.55606070196843));
#41443=CARTESIAN_POINT('Ctrl Pts',(10.0885832827944,-32.1515088079371,-4.24597933209919));
#41444=CARTESIAN_POINT('Ctrl Pts',(10.8903070521443,-32.3897610315222,1.09957512363163));
#41445=CARTESIAN_POINT('Ctrl Pts',(9.03619597933803,-32.6280132551074,6.1769746126635));
#41446=CARTESIAN_POINT('Ctrl Pts',(4.97841479809776,-32.8662654786924,9.7479864197984));
#41447=CARTESIAN_POINT('Ctrl Pts',(-0.293459559412273,-33.1045177022776,
10.9417427601586));
#41448=CARTESIAN_POINT('Ctrl Pts',(-5.49376751214475,-33.3427699258626,
9.46712055827954));
#41449=CARTESIAN_POINT('Ctrl Pts',(-9.35430248110292,-33.5810221494478,
5.68373805118744));
#41450=CARTESIAN_POINT('Ctrl Pts',(-10.9335902515748,-33.8192743730328,
0.514254171769246));
#41451=CARTESIAN_POINT('Ctrl Pts',(-9.84648764379592,-34.0575265966179,
-4.78064161206769));
#41452=CARTESIAN_POINT('Ctrl Pts',(-6.35810793409936,-34.295778820203,-8.90967545092837));
#41453=CARTESIAN_POINT('Ctrl Pts',(-1.3191672989035,-34.5340310437881,-10.8658939245695));
#41454=CARTESIAN_POINT('Ctrl Pts',(4.04148056253829,-34.7722832673732,-10.1722312205807));
#41455=CARTESIAN_POINT('Ctrl Pts',(8.41652674720532,-35.0105354909583,-6.9978518601521));
#41456=CARTESIAN_POINT('Ctrl Pts',(10.7390224500958,-35.2487877145434,-2.11689630296171));
#41457=CARTESIAN_POINT('Ctrl Pts',(10.4425773045532,-35.4870399381285,3.28030979990781));
#41458=CARTESIAN_POINT('Ctrl Pts',(7.59948581375965,-35.7252921617136,7.87754203452586));
#41459=CARTESIAN_POINT('Ctrl Pts',(2.90309678978814,-35.9635443852987,10.5536667643604));
#41460=CARTESIAN_POINT('Ctrl Pts',(-2.50127462534687,-36.2017966088839,
10.6560536034062));
#41461=CARTESIAN_POINT('Ctrl Pts',(-7.29565659631146,-36.4400488324689,
8.15973332519128));
#41462=CARTESIAN_POINT('Ctrl Pts',(-10.310836309689,-36.678301056054,3.67348714751024));
#41463=CARTESIAN_POINT('Ctrl Pts',(-10.811497527272,-36.9165532796391,-1.70861762580354));
#41464=CARTESIAN_POINT('Ctrl Pts',(-8.67554332886272,-37.1548055032242,
-6.67403935727874));
#41465=CARTESIAN_POINT('Ctrl Pts',(-4.42387183430699,-37.3930577268093,
-10.0118535213315));
#41466=CARTESIAN_POINT('Ctrl Pts',(0.906655509484174,-37.6313099503944,
-10.9080625518847));
#41467=CARTESIAN_POINT('Ctrl Pts',(6.01607574523276,-37.8695621739795,-9.14410671556304));
#41468=CARTESIAN_POINT('Ctrl Pts',(9.65834638546719,-38.1078143975646,-5.15016435505535));
#41469=CARTESIAN_POINT('Ctrl Pts',(10.9452233105833,-38.3460666211498,0.0997558540279738));
#41470=CARTESIAN_POINT('Ctrl Pts',(9.56287066352807,-38.5843188447348,5.32534873881454));
#41471=CARTESIAN_POINT('Ctrl Pts',(5.84841145753923,-38.82257106832,9.25224060771052));
#41472=CARTESIAN_POINT('Ctrl Pts',(0.70768278248567,-39.060823291905,10.9227763791256));
#41473=CARTESIAN_POINT('Ctrl Pts',(-4.60561153353682,-39.2990755154902,
9.92955670850569));
#41474=CARTESIAN_POINT('Ctrl Pts',(-8.79576482446728,-39.5373277390752,
6.51480629675831));
#41475=CARTESIAN_POINT('Ctrl Pts',(-10.8408098726847,-39.7755799626604,
1.51127160533644));
#41476=CARTESIAN_POINT('Ctrl Pts',(-10.2422364118163,-40.0138321862454,
-3.86080079579494));
#41477=CARTESIAN_POINT('Ctrl Pts',(-7.14558203450444,-40.2520844098305,
-8.29137091192963));
#41478=CARTESIAN_POINT('Ctrl Pts',(-2.30691296609827,-40.4903366334156,
-10.6998374196014));
#41479=CARTESIAN_POINT('Ctrl Pts',(3.09555850011698,-40.7285888570008,-10.4990832245953));
#41480=CARTESIAN_POINT('Ctrl Pts',(6.19188889114854,-40.8874236727241,-8.65783810040184));
#41481=CARTESIAN_POINT('Ctrl Pts',(7.42649694513297,-40.9668410805858,-7.4225782431051));
#41482=CARTESIAN_POINT('Ctrl Pts',(8.35397305039485,-19.6781514844946,-7.24556872889312));
#41483=CARTESIAN_POINT('Ctrl Pts',(9.5594544167933,-19.7575894362386,-5.8556836592167));
#41484=CARTESIAN_POINT('Ctrl Pts',(11.2617553489193,-19.9164447958441,-2.46437134127127));
#41485=CARTESIAN_POINT('Ctrl Pts',(11.0671368558985,-20.1547175633116,3.22653863837005));
#41486=CARTESIAN_POINT('Ctrl Pts',(8.17383986981593,-20.3929697868966,8.12883619759329));
#41487=CARTESIAN_POINT('Ctrl Pts',(3.28705376368968,-20.6312220104818,11.0493555592179));
#41488=CARTESIAN_POINT('Ctrl Pts',(-2.40129034069979,-20.8694742340669,
11.2749487074831));
#41489=CARTESIAN_POINT('Ctrl Pts',(-7.5040584214893,-21.107726457652,8.75105525678824));
#41490=CARTESIAN_POINT('Ctrl Pts',(-10.776785988605,-21.345978681237,4.0929539746676));
#41491=CARTESIAN_POINT('Ctrl Pts',(-11.4213707289154,-21.5842309048222,
-1.5632643140974));
#41492=CARTESIAN_POINT('Ctrl Pts',(-9.28060564270375,-21.8224831284072,
-6.83826580187362));
#41493=CARTESIAN_POINT('Ctrl Pts',(-4.87656776620671,-22.0607353519924,
-10.4456002501902));
#41494=CARTESIAN_POINT('Ctrl Pts',(0.716726628231168,-22.2989875755774,
-11.505555789129));
#41495=CARTESIAN_POINT('Ctrl Pts',(6.13523140886729,-22.5372397991626,-9.75963257721301));
#41496=CARTESIAN_POINT('Ctrl Pts',(10.0575287120496,-22.7754920227476,-5.63361488643787));
#41497=CARTESIAN_POINT('Ctrl Pts',(11.5270819102518,-23.0137442463328,-0.133718857131222));
#41498=CARTESIAN_POINT('Ctrl Pts',(10.1855091228218,-23.2519964699178,5.39878709595479));
#41499=CARTESIAN_POINT('Ctrl Pts',(6.35998154947282,-23.490248693503,9.61468321854845));
#41500=CARTESIAN_POINT('Ctrl Pts',(0.983436143492576,-23.7285009170881,
11.4858326467177));
#41501=CARTESIAN_POINT('Ctrl Pts',(-4.63294125611917,-23.9667531406732,
10.5559155849508));
#41502=CARTESIAN_POINT('Ctrl Pts',(-9.119476605462,-24.2050053642583,7.05171219138697));
#41503=CARTESIAN_POINT('Ctrl Pts',(-11.3820320820593,-24.4432575878434,
1.82779761342809));
#41504=CARTESIAN_POINT('Ctrl Pts',(-10.868835025435,-24.6815098114284,-3.84186460145004));
#41505=CARTESIAN_POINT('Ctrl Pts',(-7.70503954112061,-24.9197620350136,
-8.57460576880672));
#41506=CARTESIAN_POINT('Ctrl Pts',(-2.66220498308041,-25.1580142585986,
-11.216245497271));
#41507=CARTESIAN_POINT('Ctrl Pts',(3.02986533259278,-25.3962664821838,-11.1225633056928));
#41508=CARTESIAN_POINT('Ctrl Pts',(7.98303803241107,-25.6345187057688,-8.31640560566758));
#41509=CARTESIAN_POINT('Ctrl Pts',(10.9893757668322,-25.872770929354,-3.48211411063157));
#41510=CARTESIAN_POINT('Ctrl Pts',(11.3157186291889,-26.1110231529391,2.20136556012525));
#41511=CARTESIAN_POINT('Ctrl Pts',(8.88248091630454,-26.3492753765242,7.34799504598405));
#41512=CARTESIAN_POINT('Ctrl Pts',(4.28305980846921,-26.5875276001093,10.702658412811));
#41513=CARTESIAN_POINT('Ctrl Pts',(-1.3608772543271,-26.8257798236944,11.4472490810218));
#41514=CARTESIAN_POINT('Ctrl Pts',(-6.67293522403238,-27.0640320472795,
9.4001826535517));
#41515=CARTESIAN_POINT('Ctrl Pts',(-10.3576548843057,-27.3022842708645,
5.06068016396008));
#41516=CARTESIAN_POINT('Ctrl Pts',(-11.5164383526005,-27.5405364944497,
-0.512977674981265));
#41517=CARTESIAN_POINT('Ctrl Pts',(-9.86669143805761,-27.7787887180348,
-5.96153491061126));
#41518=CARTESIAN_POINT('Ctrl Pts',(-5.8107402932274,-28.0170409416198,-9.95624405430786));
#41519=CARTESIAN_POINT('Ctrl Pts',(-0.337715556662699,-28.255293165205,
-11.5229096424065));
#41520=CARTESIAN_POINT('Ctrl Pts',(5.21766835837407,-28.49354538879,-10.2794666849161));
#41521=CARTESIAN_POINT('Ctrl Pts',(9.50061198732568,-28.7317976123752,-6.52915540407486));
#41522=CARTESIAN_POINT('Ctrl Pts',(11.4666277080989,-28.9700498359603,-1.1865696052641));
#41523=CARTESIAN_POINT('Ctrl Pts',(10.6362604395415,-29.2083020595454,4.44538662958811));
#41524=CARTESIAN_POINT('Ctrl Pts',(7.21201304158794,-29.4465542831305,8.99324003417244));
#41525=CARTESIAN_POINT('Ctrl Pts',(2.02896165158692,-29.6848065067157,11.3478990584454));
#41526=CARTESIAN_POINT('Ctrl Pts',(-3.64889553423618,-29.9230587303007,
10.9351296199225));
#41527=CARTESIAN_POINT('Ctrl Pts',(-8.43689131864875,-30.1613109538859,
7.85559439518017));
#41528=CARTESIAN_POINT('Ctrl Pts',(-11.1673702840897,-30.3995631774709,
2.86030406815548));
#41529=CARTESIAN_POINT('Ctrl Pts',(-11.1744465985554,-30.637815401056,-2.83253272537331));
#41530=CARTESIAN_POINT('Ctrl Pts',(-8.45639455106058,-30.8760676246411,
-7.83459568970025));
#41531=CARTESIAN_POINT('Ctrl Pts',(-3.67606940325828,-31.1143198482261,
-10.9260245362485));
#41532=CARTESIAN_POINT('Ctrl Pts',(2.00074407647172,-31.3525720718113,-11.3529080664269));
#41533=CARTESIAN_POINT('Ctrl Pts',(7.18963322100266,-31.5908242953964,-9.01114157982946));
#41534=CARTESIAN_POINT('Ctrl Pts',(10.6251761725167,-31.8290765189815,-4.47181503723706));
#41535=CARTESIAN_POINT('Ctrl Pts',(11.4695421307741,-32.0673287425667,1.15805946940319));
#41536=CARTESIAN_POINT('Ctrl Pts',(9.51681435525202,-32.3055809661518,6.50551634783486));
#41537=CARTESIAN_POINT('Ctrl Pts',(5.24320737678452,-32.5438331897368,10.2664635989375));
#41538=CARTESIAN_POINT('Ctrl Pts',(-0.309068124915233,-32.7820854133219,
11.5237136079667));
#41539=CARTESIAN_POINT('Ctrl Pts',(-5.78597073852161,-33.0203376369069,
9.97065900716958));
#41540=CARTESIAN_POINT('Ctrl Pts',(-9.85184034731961,-33.2585898604922,
5.98604545548992));
#41541=CARTESIAN_POINT('Ctrl Pts',(-11.515127482688,-33.4968420840772,0.541606390048691));
#41542=CARTESIAN_POINT('Ctrl Pts',(-10.3702039189452,-33.7350943076624,
-5.03491500461833));
#41543=CARTESIAN_POINT('Ctrl Pts',(-6.69628381210821,-33.9733465312474,
-9.38356443639719));
#41544=CARTESIAN_POINT('Ctrl Pts',(-1.3893313420703,-34.2115987548325,-11.4438305145706));
#41545=CARTESIAN_POINT('Ctrl Pts',(4.25643936032185,-34.4498509784176,-10.7132731877799));
#41546=CARTESIAN_POINT('Ctrl Pts',(8.8641860747949,-34.6881032020028,-7.37005452193625));
#41547=CARTESIAN_POINT('Ctrl Pts',(11.3102109834865,-34.9263554255878,-2.22949006093621));
#41548=CARTESIAN_POINT('Ctrl Pts',(10.9979984746946,-35.1646076491729,3.45478334741955));
#41549=CARTESIAN_POINT('Ctrl Pts',(8.00368826111052,-35.402859872758,8.29653377258524));
#41550=CARTESIAN_POINT('Ctrl Pts',(3.05750708228506,-35.6411120963432,11.114996575248));
#41551=CARTESIAN_POINT('Ctrl Pts',(-2.63431274790397,-35.8793643199282,
11.2228291789063));
#41552=CARTESIAN_POINT('Ctrl Pts',(-7.68369893542883,-36.1176165435133,
8.59373429059882));
#41553=CARTESIAN_POINT('Ctrl Pts',(-10.8592504225313,-36.3558687670984,
3.86887306331091));
#41554=CARTESIAN_POINT('Ctrl Pts',(-11.3865408745652,-36.5941209906835,
-1.79949580399373));
#41555=CARTESIAN_POINT('Ctrl Pts',(-9.13697926434082,-36.8323732142686,
-7.02901903722545));
#41556=CARTESIAN_POINT('Ctrl Pts',(-4.65916930916454,-37.0706254378537,
-10.544365298446));
#41557=CARTESIAN_POINT('Ctrl Pts',(0.954878821536958,-37.3088776614388,
-11.4882420123614));
#41558=CARTESIAN_POINT('Ctrl Pts',(6.33605957035795,-37.5471298850239,-9.63046466185671));
#41559=CARTESIAN_POINT('Ctrl Pts',(10.1720557787132,-37.785382108609,-5.42409197168482));
#41560=CARTESIAN_POINT('Ctrl Pts',(11.5273792823635,-38.0236343321941,0.105061681464705));
#41561=CARTESIAN_POINT('Ctrl Pts',(10.0715018815638,-38.2618865557792,5.60859408540474));
#41562=CARTESIAN_POINT('Ctrl Pts',(6.15947753255869,-38.5001387793643,9.74434999363035));
#41563=CARTESIAN_POINT('Ctrl Pts',(0.74532310706011,-38.7383910029494,11.5037384405739));
#41564=CARTESIAN_POINT('Ctrl Pts',(-4.85057540333342,-38.9766432265345,
10.4576912719547));
#41565=CARTESIAN_POINT('Ctrl Pts',(-9.26359511660826,-39.2148954501196,
6.86131666781508));
#41566=CARTESIAN_POINT('Ctrl Pts',(-11.4174122888469,-39.4531476737047,
1.59165331752844));
#41567=CARTESIAN_POINT('Ctrl Pts',(-10.7870018243007,-39.6913998972898,
-4.06614957446744));
#41568=CARTESIAN_POINT('Ctrl Pts',(-7.52564218816163,-39.9296521208749,
-8.73237343455132));
#41569=CARTESIAN_POINT('Ctrl Pts',(-2.42961335525277,-40.16790434446,-11.268941774455));
#41570=CARTESIAN_POINT('Ctrl Pts',(3.26020547128437,-40.4061565680451,-11.0575098390168));
#41571=CARTESIAN_POINT('Ctrl Pts',(6.52122388891844,-40.5649913837685,-9.11833232786835));
#41572=CARTESIAN_POINT('Ctrl Pts',(7.82149843786967,-40.6444087916302,-7.81737130740481));
#41573=CARTESIAN_POINT('Ctrl Pts',(8.77586558817396,-19.3557191955389,-7.61148460631401));
#41574=CARTESIAN_POINT('Ctrl Pts',(10.0422262020691,-19.4351571472829,-6.15140752910658));
#41575=CARTESIAN_POINT('Ctrl Pts',(11.8304967747464,-19.5940125068886,-2.58882707902948));
#41576=CARTESIAN_POINT('Ctrl Pts',(11.6260496541463,-19.832285274356,3.38948536637273));
#41577=CARTESIAN_POINT('Ctrl Pts',(8.58663531759557,-20.0705374979411,8.53935886889055));
#41578=CARTESIAN_POINT('Ctrl Pts',(3.45305662793327,-20.3087897215262,11.6073703660148));
#41579=CARTESIAN_POINT('Ctrl Pts',(-2.52256036032647,-20.5470419451113,
11.8443564246056));
#41580=CARTESIAN_POINT('Ctrl Pts',(-7.8830285512691,-20.7852941686964,9.1930012492232));
#41581=CARTESIAN_POINT('Ctrl Pts',(-11.3210354807218,-21.0235463922815,
4.29965642977116));
#41582=CARTESIAN_POINT('Ctrl Pts',(-11.9981730543084,-21.2617986158666,
-1.64221232418978));
#41583=CARTESIAN_POINT('Ctrl Pts',(-9.74929500082207,-21.5000508394517,
-7.18361205757219));
#41584=CARTESIAN_POINT('Ctrl Pts',(-5.12284430290676,-21.7383030630368,
-10.973124192582));
#41585=CARTESIAN_POINT('Ctrl Pts',(0.752922772778706,-21.9765552866219,
-12.0866096303555));
#41586=CARTESIAN_POINT('Ctrl Pts',(6.44507300559435,-22.214807510207,-10.2525137645179));
#41587=CARTESIAN_POINT('Ctrl Pts',(10.5654542567593,-22.4530597337921,-5.91812383409328));
#41588=CARTESIAN_POINT('Ctrl Pts',(12.1092228641389,-22.6913119573772,-0.140471929907933));
#41589=CARTESIAN_POINT('Ctrl Pts',(10.6998979371592,-22.9295641809623,5.67143676517222));
#41590=CARTESIAN_POINT('Ctrl Pts',(6.6811734829336,-23.1678164045474,10.1002441700318));
#41591=CARTESIAN_POINT('Ctrl Pts',(1.03310165807095,-23.4060686281325,12.0658904293558));
#41592=CARTESIAN_POINT('Ctrl Pts',(-4.86691416124282,-23.6443208517176,
11.089010674898));
#41593=CARTESIAN_POINT('Ctrl Pts',(-9.58002862126169,-23.8825730753027,
7.40783792152343));
#41594=CARTESIAN_POINT('Ctrl Pts',(-11.9568477262104,-24.1208252988878,
1.92010509024468));
#41595=CARTESIAN_POINT('Ctrl Pts',(-11.4177331801119,-24.3590775224729,
-4.03588653529299));
#41596=CARTESIAN_POINT('Ctrl Pts',(-8.094159623994,-24.597329746058,-9.00764070516989));
#41597=CARTESIAN_POINT('Ctrl Pts',(-2.79665171993538,-24.8355819696431,
-11.7826885835309));
#41598=CARTESIAN_POINT('Ctrl Pts',(3.18287966081545,-25.0738341932282,-11.6842752517741));
#41599=CARTESIAN_POINT('Ctrl Pts',(8.38619760144056,-25.3120864168133,-8.73640091149512));
#41600=CARTESIAN_POINT('Ctrl Pts',(11.5443614727842,-25.5503386403984,-3.65796791697122));
#41601=CARTESIAN_POINT('Ctrl Pts',(11.8871853098286,-25.7885908639836,2.3125389739175));
#41602=CARTESIAN_POINT('Ctrl Pts',(9.33106417039787,-26.0268430875686,7.71908365960986));
#41603=CARTESIAN_POINT('Ctrl Pts',(4.49936299273306,-26.2650953111537,11.2431643124021));
#41604=CARTESIAN_POINT('Ctrl Pts',(-1.42960430850484,-26.5033475347388,
12.0253583155439));
#41605=CARTESIAN_POINT('Ctrl Pts',(-7.00993195111297,-26.7415997583239,
9.87491089260277));
#41606=CARTESIAN_POINT('Ctrl Pts',(-10.880737407821,-26.979851981909,5.31625474917623));
#41607=CARTESIAN_POINT('Ctrl Pts',(-12.098041785296,-27.2181042054941,-0.538884085238557));
#41608=CARTESIAN_POINT('Ctrl Pts',(-10.3649793143979,-27.4563564290792,
-6.26260448281651));
#41609=CARTESIAN_POINT('Ctrl Pts',(-6.10419443222168,-27.6946086526643,
-10.4590545189192));
#41610=CARTESIAN_POINT('Ctrl Pts',(-0.354770875418025,-27.9328608762494,
-12.1048398883276));
#41611=CARTESIAN_POINT('Ctrl Pts',(5.4811711649698,-28.1711130998345,-10.7986005462002));
#41612=CARTESIAN_POINT('Ctrl Pts',(9.98041211088462,-28.4093653234196,-6.85889095940433));
#41613=CARTESIAN_POINT('Ctrl Pts',(12.0457156024881,-28.6476175470047,-1.24649377056803));
#41614=CARTESIAN_POINT('Ctrl Pts',(11.1734131071702,-28.8858697705898,4.66988764667932));
#41615=CARTESIAN_POINT('Ctrl Pts',(7.57623428892219,-29.1241219941749,9.44741684776586));
#41616=CARTESIAN_POINT('Ctrl Pts',(2.13142831925279,-29.36237421776,11.9209909158584));
#41617=CARTESIAN_POINT('Ctrl Pts',(-3.83317213983967,-29.6006264413451,
11.4873757857244));
#41618=CARTESIAN_POINT('Ctrl Pts',(-8.86297139670491,-29.8388786649302,
8.25231780273166));
#41619=CARTESIAN_POINT('Ctrl Pts',(-11.7313450732173,-30.0771308885153,
3.00475520952911));
#41620=CARTESIAN_POINT('Ctrl Pts',(-11.7387787558777,-30.3153831121004,
-2.97558135775951));
#41621=CARTESIAN_POINT('Ctrl Pts',(-8.88345958180541,-30.5536353356855,
-8.23025862014802));
#41622=CARTESIAN_POINT('Ctrl Pts',(-3.86171834421572,-30.7918875592706,
-11.4778108769068));
#41623=CARTESIAN_POINT('Ctrl Pts',(2.10178569951469,-31.0301397828557,-11.9262528888754));
#41624=CARTESIAN_POINT('Ctrl Pts',(7.55272424212662,-31.2683920064408,-9.46622245769049));
#41625=CARTESIAN_POINT('Ctrl Pts',(11.1617690622389,-31.5066442300259,-4.69765074237494));
#41626=CARTESIAN_POINT('Ctrl Pts',(12.0487772094039,-31.744896453611,1.21654381517477));
#41627=CARTESIAN_POINT('Ctrl Pts',(9.99743273116598,-31.9831486771961,6.83405808300621));
#41628=CARTESIAN_POINT('Ctrl Pts',(5.50799995547128,-32.2214009007812,10.7849407780765));
#41629=CARTESIAN_POINT('Ctrl Pts',(-0.324676690418206,-32.4596531243664,
12.1056844557749));
#41630=CARTESIAN_POINT('Ctrl Pts',(-6.07817396489844,-32.6979053479514,
10.4741974560597));
#41631=CARTESIAN_POINT('Ctrl Pts',(-10.3493782135363,-32.9361575715365,
6.28835285979241));
#41632=CARTESIAN_POINT('Ctrl Pts',(-12.0966647138013,-33.1744097951216,
0.568958608328141));
#41633=CARTESIAN_POINT('Ctrl Pts',(-10.8939201940946,-33.4126620187067,
-5.28918839716898));
#41634=CARTESIAN_POINT('Ctrl Pts',(-7.03445969011705,-33.6509142422919,
-9.85745342186599));
#41635=CARTESIAN_POINT('Ctrl Pts',(-1.45949538523709,-33.8891664658769,
-12.0217671045718));
#41636=CARTESIAN_POINT('Ctrl Pts',(4.4713981581054,-34.127418689462,-11.2543151549789));
#41637=CARTESIAN_POINT('Ctrl Pts',(9.31184540238453,-34.3656709130471,-7.7422571837204));
#41638=CARTESIAN_POINT('Ctrl Pts',(11.8813995168772,-34.6039231366322,-2.34208381891072));
#41639=CARTESIAN_POINT('Ctrl Pts',(11.5534196448359,-34.8421753602173,3.62925689493129));
#41640=CARTESIAN_POINT('Ctrl Pts',(8.4078907084614,-35.0804275838025,8.71552551064461));
#41641=CARTESIAN_POINT('Ctrl Pts',(3.21191737478198,-35.3186798073875,11.6763263861354));
#41642=CARTESIAN_POINT('Ctrl Pts',(-2.76735087046105,-35.5569320309727,
11.7896047544065));
#41643=CARTESIAN_POINT('Ctrl Pts',(-8.0717412745462,-35.7951842545577,9.0277352560064));
#41644=CARTESIAN_POINT('Ctrl Pts',(-11.4076645353736,-36.0334364781429,
4.06425897911157));
#41645=CARTESIAN_POINT('Ctrl Pts',(-11.9615842218583,-36.2716887017279,
-1.89037398218391));
#41646=CARTESIAN_POINT('Ctrl Pts',(-9.59841519981894,-36.5099409253131,
-7.38399871717217));
#41647=CARTESIAN_POINT('Ctrl Pts',(-4.89446678402209,-36.7481931488981,
-11.0768770755603));
#41648=CARTESIAN_POINT('Ctrl Pts',(1.00310213358974,-36.9864453724833,-12.0684214728383));
#41649=CARTESIAN_POINT('Ctrl Pts',(6.65604339548311,-37.2246975960683,-10.1168226081503));
#41650=CARTESIAN_POINT('Ctrl Pts',(10.6857651719592,-37.4629498196534,-5.69801958831428));
#41651=CARTESIAN_POINT('Ctrl Pts',(12.1095352541438,-37.7012020432385,0.110367508901437));
#41652=CARTESIAN_POINT('Ctrl Pts',(10.5801330995995,-37.9394542668236,5.89183943199494));
#41653=CARTESIAN_POINT('Ctrl Pts',(6.47054360757812,-38.1777064904088,10.2364593795502));
#41654=CARTESIAN_POINT('Ctrl Pts',(0.782963431634552,-38.4159587139938,
12.0847005020222));
#41655=CARTESIAN_POINT('Ctrl Pts',(-5.09553927313002,-38.654210937579,10.9858258354038));
#41656=CARTESIAN_POINT('Ctrl Pts',(-9.73142540874922,-38.892463161164,7.20782703887185));
#41657=CARTESIAN_POINT('Ctrl Pts',(-11.9940147050091,-39.1307153847492,
1.67203502972045));
#41658=CARTESIAN_POINT('Ctrl Pts',(-11.3317672367851,-39.3689676083343,
-4.27149835313993));
#41659=CARTESIAN_POINT('Ctrl Pts',(-7.9057023418188,-39.6072198319193,-9.17337595717302));
#41660=CARTESIAN_POINT('Ctrl Pts',(-2.55231374440726,-39.8454720555045,
-11.8380461293086));
#41661=CARTESIAN_POINT('Ctrl Pts',(3.42485244245177,-40.0837242790895,-11.6159364534383));
#41662=CARTESIAN_POINT('Ctrl Pts',(6.85055888668833,-40.2425590948129,-9.57882655533487));
#41663=CARTESIAN_POINT('Ctrl Pts',(8.21649993060639,-40.3219765026746,-8.21216437170453));
#41664=CARTESIAN_POINT('Ctrl Pts',(9.19775812595307,-19.0332869065834,-7.9774004837349));
#41665=CARTESIAN_POINT('Ctrl Pts',(10.5249979873448,-19.1127248583274,-6.44713139899647));
#41666=CARTESIAN_POINT('Ctrl Pts',(12.3992382005735,-19.2715802179331,-2.71328281678768));
#41667=CARTESIAN_POINT('Ctrl Pts',(12.1849624523942,-19.5098529854005,3.5524320943754));
#41668=CARTESIAN_POINT('Ctrl Pts',(8.99943076537519,-19.7481052089856,8.94988154018779));
#41669=CARTESIAN_POINT('Ctrl Pts',(3.61905949217688,-19.9863574325707,12.1653851728116));
#41670=CARTESIAN_POINT('Ctrl Pts',(-2.64383037995317,-20.2246096561558,
12.4137641417282));
#41671=CARTESIAN_POINT('Ctrl Pts',(-8.26199868104885,-20.4628618797409,
9.63494724165815));
#41672=CARTESIAN_POINT('Ctrl Pts',(-11.8652849728387,-20.701114103326,4.50635888487473));
#41673=CARTESIAN_POINT('Ctrl Pts',(-12.5749753797014,-20.9393663269111,
-1.72116033428216));
#41674=CARTESIAN_POINT('Ctrl Pts',(-10.2179843589404,-21.1776185504962,
-7.52895831327075));
#41675=CARTESIAN_POINT('Ctrl Pts',(-5.36912083960681,-21.4158707740812,
-11.5006481349737));
#41676=CARTESIAN_POINT('Ctrl Pts',(0.789118917326245,-21.6541229976664,
-12.6676634715821));
#41677=CARTESIAN_POINT('Ctrl Pts',(6.7549146023214,-21.8923752212515,-10.7453949518229));
#41678=CARTESIAN_POINT('Ctrl Pts',(11.0733798014692,-22.1306274448366,-6.20263278174869));
#41679=CARTESIAN_POINT('Ctrl Pts',(12.6913638180259,-22.3688796684217,-0.147225002684643));
#41680=CARTESIAN_POINT('Ctrl Pts',(11.2142867514966,-22.6071318920068,5.94408643438964));
#41681=CARTESIAN_POINT('Ctrl Pts',(7.00236541639435,-22.8453841155919,10.585805121515));
#41682=CARTESIAN_POINT('Ctrl Pts',(1.08276717264934,-23.083636339177,12.6459482119938));
#41683=CARTESIAN_POINT('Ctrl Pts',(-5.10088706636648,-23.3218885627621,
11.6221057648454));
#41684=CARTESIAN_POINT('Ctrl Pts',(-10.0405806370614,-23.5601407863472,
7.76396365165987));
#41685=CARTESIAN_POINT('Ctrl Pts',(-12.5316633703614,-23.7983930099322,
2.01241256706129));
#41686=CARTESIAN_POINT('Ctrl Pts',(-11.966631334789,-24.0366452335174,-4.22990846913594));
#41687=CARTESIAN_POINT('Ctrl Pts',(-8.48327970686742,-24.2748974571024,
-9.44067564153303));
#41688=CARTESIAN_POINT('Ctrl Pts',(-2.93109845679036,-24.5131496806876,
-12.3491316697907));
#41689=CARTESIAN_POINT('Ctrl Pts',(3.33589398903813,-24.7514019042726,-12.2459871978553));
#41690=CARTESIAN_POINT('Ctrl Pts',(8.78935717047004,-24.9896541278578,-9.15639621732265));
#41691=CARTESIAN_POINT('Ctrl Pts',(12.0993471787362,-25.2279063514429,-3.83382172331087));
#41692=CARTESIAN_POINT('Ctrl Pts',(12.4586519904683,-25.466158575028,2.42371238770974));
#41693=CARTESIAN_POINT('Ctrl Pts',(9.77964742449122,-25.7044107986131,8.09017227323569));
#41694=CARTESIAN_POINT('Ctrl Pts',(4.71566617699691,-25.9426630221981,11.7836702119933));
#41695=CARTESIAN_POINT('Ctrl Pts',(-1.49833136268259,-26.1809152457833,
12.603467550066));
#41696=CARTESIAN_POINT('Ctrl Pts',(-7.34692867819358,-26.4191674693684,
10.3496391316539));
#41697=CARTESIAN_POINT('Ctrl Pts',(-11.4038199313364,-26.6574196929535,
5.57182933439236));
#41698=CARTESIAN_POINT('Ctrl Pts',(-12.6796452179915,-26.8956719165386,
-0.564790495495845));
#41699=CARTESIAN_POINT('Ctrl Pts',(-10.8632671907382,-27.1339241401237,
-6.56367405502175));
#41700=CARTESIAN_POINT('Ctrl Pts',(-6.39764857121597,-27.3721763637088,
-10.9618649835306));
#41701=CARTESIAN_POINT('Ctrl Pts',(-0.371826194173351,-27.6104285872939,
-12.6867701342486));
#41702=CARTESIAN_POINT('Ctrl Pts',(5.74467397156553,-27.848680810879,-11.3177344074843));
#41703=CARTESIAN_POINT('Ctrl Pts',(10.4602122344436,-28.0869330344641,-7.1886265147338));
#41704=CARTESIAN_POINT('Ctrl Pts',(12.6248034968774,-28.3251852580492,-1.30641793587195));
#41705=CARTESIAN_POINT('Ctrl Pts',(11.7105657747989,-28.5634374816343,4.89438866377053));
#41706=CARTESIAN_POINT('Ctrl Pts',(7.94045553625644,-28.8016897052194,9.90159366135931));
#41707=CARTESIAN_POINT('Ctrl Pts',(2.23389498691868,-29.0399419288045,12.4940827732714));
#41708=CARTESIAN_POINT('Ctrl Pts',(-4.01744874544316,-29.2781941523896,
12.0396219515263));
#41709=CARTESIAN_POINT('Ctrl Pts',(-9.28905147476106,-29.5164463759747,
8.64904121028314));
#41710=CARTESIAN_POINT('Ctrl Pts',(-12.2953198623448,-29.7546985995598,
3.14920635090273));
#41711=CARTESIAN_POINT('Ctrl Pts',(-12.3031109132,-29.9929508231448,-3.1186299901457));
#41712=CARTESIAN_POINT('Ctrl Pts',(-9.31052461255024,-30.23120304673,-8.62592155059579));
#41713=CARTESIAN_POINT('Ctrl Pts',(-4.04736728517316,-30.4694552703151,
-12.0295972175649));
#41714=CARTESIAN_POINT('Ctrl Pts',(2.20282732255767,-30.7077074939002,-12.4995977113237));
#41715=CARTESIAN_POINT('Ctrl Pts',(7.91581526325055,-30.9459597174853,-9.92130333555153));
#41716=CARTESIAN_POINT('Ctrl Pts',(11.6983619519613,-31.1842119410704,-4.92348644751282));
#41717=CARTESIAN_POINT('Ctrl Pts',(12.6280122880337,-31.4224641646555,1.27502816094633));
#41718=CARTESIAN_POINT('Ctrl Pts',(10.47805110708,-31.6607163882406,7.16259981817759));
#41719=CARTESIAN_POINT('Ctrl Pts',(5.77279253415804,-31.8989686118257,11.3034179572156));
#41720=CARTESIAN_POINT('Ctrl Pts',(-0.340285255921168,-32.1372208354108,
12.687655303583));
#41721=CARTESIAN_POINT('Ctrl Pts',(-6.37037719127529,-32.3754730589959,
10.9777359049497));
#41722=CARTESIAN_POINT('Ctrl Pts',(-10.846916079753,-32.613725282581,6.59066026409488));
#41723=CARTESIAN_POINT('Ctrl Pts',(-12.6782019449145,-32.8519775061661,
0.596310826607594));
#41724=CARTESIAN_POINT('Ctrl Pts',(-11.4176364692439,-33.0902297297512,
-5.54346178971962));
#41725=CARTESIAN_POINT('Ctrl Pts',(-7.3726355681259,-33.3284819533363,-10.3313424073348));
#41726=CARTESIAN_POINT('Ctrl Pts',(-1.52965942840387,-33.5667341769214,
-12.5997036945728));
#41727=CARTESIAN_POINT('Ctrl Pts',(4.68635695588895,-33.8049864005065,-11.7953571221779));
#41728=CARTESIAN_POINT('Ctrl Pts',(9.75950472997413,-34.0432386240916,-8.11445984550458));
#41729=CARTESIAN_POINT('Ctrl Pts',(12.4525880502679,-34.2814908476767,-2.45467757688521));
#41730=CARTESIAN_POINT('Ctrl Pts',(12.1088408149773,-34.5197430712618,3.80373044244303));
#41731=CARTESIAN_POINT('Ctrl Pts',(8.81209315581226,-34.7579952948469,9.13451724870398));
#41732=CARTESIAN_POINT('Ctrl Pts',(3.3663276672789,-34.996247518432,12.237656197023));
#41733=CARTESIAN_POINT('Ctrl Pts',(-2.90038899301814,-35.2344997420171,
12.3563803299066));
#41734=CARTESIAN_POINT('Ctrl Pts',(-8.45978361366358,-35.4727519656022,
9.46173622141395));
#41735=CARTESIAN_POINT('Ctrl Pts',(-11.9560786482159,-35.7110041891873,
4.25964489491223));
#41736=CARTESIAN_POINT('Ctrl Pts',(-12.5366275691515,-35.9492564127724,
-1.98125216037409));
#41737=CARTESIAN_POINT('Ctrl Pts',(-10.0598511352971,-36.1875086363575,
-7.7389783971189));
#41738=CARTESIAN_POINT('Ctrl Pts',(-5.12976425887965,-36.4257608599426,
-11.6093888526747));
#41739=CARTESIAN_POINT('Ctrl Pts',(1.05132544564253,-36.6640130835277,-12.648600933315));
#41740=CARTESIAN_POINT('Ctrl Pts',(6.97602722060827,-36.9022653071128,-10.6031805544441));
#41741=CARTESIAN_POINT('Ctrl Pts',(11.1994745652053,-37.1405175306979,-5.97194720494374));
#41742=CARTESIAN_POINT('Ctrl Pts',(12.6916912259241,-37.378769754283,0.115673336338168));
#41743=CARTESIAN_POINT('Ctrl Pts',(11.0887643176353,-37.6170219778681,6.17508477858514));
#41744=CARTESIAN_POINT('Ctrl Pts',(6.78160968259757,-37.8552742014532,10.7285687654699));
#41745=CARTESIAN_POINT('Ctrl Pts',(0.820603756208997,-38.0935264250383,
12.6656625634705));
#41746=CARTESIAN_POINT('Ctrl Pts',(-5.34050314292663,-38.3317786486234,
11.5139603988529));
#41747=CARTESIAN_POINT('Ctrl Pts',(-10.1992557008902,-38.5700308722085,
7.55433740992863));
#41748=CARTESIAN_POINT('Ctrl Pts',(-12.5706171211714,-38.8082830957936,
1.75241674191245));
#41749=CARTESIAN_POINT('Ctrl Pts',(-11.8765326492695,-39.0465353193787,
-4.47684713181242));
#41750=CARTESIAN_POINT('Ctrl Pts',(-8.28576249547599,-39.2847875429638,
-9.6143784797947));
#41751=CARTESIAN_POINT('Ctrl Pts',(-2.67501413356175,-39.5230397665489,
-12.4071504841623));
#41752=CARTESIAN_POINT('Ctrl Pts',(3.58949941361916,-39.761291990134,-12.1743630678598));
#41753=CARTESIAN_POINT('Ctrl Pts',(7.17989388445823,-39.9201268058574,-10.0393207828014));
#41754=CARTESIAN_POINT('Ctrl Pts',(8.61150142334309,-39.9995442137191,-8.60695743600425));
#41755=CARTESIAN_POINT('',(-9.92494571122256,-40.0002656632106,-3.43140318666995));
#41756=CARTESIAN_POINT('Ctrl Pts',(8.61094305413662,-40.,-8.60639936142963));
#41757=CARTESIAN_POINT('Ctrl Pts',(8.39826176691623,-40.,-8.79212327549395));
#41758=CARTESIAN_POINT('Ctrl Pts',(8.1793730811141,-40.,-8.96994937667235));
#41759=CARTESIAN_POINT('Ctrl Pts',(7.954781095098,-40.,-9.13970638711416));
#41760=CARTESIAN_POINT('Ctrl Pts',(7.72804274039455,-40.,-9.31108572227973));
#41761=CARTESIAN_POINT('Ctrl Pts',(7.495491008298,-40.,-9.47424130261635));
#41762=CARTESIAN_POINT('Ctrl Pts',(7.25761308334299,-40.,-9.62895430403488));
#41763=CARTESIAN_POINT('Ctrl Pts',(7.01927567527136,-40.,-9.78396614786213));
#41764=CARTESIAN_POINT('Ctrl Pts',(6.77559089325141,-40.,-9.93050302215559));
#41765=CARTESIAN_POINT('Ctrl Pts',(6.52702586402077,-40.,-10.0682981589458));
#41766=CARTESIAN_POINT('Ctrl Pts',(6.27982630171823,-40.,-10.2053363320443));
#41767=CARTESIAN_POINT('Ctrl Pts',(6.02779937839588,-40.,-10.333728742847));
#41768=CARTESIAN_POINT('Ctrl Pts',(5.77139073178792,-40.,-10.4531635937111));
#41769=CARTESIAN_POINT('Ctrl Pts',(5.51880872660686,-40.,-10.5708159994268));
#41770=CARTESIAN_POINT('Ctrl Pts',(5.26197426229078,-40.,-10.6797763198721));
#41771=CARTESIAN_POINT('Ctrl Pts',(5.00130823865076,-40.,-10.7796963458467));
#41772=CARTESIAN_POINT('Ctrl Pts',(4.90713970194856,-40.,-10.8157935805452));
#41773=CARTESIAN_POINT('Ctrl Pts',(4.81247110047981,-40.,-10.8507104815111));
#41774=CARTESIAN_POINT('Ctrl Pts',(4.71732232047202,-40.,-10.8844289444319));
#41775=CARTESIAN_POINT('Ctrl Pts',(4.68473084450778,-40.,-10.8959785877772));
#41776=CARTESIAN_POINT('Ctrl Pts',(4.65208303079231,-40.,-10.9073876128803));
#41777=CARTESIAN_POINT('Ctrl Pts',(4.61937968084376,-40.,-10.9186552672315));
#41778=CARTESIAN_POINT('Ctrl Pts',(4.59185356383537,-40.,-10.9281391510713));
#41779=CARTESIAN_POINT('Ctrl Pts',(4.56428866349076,-40.,-10.9375226531726));
#41780=CARTESIAN_POINT('Ctrl Pts',(4.53669821841154,-40.,-10.9468011456384));
#41781=CARTESIAN_POINT('Ctrl Pts',(4.27228656872564,-40.,-11.0357211138538));
#41782=CARTESIAN_POINT('Ctrl Pts',(4.00522676966733,-40.,-11.1151060432448));
#41783=CARTESIAN_POINT('Ctrl Pts',(3.73596790268631,-40.,-11.1847326159485));
#41784=CARTESIAN_POINT('Ctrl Pts',(3.59988597511649,-40.,-11.2199214969307));
#41785=CARTESIAN_POINT('Ctrl Pts',(3.46324208616997,-40.,-11.2526170856896));
#41786=CARTESIAN_POINT('Ctrl Pts',(3.3260929489447,-40.,-11.2827856394737));
#41787=CARTESIAN_POINT('Ctrl Pts',(3.05396201990356,-40.,-11.3426459983151));
#41788=CARTESIAN_POINT('Ctrl Pts',(2.77984200145971,-40.,-11.3925606000749));
#41789=CARTESIAN_POINT('Ctrl Pts',(2.50427786210809,-40.,-11.4325612835728));
#41790=CARTESIAN_POINT('Ctrl Pts',(2.22869992361977,-40.,-11.472563970143));
#41791=CARTESIAN_POINT('Ctrl Pts',(1.95167706452487,-40.,-11.5026516741963));
#41792=CARTESIAN_POINT('Ctrl Pts',(1.67375680517849,-40.,-11.5228042110682));
#41793=CARTESIAN_POINT('Ctrl Pts',(1.39864205208426,-40.,-11.5427533152421));
#41794=CARTESIAN_POINT('Ctrl Pts',(1.12264731884322,-40.,-11.5529666784976));
#41795=CARTESIAN_POINT('Ctrl Pts',(0.846315501342459,-40.,-11.5533754838016));
#41796=CARTESIAN_POINT('Ctrl Pts',(0.643529262156045,-40.,-11.5536754857736));
#41797=CARTESIAN_POINT('Ctrl Pts',(0.440561694344327,-40.,-11.5486943578675));
#41798=CARTESIAN_POINT('Ctrl Pts',(0.237634295057578,-40.,-11.5383883933861));
#41799=CARTESIAN_POINT('Ctrl Pts',(0.200021572236072,-40.,-11.5364781762995));
#41800=CARTESIAN_POINT('Ctrl Pts',(0.162410249405166,-40.,-11.5343849868962));
#41801=CARTESIAN_POINT('Ctrl Pts',(0.124801765584846,-40.,-11.5321084946763));
#41802=CARTESIAN_POINT('Ctrl Pts',(0.0953789719671696,-40.,-11.5303274933182));
#41803=CARTESIAN_POINT('Ctrl Pts',(0.0659671184443719,-40.,-11.5284348486951));
#41804=CARTESIAN_POINT('Ctrl Pts',(0.0365696537066474,-40.,-11.5264308156415));
#41805=CARTESIAN_POINT('Ctrl Pts',(-0.236604483961962,-40.,-11.5078084614291));
#41806=CARTESIAN_POINT('Ctrl Pts',(-0.508615486317793,-40.,-11.4795673079924));
#41807=CARTESIAN_POINT('Ctrl Pts',(-0.778950107545266,-40.,-11.4417467199426));
#41808=CARTESIAN_POINT('Ctrl Pts',(-1.05191932377333,-40.,-11.4035575445037));
#41809=CARTESIAN_POINT('Ctrl Pts',(-1.32317999343783,-40.,-11.355601299064));
#41810=CARTESIAN_POINT('Ctrl Pts',(-1.59219408909529,-40.,-11.2978654190554));
#41811=CARTESIAN_POINT('Ctrl Pts',(-1.86120818475246,-40.,-11.2401295390468));
#41812=CARTESIAN_POINT('Ctrl Pts',(-2.12797635797297,-40.,-11.1726139378876));
#41813=CARTESIAN_POINT('Ctrl Pts',(-2.39194108188819,-40.,-11.0952540671311));
#41814=CARTESIAN_POINT('Ctrl Pts',(-2.65358663251976,-40.,-11.0185738741089));
#41815=CARTESIAN_POINT('Ctrl Pts',(-2.91247824429427,-40.,-10.9322209570422));
#41816=CARTESIAN_POINT('Ctrl Pts',(-3.16812267150543,-40.,-10.8364284814823));
#41817=CARTESIAN_POINT('Ctrl Pts',(-3.42177931996214,-40.,-10.741380846128));
#41818=CARTESIAN_POINT('Ctrl Pts',(-3.6722395742201,-40.,-10.6370394679647));
#41819=CARTESIAN_POINT('Ctrl Pts',(-3.9189871528201,-40.,-10.5235942855308));
#41820=CARTESIAN_POINT('Ctrl Pts',(-3.96835687549402,-40.,-10.5008959586527));
#41821=CARTESIAN_POINT('Ctrl Pts',(-4.01757784481209,-40.,-10.4778330705644));
#41822=CARTESIAN_POINT('Ctrl Pts',(-4.06664573143816,-40.,-10.4544069809796));
#41823=CARTESIAN_POINT('Ctrl Pts',(-4.10490890648528,-40.,-10.43613929863));
#41824=CARTESIAN_POINT('Ctrl Pts',(-4.14308479220665,-40.,-10.4176478398036));
#41825=CARTESIAN_POINT('Ctrl Pts',(-4.18113965154256,-40.,-10.3989489818942));
#41826=CARTESIAN_POINT('Ctrl Pts',(-4.42108222934686,-40.,-10.28104939569));
#41827=CARTESIAN_POINT('Ctrl Pts',(-4.65640472965588,-40.,-10.154821243158));
#41828=CARTESIAN_POINT('Ctrl Pts',(-4.88668744403159,-40.,-10.0205608401689));
#41829=CARTESIAN_POINT('Ctrl Pts',(-5.1173904554137,-40.,-9.88605539383993));
#41830=CARTESIAN_POINT('Ctrl Pts',(-5.34303579577258,-40.,-9.74348797326746));
#41831=CARTESIAN_POINT('Ctrl Pts',(-5.56317346343205,-40.,-9.59311272976814));
#41832=CARTESIAN_POINT('Ctrl Pts',(-5.78203974319709,-40.,-9.44360596673486));
#41833=CARTESIAN_POINT('Ctrl Pts',(-5.99546225547574,-40.,-9.28638090105349));
#41834=CARTESIAN_POINT('Ctrl Pts',(-6.20296370257059,-40.,-9.12164999225825));
#41835=CARTESIAN_POINT('Ctrl Pts',(-6.40709362328022,-40.,-8.95959566530491));
#41836=CARTESIAN_POINT('Ctrl Pts',(-6.6054936891356,-40.,-8.79027700677452));
#41837=CARTESIAN_POINT('Ctrl Pts',(-6.79766944718012,-40.,-8.61386626213952));
#41838=CARTESIAN_POINT('Ctrl Pts',(-6.91421310879249,-40.,-8.50688318406177));
#41839=CARTESIAN_POINT('Ctrl Pts',(-7.02846683632195,-40.,-8.39729127199965));
#41840=CARTESIAN_POINT('Ctrl Pts',(-7.14031214075949,-40.,-8.28512438529733));
#41841=CARTESIAN_POINT('Ctrl Pts',(-7.2322458360855,-40.,-8.19292635839208));
#41842=CARTESIAN_POINT('Ctrl Pts',(-7.32255217347812,-40.,-8.09898847748873));
#41843=CARTESIAN_POINT('Ctrl Pts',(-7.41118873118237,-40.,-8.00335941612173));
#41844=CARTESIAN_POINT('Ctrl Pts',(-7.44595173807725,-40.,-7.9658539690945));
#41845=CARTESIAN_POINT('Ctrl Pts',(-7.4804578335956,-40.,-7.9280884190582));
#41846=CARTESIAN_POINT('Ctrl Pts',(-7.5147044485466,-40.,-7.89006554572198));
#41847=CARTESIAN_POINT('Ctrl Pts',(-7.54132180807535,-40.,-7.86051317999608));
#41848=CARTESIAN_POINT('Ctrl Pts',(-7.56778133285553,-40.,-7.83080646097683));
#41849=CARTESIAN_POINT('Ctrl Pts',(-7.59406823886229,-40.,-7.8009624892378));
#41850=CARTESIAN_POINT('Ctrl Pts',(-7.76810920704413,-40.,-7.60337081623842));
#41851=CARTESIAN_POINT('Ctrl Pts',(-7.93474820210051,-40.,-7.39958701787578));
#41852=CARTESIAN_POINT('Ctrl Pts',(-8.09372374882493,-40.,-7.1900765576583));
#41853=CARTESIAN_POINT('Ctrl Pts',(-8.25269854013783,-40.,-6.98056709298144));
#41854=CARTESIAN_POINT('Ctrl Pts',(-8.40401024363677,-40.,-6.76533041686787));
#41855=CARTESIAN_POINT('Ctrl Pts',(-8.54735114599831,-40.,-6.54480817806209));
#41856=CARTESIAN_POINT('Ctrl Pts',(-8.68948030195279,-40.,-6.32615014567713));
#41857=CARTESIAN_POINT('Ctrl Pts',(-8.82377306273544,-40.,-6.10229494090462));
#41858=CARTESIAN_POINT('Ctrl Pts',(-8.94988037165709,-40.,-5.87365868174475));
#41859=CARTESIAN_POINT('Ctrl Pts',(-8.96660934330763,-40.,-5.84332856424022));
#41860=CARTESIAN_POINT('Ctrl Pts',(-8.98319419515905,-40.,-5.81291429736071));
#41861=CARTESIAN_POINT('Ctrl Pts',(-8.9996340436321,-40.,-5.78241684186142));
#41862=CARTESIAN_POINT('Ctrl Pts',(-9.02204331979085,-40.,-5.74084554006121));
#41863=CARTESIAN_POINT('Ctrl Pts',(-9.04417775624957,-40.,-5.69912961896715));
#41864=CARTESIAN_POINT('Ctrl Pts',(-9.06603067192976,-40.,-5.65728119034538));
#41865=CARTESIAN_POINT('Ctrl Pts',(-9.18590518599412,-40.,-5.42772097427143));
#41866=CARTESIAN_POINT('Ctrl Pts',(-9.29736055437846,-40.,-5.19408576675231));
#41867=CARTESIAN_POINT('Ctrl Pts',(-9.40010767564824,-40.,-4.95680440176927));
#41868=CARTESIAN_POINT('Ctrl Pts',(-9.50150771608712,-40.,-4.72263394806383));
#41869=CARTESIAN_POINT('Ctrl Pts',(-9.59442649981932,-40.,-4.4849117408585));
#41870=CARTESIAN_POINT('Ctrl Pts',(-9.67853712371623,-40.,-4.2440387488937));
#41871=CARTESIAN_POINT('Ctrl Pts',(-9.73985884412757,-40.,-4.0684278024571));
#41872=CARTESIAN_POINT('Ctrl Pts',(-9.79649777621682,-40.,-3.89114186247201));
#41873=CARTESIAN_POINT('Ctrl Pts',(-9.84830976294177,-40.,-3.71233506504282));
#41874=CARTESIAN_POINT('Ctrl Pts',(-9.87531187063298,-40.,-3.6191488989586));
#41875=CARTESIAN_POINT('Ctrl Pts',(-9.90100270302723,-40.,-3.52554965431835));
#41876=CARTESIAN_POINT('Ctrl Pts',(-9.92537747903998,-40.,-3.43156570488038));
#41877=CARTESIAN_POINT('Ctrl Pts',(7.93381306740072,-20.,-6.87936125025729));
#41878=CARTESIAN_POINT('Ctrl Pts',(8.1133453307756,-20.,-6.70251189458692));
#41879=CARTESIAN_POINT('Ctrl Pts',(8.28605380477966,-20.,-6.51937440106505));
#41880=CARTESIAN_POINT('Ctrl Pts',(8.45179833248014,-20.,-6.3304725879375));
#41881=CARTESIAN_POINT('Ctrl Pts',(8.62014953535816,-20.,-6.13859990346896));
#41882=CARTESIAN_POINT('Ctrl Pts',(8.78131641900121,-20.,-5.94077982286031));
#41883=CARTESIAN_POINT('Ctrl Pts',(8.93512781381366,-20.,-5.73751337586325));
#41884=CARTESIAN_POINT('Ctrl Pts',(9.09135990232769,-20.,-5.53104790834766));
#41885=CARTESIAN_POINT('Ctrl Pts',(9.24000360283395,-20.,-5.3189629086236));
#41886=CARTESIAN_POINT('Ctrl Pts',(9.38084825643788,-20.,-5.10173994480306));
#41887=CARTESIAN_POINT('Ctrl Pts',(9.52214874442358,-20.,-4.88381395326448));
#41888=CARTESIAN_POINT('Ctrl Pts',(9.65560002828852,-20.,-4.66071618819661));
#41889=CARTESIAN_POINT('Ctrl Pts',(9.78095181260842,-20.,-4.43289630258322));
#41890=CARTESIAN_POINT('Ctrl Pts',(9.90574238975571,-20.,-4.20609637974551));
#41891=CARTESIAN_POINT('Ctrl Pts',(10.0225061921301,-20.,-3.97461598479587));
#41892=CARTESIAN_POINT('Ctrl Pts',(10.1309533968524,-20.,-3.73887037049945));
#41893=CARTESIAN_POINT('Ctrl Pts',(10.1620449654918,-20.,-3.67128263536989));
#41894=CARTESIAN_POINT('Ctrl Pts',(10.1924526568096,-20.,-3.6033441669511));
#41895=CARTESIAN_POINT('Ctrl Pts',(10.22216892119,-20.,-3.53506441406799));
#41896=CARTESIAN_POINT('Ctrl Pts',(10.2396840907369,-20.,-3.49481940099851));
#41897=CARTESIAN_POINT('Ctrl Pts',(10.2569611674535,-20.,-3.45445054560652));
#41898=CARTESIAN_POINT('Ctrl Pts',(10.2739835311438,-20.,-3.41399615802376));
#41899=CARTESIAN_POINT('Ctrl Pts',(10.376972988476,-20.,-3.16923723384292));
#41900=CARTESIAN_POINT('Ctrl Pts',(10.4707505425312,-20.,-2.92110624349569));
#41901=CARTESIAN_POINT('Ctrl Pts',(10.5551246852504,-20.,-2.67011766566478));
#41902=CARTESIAN_POINT('Ctrl Pts',(10.5927935636518,-20.,-2.55806368901074));
#41903=CARTESIAN_POINT('Ctrl Pts',(10.6285877022248,-20.,-2.44543962431441));
#41904=CARTESIAN_POINT('Ctrl Pts',(10.6624876486376,-20.,-2.33228893760792));
#41905=CARTESIAN_POINT('Ctrl Pts',(10.7376977925035,-20.,-2.0812537494667));
#41906=CARTESIAN_POINT('Ctrl Pts',(10.8035876329606,-20.,-1.82762824132255));
#41907=CARTESIAN_POINT('Ctrl Pts',(10.8602429504416,-20.,-1.57194508022938));
#41908=CARTESIAN_POINT('Ctrl Pts',(10.9173812906925,-20.,-1.31408205687149));
#41909=CARTESIAN_POINT('Ctrl Pts',(10.9651271234088,-20.,-1.05412557296116));
#41910=CARTESIAN_POINT('Ctrl Pts',(11.0035202229091,-20.,-0.792598803100003));
#41911=CARTESIAN_POINT('Ctrl Pts',(11.0420807378013,-20.,-0.529931630217876));
#41912=CARTESIAN_POINT('Ctrl Pts',(11.0712069012446,-20.,-0.265679827372533));
#41913=CARTESIAN_POINT('Ctrl Pts',(11.0908885652656,-20.,-0.000359128301619826));
#41914=CARTESIAN_POINT('Ctrl Pts',(11.1054206053359,-20.,0.195541534685157));
#41915=CARTESIAN_POINT('Ctrl Pts',(11.1148027799583,-19.9999999999999,0.392025269798154));
#41916=CARTESIAN_POINT('Ctrl Pts',(11.1190128627105,-20.,0.588886412300435));
#41917=CARTESIAN_POINT('Ctrl Pts',(11.1196345841872,-20.,0.617957764914658));
#41918=CARTESIAN_POINT('Ctrl Pts',(11.1201435132142,-20.,0.647039404376552));
#41919=CARTESIAN_POINT('Ctrl Pts',(11.1205394628636,-20.,0.676124093961359));
#41920=CARTESIAN_POINT('Ctrl Pts',(11.1242136969702,-20.,0.946016891253661));
#41921=CARTESIAN_POINT('Ctrl Pts',(11.1181568313559,-20.,1.21559421576539));
#41922=CARTESIAN_POINT('Ctrl Pts',(11.1024699155507,-20.,1.48430357102738));
#41923=CARTESIAN_POINT('Ctrl Pts',(11.0859047811347,-20.,1.76805639051336));
#41924=CARTESIAN_POINT('Ctrl Pts',(11.0586017438615,-20.,2.05084190407209));
#41925=CARTESIAN_POINT('Ctrl Pts',(11.0206211947832,-20.,2.33203086493937));
#41926=CARTESIAN_POINT('Ctrl Pts',(10.9826406457049,-20.,2.61321982580659));
#41927=CARTESIAN_POINT('Ctrl Pts',(10.9339826723985,-20.,2.89281305830032));
#41928=CARTESIAN_POINT('Ctrl Pts',(10.87464624646,-20.,3.17019109503699));
#41929=CARTESIAN_POINT('Ctrl Pts',(10.8153870220998,-20.,3.4472082400973));
#41930=CARTESIAN_POINT('Ctrl Pts',(10.7454772306754,-20.,3.72201679033749));
#41931=CARTESIAN_POINT('Ctrl Pts',(10.6652311260161,-20.,3.99411127683229));
#41932=CARTESIAN_POINT('Ctrl Pts',(10.5849850213568,-20.,4.26620576332708));
#41933=CARTESIAN_POINT('Ctrl Pts',(10.4944023351477,-20.,4.53558691968041));
#41934=CARTESIAN_POINT('Ctrl Pts',(10.3937362784269,-20.,4.80173496530221));
#41935=CARTESIAN_POINT('Ctrl Pts',(10.3777423329852,-20.,4.84402089026791));
#41936=CARTESIAN_POINT('Ctrl Pts',(10.3614937302683,-20.,4.88622515835007));
#41937=CARTESIAN_POINT('Ctrl Pts',(10.3449913509334,-20.,4.92834563232135));
#41938=CARTESIAN_POINT('Ctrl Pts',(10.3343844651706,-20.,4.95541851960774));
#41939=CARTESIAN_POINT('Ctrl Pts',(10.3236726703155,-20.,4.98245685781199));
#41940=CARTESIAN_POINT('Ctrl Pts',(10.3128617315938,-20.,5.00944653944195));
#41941=CARTESIAN_POINT('Ctrl Pts',(10.2113685957593,-20.,5.2628257782202));
#41942=CARTESIAN_POINT('Ctrl Pts',(10.101026009192,-20.,5.51221436662211));
#41943=CARTESIAN_POINT('Ctrl Pts',(9.98219337299323,-20.,5.75718786449156));
#41944=CARTESIAN_POINT('Ctrl Pts',(9.86134406372978,-20.,6.00631873419524));
#41945=CARTESIAN_POINT('Ctrl Pts',(9.73171400203854,-20.,6.25088396547886));
#41946=CARTESIAN_POINT('Ctrl Pts',(9.59362742899954,-20.,6.4904337301993));
#41947=CARTESIAN_POINT('Ctrl Pts',(9.45505341277439,-20.,6.73082910139681));
#41948=CARTESIAN_POINT('Ctrl Pts',(9.30796286010393,-20.,6.96617413669482));
#41949=CARTESIAN_POINT('Ctrl Pts',(9.15263229119251,-20.,7.19600189657105));
#41950=CARTESIAN_POINT('Ctrl Pts',(8.99804398991272,-20.,7.42473139415287));
#41951=CARTESIAN_POINT('Ctrl Pts',(8.83529395844639,-20.,7.64799680129097));
#41952=CARTESIAN_POINT('Ctrl Pts',(8.66460799084262,-20.,7.86531682618203));
#41953=CARTESIAN_POINT('Ctrl Pts',(8.55444285880692,-20.,8.00558078327371));
#41954=CARTESIAN_POINT('Ctrl Pts',(8.44097088267069,-20.,8.14336759878132));
#41955=CARTESIAN_POINT('Ctrl Pts',(8.32424315342715,-20.,8.27854145188553));
#41956=CARTESIAN_POINT('Ctrl Pts',(8.23663382474174,-20.,8.37999541319385));
#41957=CARTESIAN_POINT('Ctrl Pts',(8.14719031008403,-20.,8.47997733921384));
#41958=CARTESIAN_POINT('Ctrl Pts',(8.05595931410645,-20.,8.57845490970599));
#41959=CARTESIAN_POINT('Ctrl Pts',(8.01761638599056,-20.,8.61984345716124));
#41960=CARTESIAN_POINT('Ctrl Pts',(7.97895769445338,-20.,8.66096625341727));
#41961=CARTESIAN_POINT('Ctrl Pts',(7.93998660073734,-20.,8.70182079217647));
#41962=CARTESIAN_POINT('Ctrl Pts',(7.91066081922242,-20.,8.7325638677051));
#41963=CARTESIAN_POINT('Ctrl Pts',(7.88115851940967,-20.,8.76315450959376));
#41964=CARTESIAN_POINT('Ctrl Pts',(7.85149823338772,-20.,8.79357447449731));
#41965=CARTESIAN_POINT('Ctrl Pts',(7.65681753599435,-20.,8.9932414627969));
#41966=CARTESIAN_POINT('Ctrl Pts',(7.45515096990198,-20.,9.18575086334707));
#41967=CARTESIAN_POINT('Ctrl Pts',(7.2470114550717,-20.,9.37088205609219));
#41968=CARTESIAN_POINT('Ctrl Pts',(7.03612872385928,-20.,9.55845322243481));
#41969=CARTESIAN_POINT('Ctrl Pts',(6.81860091988332,-20.,9.73845086287543));
#41970=CARTESIAN_POINT('Ctrl Pts',(6.59491638211396,-20.,9.91061618523869));
#41971=CARTESIAN_POINT('Ctrl Pts',(6.37323524853758,-20.,10.0812395291883));
#41972=CARTESIAN_POINT('Ctrl Pts',(6.14550664670372,-20.,10.2441705630064));
#41973=CARTESIAN_POINT('Ctrl Pts',(5.91216887742395,-20.,10.399123041683));
#41974=CARTESIAN_POINT('Ctrl Pts',(5.86175766100922,-20.,10.4325995892675));
#41975=CARTESIAN_POINT('Ctrl Pts',(5.81108451494134,-20.,10.4657035986193));
#41976=CARTESIAN_POINT('Ctrl Pts',(5.76015366565449,-20.,10.4984319462714));
#41977=CARTESIAN_POINT('Ctrl Pts',(5.72101534189377,-20.,10.5235823744401));
#41978=CARTESIAN_POINT('Ctrl Pts',(5.68172721143778,-20.,10.5485093492459));
#41979=CARTESIAN_POINT('Ctrl Pts',(5.64230701875108,-20.,10.5732018578478));
#41980=CARTESIAN_POINT('Ctrl Pts',(5.39975652925315,-20.,10.7251336379868));
#41981=CARTESIAN_POINT('Ctrl Pts',(5.1520474980573,-20.,10.8682962687084));
#41982=CARTESIAN_POINT('Ctrl Pts',(4.8996827113077,-20.,11.0024328307128));
#41983=CARTESIAN_POINT('Ctrl Pts',(4.64696653000309,-20.,11.1367561654366));
#41984=CARTESIAN_POINT('Ctrl Pts',(4.38958112280953,-20.,11.2620286879808));
#41985=CARTESIAN_POINT('Ctrl Pts',(4.12799552796009,-20.,11.3779546570887));
#41986=CARTESIAN_POINT('Ctrl Pts',(3.90990991961388,-20.,11.4746028899953));
#41987=CARTESIAN_POINT('Ctrl Pts',(3.68890412368266,-20.,11.564754097854));
#41988=CARTESIAN_POINT('Ctrl Pts',(3.46523470555786,-20.,11.6482137561969));
#41989=CARTESIAN_POINT('Ctrl Pts',(3.36017632166552,-20.,11.6874150779477));
#41990=CARTESIAN_POINT('Ctrl Pts',(3.25453010754724,-20.,11.7251397777184));
#41991=CARTESIAN_POINT('Ctrl Pts',(3.14832787575818,-20.,11.7613864006883));
#41992=CARTESIAN_POINT('Ctrl Pts',(-9.92458237182475,-40.0002656632106,
-3.43127756744706));
#41993=CARTESIAN_POINT('Ctrl Pts',(-9.92574258937462,-40.0001771088071,
-3.42792176937577));
#41994=CARTESIAN_POINT('Ctrl Pts',(-9.92690110488082,-40.0000885544035,
-3.42456538284806));
#41995=CARTESIAN_POINT('Ctrl Pts',(-9.92805791774733,-40.,-3.42120840959077));
#41996=CARTESIAN_POINT('Ctrl Pts',(-3.14809266229074,-20.0004548598273,
11.7612561652465));
#41997=CARTESIAN_POINT('Ctrl Pts',(-5.10435921967941,-20.079872267689,11.2376294107338));
#41998=CARTESIAN_POINT('Ctrl Pts',(-8.74855648214142,-20.2387070834124,
9.19577637638592));
#41999=CARTESIAN_POINT('Ctrl Pts',(-12.0824131583272,-20.4769593069975,
3.88694525557923));
#42000=CARTESIAN_POINT('Ctrl Pts',(-12.4691756011198,-20.7152115305826,
-2.36849165908917));
#42001=CARTESIAN_POINT('Ctrl Pts',(-9.81532842158459,-20.9534637541677,
-8.04695416362741));
#42002=CARTESIAN_POINT('Ctrl Pts',(-4.76767052948596,-21.1917159777528,
-11.7626807483447));
#42003=CARTESIAN_POINT('Ctrl Pts',(1.44262007163241,-21.4299682013379,-12.6099815538241));
#42004=CARTESIAN_POINT('Ctrl Pts',(7.30112969128478,-21.668220424923,-10.3819902917566));
#42005=CARTESIAN_POINT('Ctrl Pts',(11.3790859526647,-21.9064726485081,-5.62216684002108));
#42006=CARTESIAN_POINT('Ctrl Pts',(12.6820163068472,-22.1447248720932,0.508761805007712));
#42007=CARTESIAN_POINT('Ctrl Pts',(10.8921610480429,-22.3829770956783,6.51560837433268));
#42008=CARTESIAN_POINT('Ctrl Pts',(6.44602083161166,-22.6212293192634,10.9334889418598));
#42009=CARTESIAN_POINT('Ctrl Pts',(0.427879238319787,-22.8594815428485,
12.6850014557692));
#42010=CARTESIAN_POINT('Ctrl Pts',(-5.69460937880688,-23.0977337664336,
11.343005608659));
#42011=CARTESIAN_POINT('Ctrl Pts',(-10.4283456669994,-23.3359859900187,
7.2347740805613));
#42012=CARTESIAN_POINT('Ctrl Pts',(-12.6189061760199,-23.5742382136038,
1.36218808736743));
#42013=CARTESIAN_POINT('Ctrl Pts',(-11.7320759505821,-23.8124904371889,
-4.8425968202088));
#42014=CARTESIAN_POINT('Ctrl Pts',(-7.9841274603316,-24.050742660774,-9.86641060411259));
#42015=CARTESIAN_POINT('Ctrl Pts',(-2.28907833971999,-24.2889948843591,
-12.4840886814594));
#42016=CARTESIAN_POINT('Ctrl Pts',(3.96421161517395,-24.5272471079442,-12.0572540805866));
#42017=CARTESIAN_POINT('Ctrl Pts',(9.25074357873224,-24.7654993315293,-8.68999959656226));
#42018=CARTESIAN_POINT('Ctrl Pts',(12.2812834041494,-25.0037515551144,-3.20350240934556));
#42019=CARTESIAN_POINT('Ctrl Pts',(12.3167689831387,-25.2420037786995,3.06423751515814));
#42020=CARTESIAN_POINT('Ctrl Pts',(9.34854639793627,-25.4802560022846,8.58469743127443));
#42021=CARTESIAN_POINT('Ctrl Pts',(4.10048035829083,-25.7185082258697,12.0115948386183));
#42022=CARTESIAN_POINT('Ctrl Pts',(-2.14757572311472,-25.9567604494548,
12.5092073390711));
#42023=CARTESIAN_POINT('Ctrl Pts',(-7.87189942455396,-26.1950126730399,
9.95618145611698));
#42024=CARTESIAN_POINT('Ctrl Pts',(-11.6764916927204,-26.433264896625,4.97512728354432));
#42025=CARTESIAN_POINT('Ctrl Pts',(-12.6335211398357,-26.6715171202101,
-1.21921833443057));
#42026=CARTESIAN_POINT('Ctrl Pts',(-10.5095956183063,-26.9097693437952,
-7.11623142381309));
#42027=CARTESIAN_POINT('Ctrl Pts',(-5.82267989949552,-27.1480215673803,
-11.2777989220269));
#42028=CARTESIAN_POINT('Ctrl Pts',(0.284221140002502,-27.3862737909654,
-12.6890333785201));
#42029=CARTESIAN_POINT('Ctrl Pts',(6.32180876134884,-27.6245260145505,-11.0057750168977));
#42030=CARTESIAN_POINT('Ctrl Pts',(10.8176877886728,-27.8627782381356,-6.63852247449934));
#42031=CARTESIAN_POINT('Ctrl Pts',(12.6754417380569,-28.1010304617207,-0.652323909386644));
#42032=CARTESIAN_POINT('Ctrl Pts',(11.4420174822295,-28.3392826853058,5.49295782561537));
#42033=CARTESIAN_POINT('Ctrl Pts',(7.41821196824627,-28.5775349088909,10.2986640362622));
#42034=CARTESIAN_POINT('Ctrl Pts',(1.58531643343681,-28.815787132476,12.592820237878));
#42035=CARTESIAN_POINT('Ctrl Pts',(-4.63419249983834,-29.0540393560611,
11.8159472583486));
#42036=CARTESIAN_POINT('Ctrl Pts',(-9.72355424374604,-29.2922915796462,
8.15750222841293));
#42037=CARTESIAN_POINT('Ctrl Pts',(-12.4416188307888,-29.5305438032313,
2.50967539873089));
#42038=CARTESIAN_POINT('Ctrl Pts',(-12.125527941276,-29.7687960268164,-3.75018957960365));
#42039=CARTESIAN_POINT('Ctrl Pts',(-8.85236711500349,-30.0070482504015,
-9.0954904320129));
#42040=CARTESIAN_POINT('Ctrl Pts',(-3.42036678980662,-30.2453004739866,
-12.2226609525431));
#42041=CARTESIAN_POINT('Ctrl Pts',(2.8457633032496,-30.4835526975717,-12.3690735691688));
#42042=CARTESIAN_POINT('Ctrl Pts',(8.41789300705035,-30.7218049211568,-9.4990224265177));
#42043=CARTESIAN_POINT('Ctrl Pts',(11.9371390374505,-30.9600571447419,-4.3124310241683));
#42044=CARTESIAN_POINT('Ctrl Pts',(12.5452578039889,-31.198309368327,1.92583913375176));
#42045=CARTESIAN_POINT('Ctrl Pts',(10.0939465085343,-31.4365615919121,7.69445213257468));
#42046=CARTESIAN_POINT('Ctrl Pts',(5.18100996193967,-31.6748138154972,11.5866080244356));
#42047=CARTESIAN_POINT('Ctrl Pts',(-0.995426934883139,-31.9130660390823,
12.6531211546773));
#42048=CARTESIAN_POINT('Ctrl Pts',(-6.92910763357261,-32.1513182626674,
10.6338994324754));
#42049=CARTESIAN_POINT('Ctrl Pts',(-11.1729768889136,-32.3895704862526,
6.02137336306566));
#42050=CARTESIAN_POINT('Ctrl Pts',(-12.692076202498,-32.6278227098376,-0.0595936877313756));
#42051=CARTESIAN_POINT('Ctrl Pts',(-11.1159406401054,-32.8660749334227,
-6.12602754019978));
#42052=CARTESIAN_POINT('Ctrl Pts',(-6.82894464797713,-33.1043271570078,
-10.6984982465997));
#42053=CARTESIAN_POINT('Ctrl Pts',(-0.876564103841478,-33.3425793805929,
-12.6619108000923));
#42054=CARTESIAN_POINT('Ctrl Pts',(5.28958538888388,-33.580831604178,-11.5374449576727));
#42055=CARTESIAN_POINT('Ctrl Pts',(10.1657560858716,-33.8190838277631,-7.59932582142831));
#42056=CARTESIAN_POINT('Ctrl Pts',(12.5627892268212,-34.0573360513483,-1.80794816851931));
#42057=CARTESIAN_POINT('Ctrl Pts',(11.8961168924868,-34.2955882749333,4.42433640425057));
#42058=CARTESIAN_POINT('Ctrl Pts',(8.32832142376291,-34.5338404985185,9.5776516954902));
#42059=CARTESIAN_POINT('Ctrl Pts',(2.72948623249549,-34.7720927221035,12.395251294106));
#42060=CARTESIAN_POINT('Ctrl Pts',(-3.53499269162053,-35.0103449456886,
12.1900031340674));
#42061=CARTESIAN_POINT('Ctrl Pts',(-8.93738786424591,-35.2485971692737,
9.01196137918275));
#42062=CARTESIAN_POINT('Ctrl Pts',(-12.1602094057867,-35.4868493928589,
3.63615964285339));
#42063=CARTESIAN_POINT('Ctrl Pts',(-12.4175031914886,-35.7251016164439,
-2.62639757513609));
#42064=CARTESIAN_POINT('Ctrl Pts',(-9.6465226171822,-35.9633538400291,-8.24845143865875));
#42065=CARTESIAN_POINT('Ctrl Pts',(-4.52303069773246,-36.2016060636141,
-11.858943589337));
#42066=CARTESIAN_POINT('Ctrl Pts',(1.70349921887366,-36.4398582871992,-12.5773781093279));
#42067=CARTESIAN_POINT('Ctrl Pts',(7.51459433853917,-36.6781105107843,-10.2285493487157));
#42068=CARTESIAN_POINT('Ctrl Pts',(11.4930945153334,-36.9163627343694,-5.38526953581525));
#42069=CARTESIAN_POINT('Ctrl Pts',(12.6687572341596,-37.1546149579545,0.771323677356681));
#42070=CARTESIAN_POINT('Ctrl Pts',(10.7548718477098,-37.3928671815396,6.7398131282622));
#42071=CARTESIAN_POINT('Ctrl Pts',(6.2181805169326,-37.6311194051247,11.0646545543017));
#42072=CARTESIAN_POINT('Ctrl Pts',(0.165052320677689,-37.8693716287098,
12.6911429724317));
#42073=CARTESIAN_POINT('Ctrl Pts',(-5.92832693959693,-38.107623852295,11.2226236804367));
#42074=CARTESIAN_POINT('Ctrl Pts',(-10.5759575529497,-38.34587607588,7.01722786017004));
#42075=CARTESIAN_POINT('Ctrl Pts',(-12.644412242237,-38.5841282994652,1.10052888764604));
#42076=CARTESIAN_POINT('Ctrl Pts',(-11.6292598420606,-38.8223805230502,
-5.08455422895767));
#42077=CARTESIAN_POINT('Ctrl Pts',(-7.77805527350331,-39.0606327466353,
-10.0296666573467));
#42078=CARTESIAN_POINT('Ctrl Pts',(-2.03002093474416,-39.2988849702204,
-12.528816073021));
#42079=CARTESIAN_POINT('Ctrl Pts',(4.21310916249937,-39.5371371938055,-11.972572766274));
#42080=CARTESIAN_POINT('Ctrl Pts',(9.42871875276412,-39.7753894173906,-8.49650536082229));
#42081=CARTESIAN_POINT('Ctrl Pts',(12.3450606821512,-40.0136416409757,-2.94849454622041));
#42082=CARTESIAN_POINT('Ctrl Pts',(12.2505387102373,-40.2518938645608,3.31879409118882));
#42083=CARTESIAN_POINT('Ctrl Pts',(9.16897630005181,-40.4901460881459,8.77627054946899));
#42084=CARTESIAN_POINT('Ctrl Pts',(3.84984706557644,-40.7284188590102,12.0946935166284));
#42085=CARTESIAN_POINT('Ctrl Pts',(-0.32088071557368,-40.8872742220127,
12.3384797159896));
#42086=CARTESIAN_POINT('Ctrl Pts',(-2.30975236282056,-40.9667121771536,
11.9541908119849));
#42087=CARTESIAN_POINT('Ctrl Pts',(-3.00369270810988,-19.6780228441179,
11.2217787630359));
#42088=CARTESIAN_POINT('Ctrl Pts',(-4.87022721769824,-19.7574402519795,
10.7221702594042));
#42089=CARTESIAN_POINT('Ctrl Pts',(-8.34726868959891,-19.916275067703,8.77397504146546));
#42090=CARTESIAN_POINT('Ctrl Pts',(-11.5282045966303,-20.154527291288,3.70865485023876));
#42091=CARTESIAN_POINT('Ctrl Pts',(-11.8972266216495,-20.3927795148732,
-2.25985124607116));
#42092=CARTESIAN_POINT('Ctrl Pts',(-9.36510883582578,-20.6310317384582,
-7.67784818830401));
#42093=CARTESIAN_POINT('Ctrl Pts',(-4.54898211085908,-20.8692839620433,
-11.2231380018903));
#42094=CARTESIAN_POINT('Ctrl Pts',(1.3764484894743,-21.1075361856285,-12.031573942001));
#42095=CARTESIAN_POINT('Ctrl Pts',(6.96623396044474,-21.3457884092135,-9.90577847614093));
#42096=CARTESIAN_POINT('Ctrl Pts',(10.8571383270859,-21.5840406327987,-5.364283505194));
#42097=CARTESIAN_POINT('Ctrl Pts',(12.1003045308358,-21.8222928563837,0.485425394929287));
#42098=CARTESIAN_POINT('Ctrl Pts',(10.3925481951215,-22.0605450799689,6.21674374369965));
#42099=CARTESIAN_POINT('Ctrl Pts',(6.15034811400611,-22.2987973035539,10.431980418571));
#42100=CARTESIAN_POINT('Ctrl Pts',(0.408252833052742,-22.5370495271391,
12.1031527538748));
#42101=CARTESIAN_POINT('Ctrl Pts',(-5.43340317505451,-22.7753017507242,
10.8227129534321));
#42102=CARTESIAN_POINT('Ctrl Pts',(-9.95000757532424,-23.0135539743092,
6.90292201716564));
#42103=CARTESIAN_POINT('Ctrl Pts',(-12.0400892004407,-23.2518061978944,
1.2997058422424));
#42104=CARTESIAN_POINT('Ctrl Pts',(-11.1939370164893,-23.4900584214795,
-4.62047160536659));
#42105=CARTESIAN_POINT('Ctrl Pts',(-7.61790328489481,-23.7283106450646,
-9.41384792823294));
#42106=CARTESIAN_POINT('Ctrl Pts',(-2.18408053856523,-23.9665628686497,
-11.911455653472));
#42107=CARTESIAN_POINT('Ctrl Pts',(3.78237707693078,-24.2048150922347,-11.5041995413608));
#42108=CARTESIAN_POINT('Ctrl Pts',(8.82642095160353,-24.4430673158199,-8.29139775151294));
#42109=CARTESIAN_POINT('Ctrl Pts',(11.7179528573444,-24.6813195394049,-3.05656086386032));
#42110=CARTESIAN_POINT('Ctrl Pts',(11.7518107472756,-24.9195717629901,2.92368391516781));
#42111=CARTESIAN_POINT('Ctrl Pts',(8.91973765043983,-25.1578239865751,8.19092569431719));
#42112=CARTESIAN_POINT('Ctrl Pts',(3.9123953050936,-25.3960762101603,11.4606346444945));
#42113=CARTESIAN_POINT('Ctrl Pts',(-2.04906850960975,-25.6343284337454,
11.9354221426448));
#42114=CARTESIAN_POINT('Ctrl Pts',(-7.51082304016482,-25.8725806573305,
9.49950107840742));
#42115=CARTESIAN_POINT('Ctrl Pts',(-11.1409023545732,-26.1108328809156,
4.74692302501242));
#42116=CARTESIAN_POINT('Ctrl Pts',(-12.0540337900549,-26.3490851045007,
-1.16329397307453));
#42117=CARTESIAN_POINT('Ctrl Pts',(-10.0275306702439,-26.5873373280858,
-6.78981679699862));
#42118=CARTESIAN_POINT('Ctrl Pts',(-5.55559922529289,-26.8255895516709,
-10.7604972342117));
#42119=CARTESIAN_POINT('Ctrl Pts',(0.271184192238789,-27.063841775256,-12.1069997362434));
#42120=CARTESIAN_POINT('Ctrl Pts',(6.03183353081841,-27.3020939988411,-10.500950801524));
#42121=CARTESIAN_POINT('Ctrl Pts',(10.3214909518584,-27.5403462224262,-6.3340198934194));
#42122=CARTESIAN_POINT('Ctrl Pts',(12.0940315311332,-27.7785984460113,-0.622402444953652));
#42123=CARTESIAN_POINT('Ctrl Pts',(10.9171832484849,-28.0168506695964,5.24100118284009));
#42124=CARTESIAN_POINT('Ctrl Pts',(7.07794578702809,-28.2551028931814,9.82627431509112));
#42125=CARTESIAN_POINT('Ctrl Pts',(1.51259950769554,-28.4933551167666,12.0151997989567));
#42126=CARTESIAN_POINT('Ctrl Pts',(-4.42162658884796,-28.7316073403516,
11.2739612287927));
#42127=CARTESIAN_POINT('Ctrl Pts',(-9.27754425042827,-28.9698595639368,
7.78332552068034));
#42128=CARTESIAN_POINT('Ctrl Pts',(-11.870933853621,-29.2081117875218,2.39455902463984));
#42129=CARTESIAN_POINT('Ctrl Pts',(-11.5693417463421,-29.446364011107,-3.57817202435472));
#42130=CARTESIAN_POINT('Ctrl Pts',(-8.44631762951329,-29.6846162346921,
-8.678289116001));
#42131=CARTESIAN_POINT('Ctrl Pts',(-3.26347788572639,-29.9228684582772,
-11.6620193606813));
#42132=CARTESIAN_POINT('Ctrl Pts',(2.71523090325989,-30.1611206818622,-11.801716172723));
#42133=CARTESIAN_POINT('Ctrl Pts',(8.03177242709483,-30.3993729054474,-9.06331148967571));
#42134=CARTESIAN_POINT('Ctrl Pts',(11.3895940586429,-30.6376251290325,-4.11462399969371));
#42135=CARTESIAN_POINT('Ctrl Pts',(11.9698190077354,-30.8758773526176,1.83750276233406));
#42136=CARTESIAN_POINT('Ctrl Pts',(9.63094698161567,-31.1141295762027,7.34151508319886));
#42137=CARTESIAN_POINT('Ctrl Pts',(4.94336206482527,-31.3523817997878,11.0551415628917));
#42138=CARTESIAN_POINT('Ctrl Pts',(-0.949767667762671,-31.5906340233729,
12.0727347712439));
#42139=CARTESIAN_POINT('Ctrl Pts',(-6.61127619335253,-31.828886246958,10.1461327891339));
#42140=CARTESIAN_POINT('Ctrl Pts',(-10.6604832859937,-32.0671384705431,
5.7451788125851));
#42141=CARTESIAN_POINT('Ctrl Pts',(-12.1099029888395,-32.3053906941281,
-0.0568601831300151));
#42142=CARTESIAN_POINT('Ctrl Pts',(-10.6060632345463,-32.5436429177133,
-5.84503260421468));
#42143=CARTESIAN_POINT('Ctrl Pts',(-6.51570758666586,-32.7818951412983,
-10.2077685183684));
#42144=CARTESIAN_POINT('Ctrl Pts',(-0.836356959386205,-33.0201473648835,
-12.0811212441569));
#42145=CARTESIAN_POINT('Ctrl Pts',(5.04695724234298,-33.2583995884685,-11.0082335582726));
#42146=CARTESIAN_POINT('Ctrl Pts',(9.69946272335483,-33.4966518120537,-7.25075212359403));
#42147=CARTESIAN_POINT('Ctrl Pts',(11.9865462812223,-33.7349040356388,-1.72501934122564));
#42148=CARTESIAN_POINT('Ctrl Pts',(11.3504535596434,-33.9731562592238,4.22139638863183));
#42149=CARTESIAN_POINT('Ctrl Pts',(7.94630940537469,-34.211408482809,9.13833411041546));
#42150=CARTESIAN_POINT('Ctrl Pts',(2.6042873488569,-34.4496607063941,11.8266931508312));
#42151=CARTESIAN_POINT('Ctrl Pts',(-3.37284600870548,-34.6879129299792,
11.630859524634));
#42152=CARTESIAN_POINT('Ctrl Pts',(-8.52743855952799,-34.9261651535643,
8.5985914597323));
#42153=CARTESIAN_POINT('Ctrl Pts',(-11.6024324057451,-35.1644173771494,
3.46937253010039));
#42154=CARTESIAN_POINT('Ctrl Pts',(-11.8479243752835,-35.4026696007345,
-2.5059272681298));
#42155=CARTESIAN_POINT('Ctrl Pts',(-9.20404598979087,-35.6409218243196,
-7.8701029789477));
#42156=CARTESIAN_POINT('Ctrl Pts',(-4.31556367068634,-35.8791740479047,
-11.3149853598205));
#42157=CARTESIAN_POINT('Ctrl Pts',(1.62536136349889,-36.1174262714898,-12.0004659858516));
#42158=CARTESIAN_POINT('Ctrl Pts',(7.16990719156578,-36.3556784950749,-9.75937572019344));
#42159=CARTESIAN_POINT('Ctrl Pts',(10.965917427667,-36.59393071866,-5.1382524503469));
#42160=CARTESIAN_POINT('Ctrl Pts',(12.0876536389402,-36.8321829422451,0.735943809094519));
#42161=CARTESIAN_POINT('Ctrl Pts',(10.2615563171244,-37.0704351658302,6.43066444322939));
#42162=CARTESIAN_POINT('Ctrl Pts',(5.93295861336892,-37.3086873894153,10.5571295917087));
#42163=CARTESIAN_POINT('Ctrl Pts',(0.157481530964674,-37.5469396130003,
12.1090125651303));
#42164=CARTESIAN_POINT('Ctrl Pts',(-5.65640033822935,-37.7851918365855,
10.7078528273879));
#42165=CARTESIAN_POINT('Ctrl Pts',(-10.0908486473709,-38.0234440601705,
6.69535443070501));
#42166=CARTESIAN_POINT('Ctrl Pts',(-12.0644253281625,-38.2616962837557,
1.05004869598765));
#42167=CARTESIAN_POINT('Ctrl Pts',(-11.0958369830495,-38.4999485073408,
-4.85133066267378));
#42168=CARTESIAN_POINT('Ctrl Pts',(-7.42128342921687,-38.7382007309259,
-9.56961558479783));
#42169=CARTESIAN_POINT('Ctrl Pts',(-1.93690584525694,-38.976452954511,-11.954131443005));
#42170=CARTESIAN_POINT('Ctrl Pts',(4.01985793539565,-39.2147051780961,-11.4234024767251));
#42171=CARTESIAN_POINT('Ctrl Pts',(8.99623257718483,-39.4529574016812,-8.10677890851787));
#42172=CARTESIAN_POINT('Ctrl Pts',(11.7788047335206,-39.6912096252663,-2.8132499638494));
#42173=CARTESIAN_POINT('Ctrl Pts',(11.6886183926944,-39.9294618488514,3.16656422818516));
#42174=CARTESIAN_POINT('Ctrl Pts',(8.74840425861466,-40.1677140724365,8.3737115395636));
#42175=CARTESIAN_POINT('Ctrl Pts',(3.67325831819566,-40.4059868433008,11.5399216668183));
#42176=CARTESIAN_POINT('Ctrl Pts',(-0.306162228668456,-40.5648422063033,
11.7725256298878));
#42177=CARTESIAN_POINT('Ctrl Pts',(-2.20380626429698,-40.6442801614442,
11.4058636848336));
#42178=CARTESIAN_POINT('Ctrl Pts',(-2.85929275392902,-19.3555908284084,
10.6823013608252));
#42179=CARTESIAN_POINT('Ctrl Pts',(-4.63609521571708,-19.4350082362701,
10.2067111080746));
#42180=CARTESIAN_POINT('Ctrl Pts',(-7.94598089705643,-19.5938430519935,
8.35217370654499));
#42181=CARTESIAN_POINT('Ctrl Pts',(-10.9739960349335,-19.8320952755786,
3.53036444489831));
#42182=CARTESIAN_POINT('Ctrl Pts',(-11.3252776421793,-20.0703474991637,
-2.15121083305315));
#42183=CARTESIAN_POINT('Ctrl Pts',(-8.91488925006696,-20.3085997227488,
-7.3087422129806));
#42184=CARTESIAN_POINT('Ctrl Pts',(-4.33029369223223,-20.5468519463339,
-10.683595255436));
#42185=CARTESIAN_POINT('Ctrl Pts',(1.31027690731619,-20.785104169919,-11.4531663301778));
#42186=CARTESIAN_POINT('Ctrl Pts',(6.6313382296047,-21.0233563935041,-9.42956666052528));
#42187=CARTESIAN_POINT('Ctrl Pts',(10.3351907015071,-21.2616086170892,-5.10640017036693));
#42188=CARTESIAN_POINT('Ctrl Pts',(11.5185927548245,-21.4998608406743,0.462088984850871));
#42189=CARTESIAN_POINT('Ctrl Pts',(9.89293534220016,-21.7381130642594,5.91787911306662));
#42190=CARTESIAN_POINT('Ctrl Pts',(5.85467539640056,-21.9763652878445,9.93047189528233));
#42191=CARTESIAN_POINT('Ctrl Pts',(0.388626427785698,-22.2146175114296,
11.5213040519803));
#42192=CARTESIAN_POINT('Ctrl Pts',(-5.17219697130215,-22.4528697350147,
10.3024202982052));
#42193=CARTESIAN_POINT('Ctrl Pts',(-9.47166948364905,-22.6911219585998,
6.57106995376998));
#42194=CARTESIAN_POINT('Ctrl Pts',(-11.4612722248617,-22.9293741821849,
1.23722359711736));
#42195=CARTESIAN_POINT('Ctrl Pts',(-10.6557980823965,-23.16762640577,-4.39834639052438));
#42196=CARTESIAN_POINT('Ctrl Pts',(-7.25167910945802,-23.4058786293551,
-8.96128525235328));
#42197=CARTESIAN_POINT('Ctrl Pts',(-2.07908273741047,-23.6441308529403,
-11.3388226254846));
#42198=CARTESIAN_POINT('Ctrl Pts',(3.6005425386876,-23.8823830765253,-10.9511450021349));
#42199=CARTESIAN_POINT('Ctrl Pts',(8.40209832447484,-24.1206353001105,-7.89279590646365));
#42200=CARTESIAN_POINT('Ctrl Pts',(11.1546223105393,-24.3588875236955,-2.90961931837506));
#42201=CARTESIAN_POINT('Ctrl Pts',(11.1868525114124,-24.5971397472806,2.78313031517747));
#42202=CARTESIAN_POINT('Ctrl Pts',(8.49092890294339,-24.8353919708657,7.79715395735995));
#42203=CARTESIAN_POINT('Ctrl Pts',(3.72431025189639,-25.0736441944508,10.9096744503706));
#42204=CARTESIAN_POINT('Ctrl Pts',(-1.95056129610478,-25.3118964180359,
11.3616369462185));
#42205=CARTESIAN_POINT('Ctrl Pts',(-7.14974665577569,-25.550148641621,9.04282070069786));
#42206=CARTESIAN_POINT('Ctrl Pts',(-10.6053130164261,-25.7884008652061,
4.51871876648054));
#42207=CARTESIAN_POINT('Ctrl Pts',(-11.4745464402741,-26.0266530887912,
-1.1073696117185));
#42208=CARTESIAN_POINT('Ctrl Pts',(-9.54546572218151,-26.2649053123763,
-6.46340217018414));
#42209=CARTESIAN_POINT('Ctrl Pts',(-5.28851855109026,-26.5031575359614,
-10.2431955463965));
#42210=CARTESIAN_POINT('Ctrl Pts',(0.258147244475094,-26.7414097595465,
-11.5249660939666));
#42211=CARTESIAN_POINT('Ctrl Pts',(5.74185830028796,-26.9796619831316,-9.9961265861502));
#42212=CARTESIAN_POINT('Ctrl Pts',(9.82529411504405,-27.2179142067167,-6.02951731233948));
#42213=CARTESIAN_POINT('Ctrl Pts',(11.5126213242094,-27.4561664303018,-0.592480980520653));
#42214=CARTESIAN_POINT('Ctrl Pts',(10.3923490147401,-27.6944186538869,4.98904454006482));
#42215=CARTESIAN_POINT('Ctrl Pts',(6.73767960580988,-27.932670877472,9.35388459392002));
#42216=CARTESIAN_POINT('Ctrl Pts',(1.43988258195426,-28.1709231010571,11.4375793600353));
#42217=CARTESIAN_POINT('Ctrl Pts',(-4.2090606778576,-28.4091753246422,10.7319751992368));
#42218=CARTESIAN_POINT('Ctrl Pts',(-8.83153425711049,-28.6474275482273,
7.40914881294773));
#42219=CARTESIAN_POINT('Ctrl Pts',(-11.3002488764531,-28.8856797718124,
2.27944265054878));
#42220=CARTESIAN_POINT('Ctrl Pts',(-11.0131555514081,-29.1239319953975,
-3.40615446910582));
#42221=CARTESIAN_POINT('Ctrl Pts',(-8.04026814402308,-29.3621842189826,
-8.2610877999891));
#42222=CARTESIAN_POINT('Ctrl Pts',(-3.10658898164615,-29.6004364425677,
-11.1013777688193));
#42223=CARTESIAN_POINT('Ctrl Pts',(2.58469850327018,-29.8386886661528,-11.2343587762771));
#42224=CARTESIAN_POINT('Ctrl Pts',(7.64565184713929,-30.0769408897379,-8.62760055283371));
#42225=CARTESIAN_POINT('Ctrl Pts',(10.8420490798353,-30.315193113323,-3.91681697521912));
#42226=CARTESIAN_POINT('Ctrl Pts',(11.3943802114819,-30.5534453369081,1.74916639091636));
#42227=CARTESIAN_POINT('Ctrl Pts',(9.16794745469711,-30.7916975604932,6.98857803382302));
#42228=CARTESIAN_POINT('Ctrl Pts',(4.70571416771088,-31.0299497840783,10.5236751013477));
#42229=CARTESIAN_POINT('Ctrl Pts',(-0.904108400642208,-31.2682020076634,
11.4923483878104));
#42230=CARTESIAN_POINT('Ctrl Pts',(-6.29344475313245,-31.5064542312485,
9.65836614579251));
#42231=CARTESIAN_POINT('Ctrl Pts',(-10.1479896830738,-31.7447064548336,
5.46898426210454));
#42232=CARTESIAN_POINT('Ctrl Pts',(-11.527729775181,-31.9829586784187,-0.0541266785286571));
#42233=CARTESIAN_POINT('Ctrl Pts',(-10.0961858289872,-32.2212109020038,
-5.56403766822958));
#42234=CARTESIAN_POINT('Ctrl Pts',(-6.20247052535459,-32.4594631255889,
-9.71703879013706));
#42235=CARTESIAN_POINT('Ctrl Pts',(-0.79614981493094,-32.6977153491741,
-11.5003316882214));
#42236=CARTESIAN_POINT('Ctrl Pts',(4.80432909580209,-32.9359675727591,-10.4790221588725));
#42237=CARTESIAN_POINT('Ctrl Pts',(9.23316936083815,-33.1742197963443,-6.90217842575973));
#42238=CARTESIAN_POINT('Ctrl Pts',(11.4103033356234,-33.4124720199293,-1.64209051393198));
#42239=CARTESIAN_POINT('Ctrl Pts',(10.8047902268,-33.6507242435144,4.01845637301311));
#42240=CARTESIAN_POINT('Ctrl Pts',(7.56429738698645,-33.8889764670995,8.69901652534074));
#42241=CARTESIAN_POINT('Ctrl Pts',(2.47908846521831,-34.1272286906846,11.2581350075564));
#42242=CARTESIAN_POINT('Ctrl Pts',(-3.21069932579042,-34.3654809142697,
11.0717159152007));
#42243=CARTESIAN_POINT('Ctrl Pts',(-8.11748925481006,-34.6037331378548,
8.18522154028186));
#42244=CARTESIAN_POINT('Ctrl Pts',(-11.0446554057036,-34.8419853614399,
3.30258541734742));
#42245=CARTESIAN_POINT('Ctrl Pts',(-11.2783455590783,-35.080237585025,-2.38545696112353));
#42246=CARTESIAN_POINT('Ctrl Pts',(-8.76156936239957,-35.3184898086102,
-7.49175451923665));
#42247=CARTESIAN_POINT('Ctrl Pts',(-4.10809664364021,-35.5567420321952,
-10.771027130304));
#42248=CARTESIAN_POINT('Ctrl Pts',(1.5472235081241,-35.7949942557803,-11.4235538623753));
#42249=CARTESIAN_POINT('Ctrl Pts',(6.82522004459241,-36.0332464793655,-9.2902020916712));
#42250=CARTESIAN_POINT('Ctrl Pts',(10.4387403400005,-36.2714987029505,-4.89123536487858));
#42251=CARTESIAN_POINT('Ctrl Pts',(11.5065500437207,-36.5097509265356,0.70056394083236));
#42252=CARTESIAN_POINT('Ctrl Pts',(9.76824078653887,-36.7480031501207,6.12151575819658));
#42253=CARTESIAN_POINT('Ctrl Pts',(5.64773670980524,-36.9862553737058,10.0496046291158));
#42254=CARTESIAN_POINT('Ctrl Pts',(0.149910741251658,-37.2245075972909,
11.5268821578289));
#42255=CARTESIAN_POINT('Ctrl Pts',(-5.38447373686177,-37.4627598208761,
10.1930819743391));
#42256=CARTESIAN_POINT('Ctrl Pts',(-9.60573974179206,-37.7010120444611,
6.37348100123998));
#42257=CARTESIAN_POINT('Ctrl Pts',(-11.4844384140878,-37.9392642680463,
0.999568504329265));
#42258=CARTESIAN_POINT('Ctrl Pts',(-10.5624141240384,-38.1775164916313,
-4.61810709638991));
#42259=CARTESIAN_POINT('Ctrl Pts',(-7.06451158493042,-38.4157687152165,
-9.10956451224892));
#42260=CARTESIAN_POINT('Ctrl Pts',(-1.84379075576973,-38.6540209388015,
-11.379446812989));
#42261=CARTESIAN_POINT('Ctrl Pts',(3.82660670829195,-38.8922731623866,-10.8742321871762));
#42262=CARTESIAN_POINT('Ctrl Pts',(8.56374640160554,-39.1305253859717,-7.71705245621344));
#42263=CARTESIAN_POINT('Ctrl Pts',(11.2125487848899,-39.3687776095568,-2.67800538147839));
#42264=CARTESIAN_POINT('Ctrl Pts',(11.1266980751514,-39.6070298331421,3.01433436518149));
#42265=CARTESIAN_POINT('Ctrl Pts',(8.32783221717754,-39.845282056727,7.97115252965823));
#42266=CARTESIAN_POINT('Ctrl Pts',(3.49666957081488,-40.0835548275914,10.9851498170082));
#42267=CARTESIAN_POINT('Ctrl Pts',(-0.291443741763231,-40.2424101905938,
11.2065715437861));
#42268=CARTESIAN_POINT('Ctrl Pts',(-2.09786016577339,-40.3218481457347,
10.8575365576823));
#42269=CARTESIAN_POINT('Ctrl Pts',(-2.71489279974816,-19.033158812699,10.1428239586147));
#42270=CARTESIAN_POINT('Ctrl Pts',(-4.40196321373591,-19.1125762205607,
9.69125195674494));
#42271=CARTESIAN_POINT('Ctrl Pts',(-7.54469310451393,-19.2714110362841,
7.93037237162453));
#42272=CARTESIAN_POINT('Ctrl Pts',(-10.4197874732365,-19.5096632598692,
3.35207403955784));
#42273=CARTESIAN_POINT('Ctrl Pts',(-10.7533286627092,-19.7479154834543,
-2.04257042003514));
#42274=CARTESIAN_POINT('Ctrl Pts',(-8.46466966430815,-19.9861677070394,
-6.9396362376572));
#42275=CARTESIAN_POINT('Ctrl Pts',(-4.11160527360535,-20.2244199306245,
-10.1440525089817));
#42276=CARTESIAN_POINT('Ctrl Pts',(1.24410532515808,-20.4626721542096,-10.8747587183546));
#42277=CARTESIAN_POINT('Ctrl Pts',(6.29644249876465,-20.7009243777947,-8.95335484490964));
#42278=CARTESIAN_POINT('Ctrl Pts',(9.81324307592822,-20.9391766013798,-4.84851683553984));
#42279=CARTESIAN_POINT('Ctrl Pts',(10.936880978813,-21.1774288249649,0.438752574772446));
#42280=CARTESIAN_POINT('Ctrl Pts',(9.39332248927878,-21.41568104855,5.6190144824336));
#42281=CARTESIAN_POINT('Ctrl Pts',(5.55900267879502,-21.6539332721351,9.42896337199362));
#42282=CARTESIAN_POINT('Ctrl Pts',(0.369000022518657,-21.8921854957201,
10.9394553500859));
#42283=CARTESIAN_POINT('Ctrl Pts',(-4.9109907675498,-22.1304377193054,9.78212764297827));
#42284=CARTESIAN_POINT('Ctrl Pts',(-8.99333139197383,-22.3686899428904,
6.23921789037432));
#42285=CARTESIAN_POINT('Ctrl Pts',(-10.8824552492826,-22.6069421664755,
1.17474135199233));
#42286=CARTESIAN_POINT('Ctrl Pts',(-10.1176591483038,-22.8451943900606,
-4.17622117568216));
#42287=CARTESIAN_POINT('Ctrl Pts',(-6.88545493402124,-23.0834466136456,
-8.50872257647364));
#42288=CARTESIAN_POINT('Ctrl Pts',(-1.9740849362557,-23.3216988372308,-10.766189597497));
#42289=CARTESIAN_POINT('Ctrl Pts',(3.41870800044444,-23.5599510608158,-10.398090462909));
#42290=CARTESIAN_POINT('Ctrl Pts',(7.97777569734612,-23.798203284401,-7.49419406141432));
#42291=CARTESIAN_POINT('Ctrl Pts',(10.5912917637341,-24.0364555079861,-2.76267777288981));
#42292=CARTESIAN_POINT('Ctrl Pts',(10.6218942755493,-24.2747077315712,2.64257671518715));
#42293=CARTESIAN_POINT('Ctrl Pts',(8.06212015544694,-24.5129599551563,7.4033822204027));
#42294=CARTESIAN_POINT('Ctrl Pts',(3.53622519869919,-24.7512121787415,10.3587142562468));
#42295=CARTESIAN_POINT('Ctrl Pts',(-1.85205408259982,-24.9894644023266,
10.7878517497922));
#42296=CARTESIAN_POINT('Ctrl Pts',(-6.78867027138654,-25.2277166259116,
8.5861403229883));
#42297=CARTESIAN_POINT('Ctrl Pts',(-10.0697236782791,-25.4659688494967,
4.29051450794865));
#42298=CARTESIAN_POINT('Ctrl Pts',(-10.8950590904933,-25.7042210730818,
-1.05144525036246));
#42299=CARTESIAN_POINT('Ctrl Pts',(-9.06340077411912,-25.9424732966669,
-6.13698754336968));
#42300=CARTESIAN_POINT('Ctrl Pts',(-5.02143787688763,-26.180725520252,-9.72589385858134));
#42301=CARTESIAN_POINT('Ctrl Pts',(0.245110296711381,-26.4189777438371,
-10.9429324516899));
#42302=CARTESIAN_POINT('Ctrl Pts',(5.45188306975753,-26.6572299674222,-9.49130237077641));
#42303=CARTESIAN_POINT('Ctrl Pts',(9.32909727822968,-26.8954821910073,-5.72501473125955));
#42304=CARTESIAN_POINT('Ctrl Pts',(10.9312111172857,-27.1337344145924,-0.562559516087659));
#42305=CARTESIAN_POINT('Ctrl Pts',(9.86751478099552,-27.3719866381775,4.73708789728954));
#42306=CARTESIAN_POINT('Ctrl Pts',(6.3974134245917,-27.6102388617627,8.8814948727489));
#42307=CARTESIAN_POINT('Ctrl Pts',(1.367165656213,-27.8484910853478,10.8599589211139));
#42308=CARTESIAN_POINT('Ctrl Pts',(-3.99649476686722,-28.0867433089328,
10.1899891696809));
#42309=CARTESIAN_POINT('Ctrl Pts',(-8.38552426379272,-28.3249955325179,
7.03497210521514));
#42310=CARTESIAN_POINT('Ctrl Pts',(-10.7295638992853,-28.563247756103,2.16432627645773));
#42311=CARTESIAN_POINT('Ctrl Pts',(-10.4569693564742,-28.8014999796881,
-3.23413691385691));
#42312=CARTESIAN_POINT('Ctrl Pts',(-7.63421865853288,-29.0397522032732,
-7.84388648397718));
#42313=CARTESIAN_POINT('Ctrl Pts',(-2.94970007756592,-29.2780044268583,
-10.5407361769574));
#42314=CARTESIAN_POINT('Ctrl Pts',(2.45416610328047,-29.5162566504434,-10.6670013798312));
#42315=CARTESIAN_POINT('Ctrl Pts',(7.25953126718375,-29.7545088740285,-8.19188961599172));
#42316=CARTESIAN_POINT('Ctrl Pts',(10.2945041010277,-29.9927610976136,-3.71900995074453));
#42317=CARTESIAN_POINT('Ctrl Pts',(10.8189414152284,-30.2310133211987,1.66083001949865));
#42318=CARTESIAN_POINT('Ctrl Pts',(8.70494792777857,-30.4692655447839,6.63564098444718));
#42319=CARTESIAN_POINT('Ctrl Pts',(4.46806627059647,-30.7075177683689,9.9922086398038));
#42320=CARTESIAN_POINT('Ctrl Pts',(-0.858449133521731,-30.945769991954,
10.911962004377));
#42321=CARTESIAN_POINT('Ctrl Pts',(-5.97561331291237,-31.1840222155391,
9.17059950245109));
#42322=CARTESIAN_POINT('Ctrl Pts',(-9.63549608015401,-31.4222744391242,
5.19278971162398));
#42323=CARTESIAN_POINT('Ctrl Pts',(-10.9455565615224,-31.6605266627093,
-0.0513931739272948));
#42324=CARTESIAN_POINT('Ctrl Pts',(-9.58630842342817,-31.8987788862944,
-5.28304273224449));
#42325=CARTESIAN_POINT('Ctrl Pts',(-5.88923346404332,-32.1370311098795,
-9.22630906190571));
#42326=CARTESIAN_POINT('Ctrl Pts',(-0.755942670475671,-32.3752833334646,
-10.919542132286));
#42327=CARTESIAN_POINT('Ctrl Pts',(4.56170094926121,-32.6135355570497,-9.94981075947233));
#42328=CARTESIAN_POINT('Ctrl Pts',(8.76687599832148,-32.8517877806348,-6.55360472792545));
#42329=CARTESIAN_POINT('Ctrl Pts',(10.8340603900244,-33.09004000422,-1.55916168663833));
#42330=CARTESIAN_POINT('Ctrl Pts',(10.2591268939567,-33.3282922278051,3.81551635739438));
#42331=CARTESIAN_POINT('Ctrl Pts',(7.18228536859824,-33.5665444513901,8.25969894026603));
#42332=CARTESIAN_POINT('Ctrl Pts',(2.35388958157973,-33.8047966749752,10.6895768642816));
#42333=CARTESIAN_POINT('Ctrl Pts',(-3.04855264287536,-34.0430488985603,
10.5125723057673));
#42334=CARTESIAN_POINT('Ctrl Pts',(-7.70753995009214,-34.2813011221453,
7.77185162083141));
#42335=CARTESIAN_POINT('Ctrl Pts',(-10.4868784056621,-34.5195533457305,
3.13579830459444));
#42336=CARTESIAN_POINT('Ctrl Pts',(-10.7087667428733,-34.7578055693156,
-2.26498665411725));
#42337=CARTESIAN_POINT('Ctrl Pts',(-8.31909273500825,-34.9960577929007,
-7.11340605952559));
#42338=CARTESIAN_POINT('Ctrl Pts',(-3.90062961659408,-35.2343100164858,
-10.2270689007874));
#42339=CARTESIAN_POINT('Ctrl Pts',(1.46908565274932,-35.4725622400709,-10.846641738899));
#42340=CARTESIAN_POINT('Ctrl Pts',(6.48053289761904,-35.710814463656,-8.82102846314895));
#42341=CARTESIAN_POINT('Ctrl Pts',(9.91156325233417,-35.9490666872412,-4.64421827941024));
#42342=CARTESIAN_POINT('Ctrl Pts',(10.9254464485013,-36.1873189108262,0.665184072570199));
#42343=CARTESIAN_POINT('Ctrl Pts',(9.27492525595335,-36.4255711344113,5.81236707316378));
#42344=CARTESIAN_POINT('Ctrl Pts',(5.36251480624159,-36.6638233579963,9.54207966652283));
#42345=CARTESIAN_POINT('Ctrl Pts',(0.142339951538634,-36.9020755815815,
10.9447517505275));
#42346=CARTESIAN_POINT('Ctrl Pts',(-5.11254713549418,-37.1403278051666,
9.67831112129032));
#42347=CARTESIAN_POINT('Ctrl Pts',(-9.12063083621321,-37.3785800287517,
6.05160757177495));
#42348=CARTESIAN_POINT('Ctrl Pts',(-10.9044515000132,-37.6168322523368,
0.949088312670873));
#42349=CARTESIAN_POINT('Ctrl Pts',(-10.0289912650274,-37.8550844759219,
-4.38488353010602));
#42350=CARTESIAN_POINT('Ctrl Pts',(-6.707739740644,-38.093336699507,-8.64951343970004));
#42351=CARTESIAN_POINT('Ctrl Pts',(-1.75067566628252,-38.3315889230921,
-10.8047621829729));
#42352=CARTESIAN_POINT('Ctrl Pts',(3.63335548118823,-38.5698411466772,-10.3250618976272));
#42353=CARTESIAN_POINT('Ctrl Pts',(8.13126022602624,-38.8080933702623,-7.32732600390901));
#42354=CARTESIAN_POINT('Ctrl Pts',(10.6462928362593,-39.0463455938474,-2.54276079910738));
#42355=CARTESIAN_POINT('Ctrl Pts',(10.5647777576085,-39.2845978174325,2.86210450217782));
#42356=CARTESIAN_POINT('Ctrl Pts',(7.90726017574041,-39.5228500410176,7.56859351975284));
#42357=CARTESIAN_POINT('Ctrl Pts',(3.32008082343409,-39.7611228118819,10.430377967198));
#42358=CARTESIAN_POINT('Ctrl Pts',(-0.276725254858005,-39.9199781748845,
10.6406174576843));
#42359=CARTESIAN_POINT('Ctrl Pts',(-1.99191406724981,-39.9994161300253,
10.309209430531));
#42360=CARTESIAN_POINT('Ctrl Pts',(-1.99079507083261,-40.,10.3105642903746));
#42361=CARTESIAN_POINT('Ctrl Pts',(-1.74787308387827,-40.,10.3776190639041));
#42362=CARTESIAN_POINT('Ctrl Pts',(-1.50291730396267,-40.,10.4356201925428));
#42363=CARTESIAN_POINT('Ctrl Pts',(-1.25645144932134,-40.,10.4847082098124));
#42364=CARTESIAN_POINT('Ctrl Pts',(-1.00610937592225,-40.,10.5345682443401));
#42365=CARTESIAN_POINT('Ctrl Pts',(-0.754208864891479,-40.,10.5752327782703));
#42366=CARTESIAN_POINT('Ctrl Pts',(-0.501269405627775,-40.,10.6068040933286));
#42367=CARTESIAN_POINT('Ctrl Pts',(-0.244349089886426,-40.,10.6388722896344));
#42368=CARTESIAN_POINT('Ctrl Pts',(0.0136436911868619,-40.,10.6615589819356));
#42369=CARTESIAN_POINT('Ctrl Pts',(0.272186557320881,-40.,10.6749225226571));
#42370=CARTESIAN_POINT('Ctrl Pts',(0.531566238246189,-40.,10.6883293165871));
#42371=CARTESIAN_POINT('Ctrl Pts',(0.791500205704512,-40.,10.6923526126214));
#42372=CARTESIAN_POINT('Ctrl Pts',(1.05147390013315,-40.,10.6870004794339));
#42373=CARTESIAN_POINT('Ctrl Pts',(1.31028376057683,-40.,10.6816723063417));
#42374=CARTESIAN_POINT('Ctrl Pts',(1.56913364179828,-40.,10.6670525037355));
#42375=CARTESIAN_POINT('Ctrl Pts',(1.82751901150857,-40.,10.6430977083202));
#42376=CARTESIAN_POINT('Ctrl Pts',(1.90159764111365,-40.,10.63622991074));
#42377=CARTESIAN_POINT('Ctrl Pts',(1.97563807578317,-40.,10.6285944888747));
#42378=CARTESIAN_POINT('Ctrl Pts',(2.04962835769163,-40.,10.6201896290691));
#42379=CARTESIAN_POINT('Ctrl Pts',(2.08954125923063,-40.,10.6156557587659));
#42380=CARTESIAN_POINT('Ctrl Pts',(2.12944528573599,-40.,10.6108972103674));
#42381=CARTESIAN_POINT('Ctrl Pts',(2.1693057513364,-40.,10.6059179310049));
#42382=CARTESIAN_POINT('Ctrl Pts',(2.43279869411486,-40.,10.5730029875293));
#42383=CARTESIAN_POINT('Ctrl Pts',(2.69461388759026,-40.,10.5304238386819));
#42384=CARTESIAN_POINT('Ctrl Pts',(2.95420990430362,-40.,10.4782725649795));
#42385=CARTESIAN_POINT('Ctrl Pts',(3.07376860221232,-40.,10.4542539438269));
#42386=CARTESIAN_POINT('Ctrl Pts',(3.19285681334827,-40.,10.4282042572862));
#42387=CARTESIAN_POINT('Ctrl Pts',(3.31142253876288,-40.,10.4001289044428));
#42388=CARTESIAN_POINT('Ctrl Pts',(3.56622266861186,-40.,10.3397944062138));
#42389=CARTESIAN_POINT('Ctrl Pts',(3.81860986323782,-40.,10.2701083948083));
#42390=CARTESIAN_POINT('Ctrl Pts',(4.06816673278712,-40.,10.1914106777717));
#42391=CARTESIAN_POINT('Ctrl Pts',(4.32019405273534,-40.,10.1119339046154));
#42392=CARTESIAN_POINT('Ctrl Pts',(4.56933530406408,-40.,10.0232659758112));
#42393=CARTESIAN_POINT('Ctrl Pts',(4.815156586397,-40.,9.92570343373692));
#42394=CARTESIAN_POINT('Ctrl Pts',(5.06195033757761,-40.,9.82775493430386));
#42395=CARTESIAN_POINT('Ctrl Pts',(5.30539839959129,-40.,9.72084110382949));
#42396=CARTESIAN_POINT('Ctrl Pts',(5.54504887007903,-40.,9.60521113342298));
#42397=CARTESIAN_POINT('Ctrl Pts',(5.66474353971471,-40.,9.54745914537295));
#42398=CARTESIAN_POINT('Ctrl Pts',(5.78349062335036,-40.,9.48753209533787));
#42399=CARTESIAN_POINT('Ctrl Pts',(5.90123190287221,-40.,9.42545655152217));
#42400=CARTESIAN_POINT('Ctrl Pts',(5.95755289783563,-40.,9.39576300305053));
#42401=CARTESIAN_POINT('Ctrl Pts',(6.01364372866714,-40.,9.36557780581555));
#42402=CARTESIAN_POINT('Ctrl Pts',(6.06949789365341,-40.,9.33490363661388));
#42403=CARTESIAN_POINT('Ctrl Pts',(6.10987237433491,-40.,9.31273065001283));
#42404=CARTESIAN_POINT('Ctrl Pts',(6.15013052671072,-40.,9.29029793926035));
#42405=CARTESIAN_POINT('Ctrl Pts',(6.19023375294448,-40.,9.26762711136606));
#42406=CARTESIAN_POINT('Ctrl Pts',(6.42530159529298,-40.,9.1347404810909));
#42407=CARTESIAN_POINT('Ctrl Pts',(6.6551974805836,-40.,8.99359845953242));
#42408=CARTESIAN_POINT('Ctrl Pts',(6.87949236004535,-40.,8.84456214268246));
#42409=CARTESIAN_POINT('Ctrl Pts',(7.1090735464645,-40.,8.69201325470042));
#42410=CARTESIAN_POINT('Ctrl Pts',(7.33278726191541,-40.,8.53119349946645));
#42411=CARTESIAN_POINT('Ctrl Pts',(7.55016317409375,-40.,8.36243515486996));
#42412=CARTESIAN_POINT('Ctrl Pts',(7.76753908627209,-40.,8.19367681027347));
#42413=CARTESIAN_POINT('Ctrl Pts',(7.97857784575597,-40.,8.01697958779349));
#42414=CARTESIAN_POINT('Ctrl Pts',(8.18278913651048,-40.,7.83262450231714));
#42415=CARTESIAN_POINT('Ctrl Pts',(8.38288054194601,-40.,7.65198871075115));
#42416=CARTESIAN_POINT('Ctrl Pts',(8.57641773083012,-40.,7.46400053667575));
#42417=CARTESIAN_POINT('Ctrl Pts',(8.76315973735505,-40.,7.26911327773004));
#42418=CARTESIAN_POINT('Ctrl Pts',(8.95087399746834,-40.,7.07321135775353));
#42419=CARTESIAN_POINT('Ctrl Pts',(9.13172256231602,-40.,6.87033788456684));
#42420=CARTESIAN_POINT('Ctrl Pts',(9.30542514585722,-40.,6.66091475526788));
#42421=CARTESIAN_POINT('Ctrl Pts',(9.35096602916371,-40.,6.60600875387947));
#42422=CARTESIAN_POINT('Ctrl Pts',(9.39601551124977,-40.,6.55065236459227));
#42423=CARTESIAN_POINT('Ctrl Pts',(9.44056808201162,-40.,6.49485281517297));
#42424=CARTESIAN_POINT('Ctrl Pts',(9.45871046836229,-40.,6.47213051281313));
#42425=CARTESIAN_POINT('Ctrl Pts',(9.4767704796353,-40.,6.44933463079931));
#42426=CARTESIAN_POINT('Ctrl Pts',(9.49473878095482,-40.,6.42647721576431));
#42427=CARTESIAN_POINT('Ctrl Pts',(9.66342503031444,-40.,6.21189201131205));
#42428=CARTESIAN_POINT('Ctrl Pts',(9.82423055529978,-40.,5.99163828046608));
#42429=CARTESIAN_POINT('Ctrl Pts',(9.97696748002078,-40.,5.76623949569044));
#42430=CARTESIAN_POINT('Ctrl Pts',(10.1322964813989,-40.,5.53701550015035));
#42431=CARTESIAN_POINT('Ctrl Pts',(10.2792811504091,-40.,5.30246996694981));
#42432=CARTESIAN_POINT('Ctrl Pts',(10.417694044428,-40.,5.06310861338164));
#42433=CARTESIAN_POINT('Ctrl Pts',(10.5565955438655,-40.,4.82290230056891));
#42434=CARTESIAN_POINT('Ctrl Pts',(10.6868650567645,-40.,4.5778456180751));
#42435=CARTESIAN_POINT('Ctrl Pts',(10.8082364611378,-40.,4.32841151149382));
#42436=CARTESIAN_POINT('Ctrl Pts',(10.9290278826149,-40.,4.08016934560317));
#42437=CARTESIAN_POINT('Ctrl Pts',(11.0410063972023,-40.,3.82759096037244));
#42438=CARTESIAN_POINT('Ctrl Pts',(11.1438680903661,-40.,3.57111254742491));
#42439=CARTESIAN_POINT('Ctrl Pts',(11.2102577344974,-40.,3.4055746290881));
#42440=CARTESIAN_POINT('Ctrl Pts',(11.2728486827081,-40.,3.2384114695089));
#42441=CARTESIAN_POINT('Ctrl Pts',(11.3315488558307,-40.,3.06973522608137));
#42442=CARTESIAN_POINT('Ctrl Pts',(11.3969138737467,-40.,2.88190740399589));
#42443=CARTESIAN_POINT('Ctrl Pts',(11.4574546537082,-40.,2.69220336876743));
#42444=CARTESIAN_POINT('Ctrl Pts',(11.5131538719282,-40.,2.50080739873));
#42445=CARTESIAN_POINT('Ctrl Pts',(11.5219564527078,-40.,2.47055960457812));
#42446=CARTESIAN_POINT('Ctrl Pts',(11.5306367798565,-40.,2.44027394775998));
#42447=CARTESIAN_POINT('Ctrl Pts',(11.5391927173603,-40.,2.40995901899243));
#42448=CARTESIAN_POINT('Ctrl Pts',(11.6149930718682,-40.,2.14138735791641));
#42449=CARTESIAN_POINT('Ctrl Pts',(11.6810877877354,-40.,1.87033611873909));
#42450=CARTESIAN_POINT('Ctrl Pts',(11.7375427831218,-40.,1.59736118879834));
#42451=CARTESIAN_POINT('Ctrl Pts',(11.7945063358724,-40.,1.3219272486335));
#42452=CARTESIAN_POINT('Ctrl Pts',(11.8416558786766,-40.,1.04453424293325));
#42453=CARTESIAN_POINT('Ctrl Pts',(11.8790117308312,-40.,0.765729000453357));
#42454=CARTESIAN_POINT('Ctrl Pts',(11.9165716379187,-40.,0.485400794856042));
#42455=CARTESIAN_POINT('Ctrl Pts',(11.944230718393,-40.,0.203644274650995));
#42456=CARTESIAN_POINT('Ctrl Pts',(11.9619595695781,-40.,-0.0790002471504572));
#42457=CARTESIAN_POINT('Ctrl Pts',(11.9657577576826,-40.,-0.139553356276698));
#42458=CARTESIAN_POINT('Ctrl Pts',(11.9690999836388,-40.,-0.200147259763613));
#42459=CARTESIAN_POINT('Ctrl Pts',(11.9719856511623,-40.,-0.260776694674977));
#42460=CARTESIAN_POINT('Ctrl Pts',(11.9737712450156,-40.,-0.298292986980646));
#42461=CARTESIAN_POINT('Ctrl Pts',(11.9753819638708,-40.,-0.335822485014977));
#42462=CARTESIAN_POINT('Ctrl Pts',(11.9768172604587,-40.,-0.373350238049461));
#42463=CARTESIAN_POINT('Ctrl Pts',(11.9877545329118,-40.,-0.659319885686147));
#42464=CARTESIAN_POINT('Ctrl Pts',(11.9885197420998,-40.,-0.945390292321779));
#42465=CARTESIAN_POINT('Ctrl Pts',(11.9791433269757,-40.,-1.23099730766991));
#42466=CARTESIAN_POINT('Ctrl Pts',(11.9697517430852,-40.,-1.51706636592596));
#42467=CARTESIAN_POINT('Ctrl Pts',(11.9501858036918,-40.,-1.80267116614139));
#42468=CARTESIAN_POINT('Ctrl Pts',(11.9204255171557,-40.,-2.08725729207421));
#42469=CARTESIAN_POINT('Ctrl Pts',(11.8946825397073,-40.,-2.33342744279288));
#42470=CARTESIAN_POINT('Ctrl Pts',(11.8613109472889,-40.,-2.57883581882763));
#42471=CARTESIAN_POINT('Ctrl Pts',(11.8202663870092,-40.,-2.82312554759088));
#42472=CARTESIAN_POINT('Ctrl Pts',(11.8016841988292,-40.,-2.93372333885434));
#42473=CARTESIAN_POINT('Ctrl Pts',(11.7815289081037,-40.,-3.04409183784577));
#42474=CARTESIAN_POINT('Ctrl Pts',(11.7598151666302,-40.,-3.15420275595777));
#42475=CARTESIAN_POINT('Ctrl Pts',(-3.14788895504392,-20.,11.7604951161383));
#42476=CARTESIAN_POINT('Ctrl Pts',(-3.41583726409301,-20.,11.6689078365353));
#42477=CARTESIAN_POINT('Ctrl Pts',(-3.6800281171579,-20.,11.5679423474188));
#42478=CARTESIAN_POINT('Ctrl Pts',(-3.9400576560663,-20.,11.4579525320777));
#42479=CARTESIAN_POINT('Ctrl Pts',(-4.20217416505819,-20.,11.3470799498977));
#42480=CARTESIAN_POINT('Ctrl Pts',(-4.46006282884733,-20.,11.227037265788));
#42481=CARTESIAN_POINT('Ctrl Pts',(-4.71328870843099,-20.,11.0981380891977));
#42482=CARTESIAN_POINT('Ctrl Pts',(-4.96683786875418,-20.,10.9690743535142));
#42483=CARTESIAN_POINT('Ctrl Pts',(-5.2157128452745,-20.,10.8311311125707));
#42484=CARTESIAN_POINT('Ctrl Pts',(-5.45944793382123,-20.,10.6845799114082));
#42485=CARTESIAN_POINT('Ctrl Pts',(-5.70414316174853,-20.,10.5374514048592));
#42486=CARTESIAN_POINT('Ctrl Pts',(-5.9436584643848,-20.,10.381646622191));
#42487=CARTESIAN_POINT('Ctrl Pts',(-6.17748537864976,-20.,10.2174023572803));
#42488=CARTESIAN_POINT('Ctrl Pts',(-6.35285556434856,-20.,10.0942191585973));
#42489=CARTESIAN_POINT('Ctrl Pts',(-6.52502531464269,-20.,9.96628793637483));
#42490=CARTESIAN_POINT('Ctrl Pts',(-6.69376370895902,-20.,9.83369652465032));
#42491=CARTESIAN_POINT('Ctrl Pts',(-6.82031750469622,-20.,9.73425296585697));
#42492=CARTESIAN_POINT('Ctrl Pts',(-6.94494088192704,-20.,9.63218783302566));
#42493=CARTESIAN_POINT('Ctrl Pts',(-7.06753052957085,-20.,9.52753487822875));
#42494=CARTESIAN_POINT('Ctrl Pts',(-7.10083026081442,-20.,9.49910739405238));
#42495=CARTESIAN_POINT('Ctrl Pts',(-7.13398139806579,-20.,9.4704876398804));
#42496=CARTESIAN_POINT('Ctrl Pts',(-7.16697685341455,-20.,9.44168058852786));
#42497=CARTESIAN_POINT('Ctrl Pts',(-7.1942855680072,-20.,9.4178384097997));
#42498=CARTESIAN_POINT('Ctrl Pts',(-7.22148095877947,-20.,9.39387375783253));
#42499=CARTESIAN_POINT('Ctrl Pts',(-7.24855699713369,-20.,9.36979178770966));
#42500=CARTESIAN_POINT('Ctrl Pts',(-7.45693217509727,-20.,9.18445873623375));
#42501=CARTESIAN_POINT('Ctrl Pts',(-7.65835188614669,-20.,8.99208370432816));
#42502=CARTESIAN_POINT('Ctrl Pts',(-7.85239628226539,-20.,8.79294161273235));
#42503=CARTESIAN_POINT('Ctrl Pts',(-7.93912888539186,-20.,8.70393047743737));
#42504=CARTESIAN_POINT('Ctrl Pts',(-8.02438754698256,-20.,8.61356687371931));
#42505=CARTESIAN_POINT('Ctrl Pts',(-8.10813234606881,-20.,8.52187300942612));
#42506=CARTESIAN_POINT('Ctrl Pts',(-8.29599191369487,-20.,8.31618179172622));
#42507=CARTESIAN_POINT('Ctrl Pts',(-8.47623651864014,-20.,8.10379842051384));
#42508=CARTESIAN_POINT('Ctrl Pts',(-8.64862143631681,-20.,7.8852104092871));
#42509=CARTESIAN_POINT('Ctrl Pts',(-8.82101815484727,-20.,7.66660743430834));
#42510=CARTESIAN_POINT('Ctrl Pts',(-8.9855543755666,-20.,7.44179836760427));
#42511=CARTESIAN_POINT('Ctrl Pts',(-9.14193907461982,-20.,7.21124696766876));
#42512=CARTESIAN_POINT('Ctrl Pts',(-9.2972524856338,-20.,6.9822749227384));
#42513=CARTESIAN_POINT('Ctrl Pts',(-9.44452587993939,-20.,6.74763835305147));
#42514=CARTESIAN_POINT('Ctrl Pts',(-9.58342512212373,-20.,6.50777699481686));
#42515=CARTESIAN_POINT('Ctrl Pts',(-9.65196330375271,-20.,6.38942025594683));
#42516=CARTESIAN_POINT('Ctrl Pts',(-9.71846176210418,-20.,6.26979121078749));
#42517=CARTESIAN_POINT('Ctrl Pts',(-9.78287566835972,-20.,6.14894204251706));
#42518=CARTESIAN_POINT('Ctrl Pts',(-9.81320887096953,-20.,6.09203286685191));
#42519=CARTESIAN_POINT('Ctrl Pts',(-9.84307976388747,-20.,6.03485311689594));
#42520=CARTESIAN_POINT('Ctrl Pts',(-9.87248341770164,-20.,5.97740823116596));
#42521=CARTESIAN_POINT('Ctrl Pts',(-9.88901621100681,-20.,5.94510869355695));
#42522=CARTESIAN_POINT('Ctrl Pts',(-9.90540128490397,-20.,5.9127253338552));
#42523=CARTESIAN_POINT('Ctrl Pts',(-9.92163774063042,-20.,5.88025911881517));
#42524=CARTESIAN_POINT('Ctrl Pts',(-9.93566445788436,-20.,5.85221146935616));
#42525=CARTESIAN_POINT('Ctrl Pts',(-9.94957694946133,-20.,5.82410855096149));
#42526=CARTESIAN_POINT('Ctrl Pts',(-9.96337153280794,-20.,5.79595784393402));
#42527=CARTESIAN_POINT('Ctrl Pts',(-10.0085819469324,-20.,5.70369662149397));
#42528=CARTESIAN_POINT('Ctrl Pts',(-10.0525370764346,-20.,5.6108998857053));
#42529=CARTESIAN_POINT('Ctrl Pts',(-10.0952260546702,-20.,5.51759231250541));
#42530=CARTESIAN_POINT('Ctrl Pts',(-10.2089718864923,-20.,5.2689719901745));
#42531=CARTESIAN_POINT('Ctrl Pts',(-10.3137316499186,-20.,5.01672676215728));
#42532=CARTESIAN_POINT('Ctrl Pts',(-10.4092650117527,-20.,4.76131291979556));
#42533=CARTESIAN_POINT('Ctrl Pts',(-10.5040506852791,-20.,4.50789806438331));
#42534=CARTESIAN_POINT('Ctrl Pts',(-10.5897539783247,-20.,4.25136340977421));
#42535=CARTESIAN_POINT('Ctrl Pts',(-10.6660911528296,-20.,3.99214067649283));
#42536=CARTESIAN_POINT('Ctrl Pts',(-10.7164100464605,-20.,3.82126978393892));
#42537=CARTESIAN_POINT('Ctrl Pts',(-10.76265835388,-20.,3.64923065339804));
#42538=CARTESIAN_POINT('Ctrl Pts',(-10.8047424783443,-20.,3.47614542570932));
#42539=CARTESIAN_POINT('Ctrl Pts',(-10.8705314538897,-20.,3.20556596239269));
#42540=CARTESIAN_POINT('Ctrl Pts',(-10.9261465394823,-20.,2.93242944986049));
#42541=CARTESIAN_POINT('Ctrl Pts',(-10.971539533839,-20.,2.65731524077356));
#42542=CARTESIAN_POINT('Ctrl Pts',(-11.0169325281957,-20.,2.38220103168662));
#42543=CARTESIAN_POINT('Ctrl Pts',(-11.0521033806315,-20.,2.10510839212968));
#42544=CARTESIAN_POINT('Ctrl Pts',(-11.0769480123086,-20.,1.82662914162098));
#42545=CARTESIAN_POINT('Ctrl Pts',(-11.0805510773543,-20.,1.78624299838922));
#42546=CARTESIAN_POINT('Ctrl Pts',(-11.0839368669433,-20.,1.74582772459025));
#42547=CARTESIAN_POINT('Ctrl Pts',(-11.0871049669885,-20.,1.70538516141017));
#42548=CARTESIAN_POINT('Ctrl Pts',(-11.0904162776532,-20.,1.6631144348383));
#42549=CARTESIAN_POINT('Ctrl Pts',(-11.093490147485,-20.,1.62080741465348));
#42550=CARTESIAN_POINT('Ctrl Pts',(-11.0963238911948,-20.,1.57850150671815));
#42551=CARTESIAN_POINT('Ctrl Pts',(-11.1141911417012,-20.,1.31175534601939));
#42552=CARTESIAN_POINT('Ctrl Pts',(-11.1225356031101,-20.,1.04484600136718));
#42553=CARTESIAN_POINT('Ctrl Pts',(-11.1214040387022,-20.,0.778285111147121));
#42554=CARTESIAN_POINT('Ctrl Pts',(-11.1202704089919,-20.,0.511237700808428));
#42555=CARTESIAN_POINT('Ctrl Pts',(-11.1096260686144,-20.,0.244539371965727));
#42556=CARTESIAN_POINT('Ctrl Pts',(-11.0894661186613,-20.,-0.0212930845089499));
#42557=CARTESIAN_POINT('Ctrl Pts',(-11.0694226013899,-20.,-0.285590240256897));
#42558=CARTESIAN_POINT('Ctrl Pts',(-11.0399729544248,-20.,-0.549032107069646));
#42559=CARTESIAN_POINT('Ctrl Pts',(-11.0010625247024,-20.,-0.811099100987041));
#42560=CARTESIAN_POINT('Ctrl Pts',(-10.962784322418,-20.,-1.06890795781023));
#42561=CARTESIAN_POINT('Ctrl Pts',(-10.9153500989546,-20.,-1.32538677921543));
#42562=CARTESIAN_POINT('Ctrl Pts',(-10.8586617972334,-20.,-1.58002123156791));
#42563=CARTESIAN_POINT('Ctrl Pts',(-10.8242835539937,-20.,-1.73444260025203));
#42564=CARTESIAN_POINT('Ctrl Pts',(-10.7865010252999,-20.,-1.88818524302589));
#42565=CARTESIAN_POINT('Ctrl Pts',(-10.7452842897659,-20.,-2.04112961510651));
#42566=CARTESIAN_POINT('Ctrl Pts',(-10.6983394263361,-20.,-2.21532955031828));
#42567=CARTESIAN_POINT('Ctrl Pts',(-10.6469394936606,-20.,-2.38849410088828));
#42568=CARTESIAN_POINT('Ctrl Pts',(-10.5911391151801,-20.,-2.5604596881072));
#42569=CARTESIAN_POINT('Ctrl Pts',(-10.5808112700642,-20.,-2.59228803763508));
#42570=CARTESIAN_POINT('Ctrl Pts',(-10.5703323195386,-20.,-2.6240761705273));
#42571=CARTESIAN_POINT('Ctrl Pts',(-10.5597080024052,-20.,-2.65580723494851));
#42572=CARTESIAN_POINT('Ctrl Pts',(-10.4761217376019,-20.,-2.90544974089913));
#42573=CARTESIAN_POINT('Ctrl Pts',(-10.3834680471006,-20.,-3.1517916819884));
#42574=CARTESIAN_POINT('Ctrl Pts',(-10.2820203829828,-20.,-3.39437485165505));
#42575=CARTESIAN_POINT('Ctrl Pts',(-10.1805768302642,-20.,-3.63694819008265));
#42576=CARTESIAN_POINT('Ctrl Pts',(-10.070339637341,-20.,-3.87576361218799));
#42577=CARTESIAN_POINT('Ctrl Pts',(-9.9515383732788,-20.,-4.1103350805885));
#42578=CARTESIAN_POINT('Ctrl Pts',(-9.8329461967683,-20.,-4.3444937084824));
#42579=CARTESIAN_POINT('Ctrl Pts',(-9.70581969060581,-20.,-4.5744238409605));
#42580=CARTESIAN_POINT('Ctrl Pts',(-9.57034919815825,-20.,-4.79960611605748));
#42581=CARTESIAN_POINT('Ctrl Pts',(-9.54674783670939,-20.,-4.83883686048325));
#42582=CARTESIAN_POINT('Ctrl Pts',(-9.52289211519482,-20.,-4.87792504279439));
#42583=CARTESIAN_POINT('Ctrl Pts',(-9.49878621049929,-20.,-4.9168625054116));
#42584=CARTESIAN_POINT('Ctrl Pts',(-9.47147256286588,-20.,-4.96098132804441));
#42585=CARTESIAN_POINT('Ctrl Pts',(-9.44384413272872,-20.,-5.00489628904724));
#42586=CARTESIAN_POINT('Ctrl Pts',(-9.41590688798062,-20.,-5.04859740776055));
#42587=CARTESIAN_POINT('Ctrl Pts',(-9.27645734814993,-20.,-5.26673276611845));
#42588=CARTESIAN_POINT('Ctrl Pts',(-9.12928197945513,-20.,-5.47959888543939));
#42589=CARTESIAN_POINT('Ctrl Pts',(-8.97460596288743,-20.,-5.68672989182249));
#42590=CARTESIAN_POINT('Ctrl Pts',(-8.82197250195883,-20.,-5.89112565447157));
#42591=CARTESIAN_POINT('Ctrl Pts',(-8.66203475773642,-20.,-6.0899371852121));
#42592=CARTESIAN_POINT('Ctrl Pts',(-8.49497512476503,-20.,-6.28267972759005));
#42593=CARTESIAN_POINT('Ctrl Pts',(-8.37973300463925,-20.,-6.4156385927988));
#42594=CARTESIAN_POINT('Ctrl Pts',(-8.26110115916421,-20.,-6.54570870297757));
#42595=CARTESIAN_POINT('Ctrl Pts',(-8.13913138220323,-20.,-6.6727188759329));
#42596=CARTESIAN_POINT('Ctrl Pts',(-8.07193084909504,-20.,-6.74269646829574));
#42597=CARTESIAN_POINT('Ctrl Pts',(-8.0037169417772,-20.,-6.81174500263592));
#42598=CARTESIAN_POINT('Ctrl Pts',(-7.93451184210526,-20.,-6.87984615149801));
#42599=CARTESIAN_POINT('Origin',(0.,-40.,-2.22044604925031E-15));
#42600=CARTESIAN_POINT('',(9.46171656752341,-40.,16.3881738217667));
#42601=CARTESIAN_POINT('',(-9.46171656752339,-40.,16.3881738217667));
#42602=CARTESIAN_POINT('',(9.46171656752341,-40.,16.3881738217667));
#42603=CARTESIAN_POINT('',(-18.9234331350468,-40.,4.44089209850063E-15));
#42604=CARTESIAN_POINT('',(-9.46171656752339,-40.,16.3881738217667));
#42605=CARTESIAN_POINT('',(-9.4617165675234,-40.,-16.3881738217667));
#42606=CARTESIAN_POINT('',(-18.9234331350468,-40.,4.44089209850063E-15));
#42607=CARTESIAN_POINT('',(9.46171656752339,-40.,-16.3881738217667));
#42608=CARTESIAN_POINT('',(-9.4617165675234,-40.,-16.3881738217667));
#42609=CARTESIAN_POINT('',(18.9234331350468,-40.,-1.22124532708767E-14));
#42610=CARTESIAN_POINT('',(9.46171656752339,-40.,-16.3881738217667));
#42611=CARTESIAN_POINT('',(18.9234331350468,-40.,-1.22124532708767E-14));
#42612=CARTESIAN_POINT('Origin',(18.9234331350468,-20.,-1.22124532708767E-14));
#42613=CARTESIAN_POINT('',(18.9234331350468,-20.,-1.22124532708767E-14));
#42614=CARTESIAN_POINT('',(9.46171656752341,-20.,16.3881738217667));
#42615=CARTESIAN_POINT('',(18.9234331350468,-20.,-1.22124532708767E-14));
#42616=CARTESIAN_POINT('',(9.46171656752341,-20.,16.3881738217667));
#42617=CARTESIAN_POINT('',(18.9234331350468,-20.,-1.22124532708767E-14));
#42618=CARTESIAN_POINT('Origin',(9.46171656752339,-20.,-16.3881738217667));
#42619=CARTESIAN_POINT('',(9.46171656752339,-20.,-16.3881738217667));
#42620=CARTESIAN_POINT('',(9.46171656752339,-20.,-16.3881738217667));
#42621=CARTESIAN_POINT('',(9.46171656752339,-20.,-16.3881738217667));
#42622=CARTESIAN_POINT('Origin',(-9.4617165675234,-20.,-16.3881738217667));
#42623=CARTESIAN_POINT('',(-9.4617165675234,-20.,-16.3881738217667));
#42624=CARTESIAN_POINT('',(-9.4617165675234,-20.,-16.3881738217667));
#42625=CARTESIAN_POINT('',(-9.4617165675234,-20.,-16.3881738217667));
#42626=CARTESIAN_POINT('Origin',(-18.9234331350468,-20.,4.44089209850063E-15));
#42627=CARTESIAN_POINT('',(-18.9234331350468,-20.,4.44089209850063E-15));
#42628=CARTESIAN_POINT('',(-18.9234331350468,-20.,4.44089209850063E-15));
#42629=CARTESIAN_POINT('',(-18.9234331350468,-20.,4.44089209850063E-15));
#42630=CARTESIAN_POINT('Origin',(-9.46171656752339,-20.,16.3881738217667));
#42631=CARTESIAN_POINT('',(-9.46171656752339,-20.,16.3881738217667));
#42632=CARTESIAN_POINT('',(-9.46171656752339,-20.,16.3881738217667));
#42633=CARTESIAN_POINT('',(-9.46171656752339,-20.,16.3881738217667));
#42634=CARTESIAN_POINT('Origin',(9.46171656752341,-20.,16.3881738217667));
#42635=CARTESIAN_POINT('',(9.46171656752341,-20.,16.3881738217667));
#42636=CARTESIAN_POINT('Origin',(0.,-20.,-2.22044604925031E-15));
#42637=CARTESIAN_POINT('',(0.,0.,0.));
#42638=CARTESIAN_POINT('',(0.,0.,0.));
#42639=CARTESIAN_POINT('',(0.,0.,0.));
#42640=CARTESIAN_POINT('',(0.,0.,0.));
#42641=CARTESIAN_POINT('',(0.,0.,0.));
#42642=CARTESIAN_POINT('',(0.,0.,0.));
#42643=CARTESIAN_POINT('',(0.,0.,0.));
#42644=CARTESIAN_POINT('',(0.,0.,0.));
#42645=CARTESIAN_POINT('',(0.,0.,0.));
#42646=UNCERTAINTY_MEASURE_WITH_UNIT(LENGTH_MEASURE(0.01),#42668,
'DISTANCE_ACCURACY_VALUE',
'Maximum model space distance between geometric entities at asserted c
onnectivities');
#42647=UNCERTAINTY_MEASURE_WITH_UNIT(LENGTH_MEASURE(0.01),#42668,
'DISTANCE_ACCURACY_VALUE',
'Maximum model space distance between geometric entities at asserted c
onnectivities');
#42648=UNCERTAINTY_MEASURE_WITH_UNIT(LENGTH_MEASURE(0.01),#42668,
'DISTANCE_ACCURACY_VALUE',
'Maximum model space distance between geometric entities at asserted c
onnectivities');
#42649=UNCERTAINTY_MEASURE_WITH_UNIT(LENGTH_MEASURE(0.01),#42668,
'DISTANCE_ACCURACY_VALUE',
'Maximum model space distance between geometric entities at asserted c
onnectivities');
#42650=UNCERTAINTY_MEASURE_WITH_UNIT(LENGTH_MEASURE(0.01),#42668,
'DISTANCE_ACCURACY_VALUE',
'Maximum model space distance between geometric entities at asserted c
onnectivities');
#42651=UNCERTAINTY_MEASURE_WITH_UNIT(LENGTH_MEASURE(0.01),#42668,
'DISTANCE_ACCURACY_VALUE',
'Maximum model space distance between geometric entities at asserted c
onnectivities');
#42652=UNCERTAINTY_MEASURE_WITH_UNIT(LENGTH_MEASURE(0.01),#42668,
'DISTANCE_ACCURACY_VALUE',
'Maximum model space distance between geometric entities at asserted c
onnectivities');
#42653=UNCERTAINTY_MEASURE_WITH_UNIT(LENGTH_MEASURE(0.01),#42668,
'DISTANCE_ACCURACY_VALUE',
'Maximum model space distance between geometric entities at asserted c
onnectivities');
#42654=UNCERTAINTY_MEASURE_WITH_UNIT(LENGTH_MEASURE(0.01),#42668,
'DISTANCE_ACCURACY_VALUE',
'Maximum model space distance between geometric entities at asserted c
onnectivities');
#42655=UNCERTAINTY_MEASURE_WITH_UNIT(LENGTH_MEASURE(0.01),#42668,
'DISTANCE_ACCURACY_VALUE',
'Maximum model space distance between geometric entities at asserted c
onnectivities');
#42656=UNCERTAINTY_MEASURE_WITH_UNIT(LENGTH_MEASURE(0.01),#42668,
'DISTANCE_ACCURACY_VALUE',
'Maximum model space distance between geometric entities at asserted c
onnectivities');
#42657=(
GEOMETRIC_REPRESENTATION_CONTEXT(3)
GLOBAL_UNCERTAINTY_ASSIGNED_CONTEXT((#42646))
GLOBAL_UNIT_ASSIGNED_CONTEXT((#42668,#42670,#42671))
REPRESENTATION_CONTEXT('','3D')
);
#42658=(
GEOMETRIC_REPRESENTATION_CONTEXT(3)
GLOBAL_UNCERTAINTY_ASSIGNED_CONTEXT((#42647))
GLOBAL_UNIT_ASSIGNED_CONTEXT((#42668,#42670,#42671))
REPRESENTATION_CONTEXT('','3D')
);
#42659=(
GEOMETRIC_REPRESENTATION_CONTEXT(3)
GLOBAL_UNCERTAINTY_ASSIGNED_CONTEXT((#42648))
GLOBAL_UNIT_ASSIGNED_CONTEXT((#42668,#42670,#42671))
REPRESENTATION_CONTEXT('','3D')
);
#42660=(
GEOMETRIC_REPRESENTATION_CONTEXT(3)
GLOBAL_UNCERTAINTY_ASSIGNED_CONTEXT((#42649))
GLOBAL_UNIT_ASSIGNED_CONTEXT((#42668,#42670,#42671))
REPRESENTATION_CONTEXT('','3D')
);
#42661=(
GEOMETRIC_REPRESENTATION_CONTEXT(3)
GLOBAL_UNCERTAINTY_ASSIGNED_CONTEXT((#42650))
GLOBAL_UNIT_ASSIGNED_CONTEXT((#42668,#42670,#42671))
REPRESENTATION_CONTEXT('','3D')
);
#42662=(
GEOMETRIC_REPRESENTATION_CONTEXT(3)
GLOBAL_UNCERTAINTY_ASSIGNED_CONTEXT((#42651))
GLOBAL_UNIT_ASSIGNED_CONTEXT((#42668,#42670,#42671))
REPRESENTATION_CONTEXT('','3D')
);
#42663=(
GEOMETRIC_REPRESENTATION_CONTEXT(3)
GLOBAL_UNCERTAINTY_ASSIGNED_CONTEXT((#42652))
GLOBAL_UNIT_ASSIGNED_CONTEXT((#42668,#42670,#42671))
REPRESENTATION_CONTEXT('','3D')
);
#42664=(
GEOMETRIC_REPRESENTATION_CONTEXT(3)
GLOBAL_UNCERTAINTY_ASSIGNED_CONTEXT((#42653))
GLOBAL_UNIT_ASSIGNED_CONTEXT((#42668,#42670,#42671))
REPRESENTATION_CONTEXT('','3D')
);
#42665=(
GEOMETRIC_REPRESENTATION_CONTEXT(3)
GLOBAL_UNCERTAINTY_ASSIGNED_CONTEXT((#42654))
GLOBAL_UNIT_ASSIGNED_CONTEXT((#42668,#42670,#42671))
REPRESENTATION_CONTEXT('','3D')
);
#42666=(
GEOMETRIC_REPRESENTATION_CONTEXT(3)
GLOBAL_UNCERTAINTY_ASSIGNED_CONTEXT((#42655))
GLOBAL_UNIT_ASSIGNED_CONTEXT((#42668,#42670,#42671))
REPRESENTATION_CONTEXT('','3D')
);
#42667=(
GEOMETRIC_REPRESENTATION_CONTEXT(3)
GLOBAL_UNCERTAINTY_ASSIGNED_CONTEXT((#42656))
GLOBAL_UNIT_ASSIGNED_CONTEXT((#42668,#42670,#42671))
REPRESENTATION_CONTEXT('','3D')
);
#42668=(
LENGTH_UNIT()
NAMED_UNIT(*)
SI_UNIT(.MILLI.,.METRE.)
);
#42669=(
LENGTH_UNIT()
NAMED_UNIT(*)
SI_UNIT($,.METRE.)
);
#42670=(
NAMED_UNIT(*)
PLANE_ANGLE_UNIT()
SI_UNIT($,.RADIAN.)
);
#42671=(
NAMED_UNIT(*)
SI_UNIT($,.STERADIAN.)
SOLID_ANGLE_UNIT()
);
#42672=SHAPE_DEFINITION_REPRESENTATION(#42682,#42701);
#42673=SHAPE_DEFINITION_REPRESENTATION(#42683,#42702);
#42674=SHAPE_DEFINITION_REPRESENTATION(#42684,#42703);
#42675=SHAPE_DEFINITION_REPRESENTATION(#42685,#42704);
#42676=SHAPE_DEFINITION_REPRESENTATION(#42686,#42705);
#42677=SHAPE_DEFINITION_REPRESENTATION(#42687,#42706);
#42678=SHAPE_DEFINITION_REPRESENTATION(#42688,#42707);
#42679=SHAPE_DEFINITION_REPRESENTATION(#42689,#42708);
#42680=SHAPE_DEFINITION_REPRESENTATION(#42690,#42709);
#42681=SHAPE_DEFINITION_REPRESENTATION(#42691,#42710);
#42682=PRODUCT_DEFINITION_SHAPE('',$,#42712);
#42683=PRODUCT_DEFINITION_SHAPE('',$,#42713);
#42684=PRODUCT_DEFINITION_SHAPE('',$,#42714);
#42685=PRODUCT_DEFINITION_SHAPE('',$,#42715);
#42686=PRODUCT_DEFINITION_SHAPE('',$,#42716);
#42687=PRODUCT_DEFINITION_SHAPE('',$,#42717);
#42688=PRODUCT_DEFINITION_SHAPE('',$,#42718);
#42689=PRODUCT_DEFINITION_SHAPE('',$,#42719);
#42690=PRODUCT_DEFINITION_SHAPE('',$,#42720);
#42691=PRODUCT_DEFINITION_SHAPE('',$,#42721);
#42692=PRODUCT_DEFINITION_SHAPE($,$,#38);
#42693=PRODUCT_DEFINITION_SHAPE($,$,#39);
#42694=PRODUCT_DEFINITION_SHAPE($,$,#40);
#42695=PRODUCT_DEFINITION_SHAPE($,$,#41);
#42696=PRODUCT_DEFINITION_SHAPE($,$,#42);
#42697=PRODUCT_DEFINITION_SHAPE($,$,#43);
#42698=PRODUCT_DEFINITION_SHAPE($,$,#44);
#42699=PRODUCT_DEFINITION_SHAPE($,$,#45);
#42700=PRODUCT_DEFINITION_SHAPE($,$,#46);
#42701=SHAPE_REPRESENTATION('',(#4141,#4459,#4460,#4461,#4462,#4463,#4464,
#4465,#4466,#4467),#42657);
#42702=SHAPE_REPRESENTATION('',(#4142),#42658);
#42703=SHAPE_REPRESENTATION('',(#4196),#42659);
#42704=SHAPE_REPRESENTATION('',(#4231),#42660);
#42705=SHAPE_REPRESENTATION('',(#4235),#42661);
#42706=SHAPE_REPRESENTATION('',(#4264),#42662);
#42707=SHAPE_REPRESENTATION('',(#4301),#42663);
#42708=SHAPE_REPRESENTATION('',(#4305),#42664);
#42709=SHAPE_REPRESENTATION('',(#4317),#42665);
#42710=SHAPE_REPRESENTATION('',(#4430),#42666);
#42711=PRODUCT_DEFINITION_CONTEXT('part definition',#42743,'design');
#42712=PRODUCT_DEFINITION('BR-301','BR-301',#42722,#42711);
#42713=PRODUCT_DEFINITION('Middle_Body','Middle_Body',#42723,#42711);
#42714=PRODUCT_DEFINITION('Cover','Cover',#42724,#42711);
#42715=PRODUCT_DEFINITION('Ball_02','Ball_02',#42725,#42711);
#42716=PRODUCT_DEFINITION('Adapter','Adapter',#42726,#42711);
#42717=PRODUCT_DEFINITION('Screw','Screw',#42727,#42711);
#42718=PRODUCT_DEFINITION('Ball_01','Ball_01',#42728,#42711);
#42719=PRODUCT_DEFINITION('Nut','Nut',#42729,#42711);
#42720=PRODUCT_DEFINITION('Handle','Handle',#42730,#42711);
#42721=PRODUCT_DEFINITION('Adapter_01','Adapter_01',#42731,#42711);
#42722=PRODUCT_DEFINITION_FORMATION('',$,#42745);
#42723=PRODUCT_DEFINITION_FORMATION('',$,#42746);
#42724=PRODUCT_DEFINITION_FORMATION('',$,#42747);
#42725=PRODUCT_DEFINITION_FORMATION('',$,#42748);
#42726=PRODUCT_DEFINITION_FORMATION('',$,#42749);
#42727=PRODUCT_DEFINITION_FORMATION('',$,#42750);
#42728=PRODUCT_DEFINITION_FORMATION('',$,#42751);
#42729=PRODUCT_DEFINITION_FORMATION('',$,#42752);
#42730=PRODUCT_DEFINITION_FORMATION('',$,#42753);
#42731=PRODUCT_DEFINITION_FORMATION('',$,#42754);
#42732=PRODUCT_RELATED_PRODUCT_CATEGORY('BR-301','BR-301',(#42745));
#42733=PRODUCT_RELATED_PRODUCT_CATEGORY('Middle_Body','Middle_Body',(#42746));
#42734=PRODUCT_RELATED_PRODUCT_CATEGORY('Cover','Cover',(#42747));
#42735=PRODUCT_RELATED_PRODUCT_CATEGORY('Ball_02','Ball_02',(#42748));
#42736=PRODUCT_RELATED_PRODUCT_CATEGORY('Adapter','Adapter',(#42749));
#42737=PRODUCT_RELATED_PRODUCT_CATEGORY('Screw','Screw',(#42750));
#42738=PRODUCT_RELATED_PRODUCT_CATEGORY('Ball_01','Ball_01',(#42751));
#42739=PRODUCT_RELATED_PRODUCT_CATEGORY('Nut','Nut',(#42752));
#42740=PRODUCT_RELATED_PRODUCT_CATEGORY('Handle','Handle',(#42753));
#42741=PRODUCT_RELATED_PRODUCT_CATEGORY('Adapter_01','Adapter_01',(#42754));
#42742=APPLICATION_PROTOCOL_DEFINITION('international standard',
'automotive_design',2009,#42743);
#42743=APPLICATION_CONTEXT(
'Core Data for Automotive Mechanical Design Process');
#42744=PRODUCT_CONTEXT('part definition',#42743,'mechanical');
#42745=PRODUCT('BR-301','BR-301',$,(#42744));
#42746=PRODUCT('Middle_Body','Middle_Body',$,(#42744));
#42747=PRODUCT('Cover','Cover',$,(#42744));
#42748=PRODUCT('Ball_02','Ball_02',$,(#42744));
#42749=PRODUCT('Adapter','Adapter',$,(#42744));
#42750=PRODUCT('Screw','Screw',$,(#42744));
#42751=PRODUCT('Ball_01','Ball_01',$,(#42744));
#42752=PRODUCT('Nut','Nut',$,(#42744));
#42753=PRODUCT('Handle','Handle',$,(#42744));
#42754=PRODUCT('Adapter_01','Adapter_01',$,(#42744));
#42755=PRESENTATION_STYLE_ASSIGNMENT((#42757));
#42756=PRESENTATION_STYLE_ASSIGNMENT((#42758));
#42757=SURFACE_STYLE_USAGE(.BOTH.,#42759);
#42758=SURFACE_STYLE_USAGE(.BOTH.,#42760);
#42759=SURFACE_SIDE_STYLE('',(#42761));
#42760=SURFACE_SIDE_STYLE('',(#42762));
#42761=SURFACE_STYLE_FILL_AREA(#42763);
#42762=SURFACE_STYLE_FILL_AREA(#42764);
#42763=FILL_AREA_STYLE('Steel - Satin',(#42765));
#42764=FILL_AREA_STYLE('Opaque(160,160,160)',(#42766));
#42765=FILL_AREA_STYLE_COLOUR('Steel - Satin',#42767);
#42766=FILL_AREA_STYLE_COLOUR('Opaque(160,160,160)',#42768);
#42767=COLOUR_RGB('Steel - Satin', 0.09019608, 0.27058824, 0.51372549);
#42768=COLOUR_RGB('Opaque(160,160,160)', 0.09019608, 0.27058824, 0.51372549);
ENDSEC;
END-ISO-10303-21;
